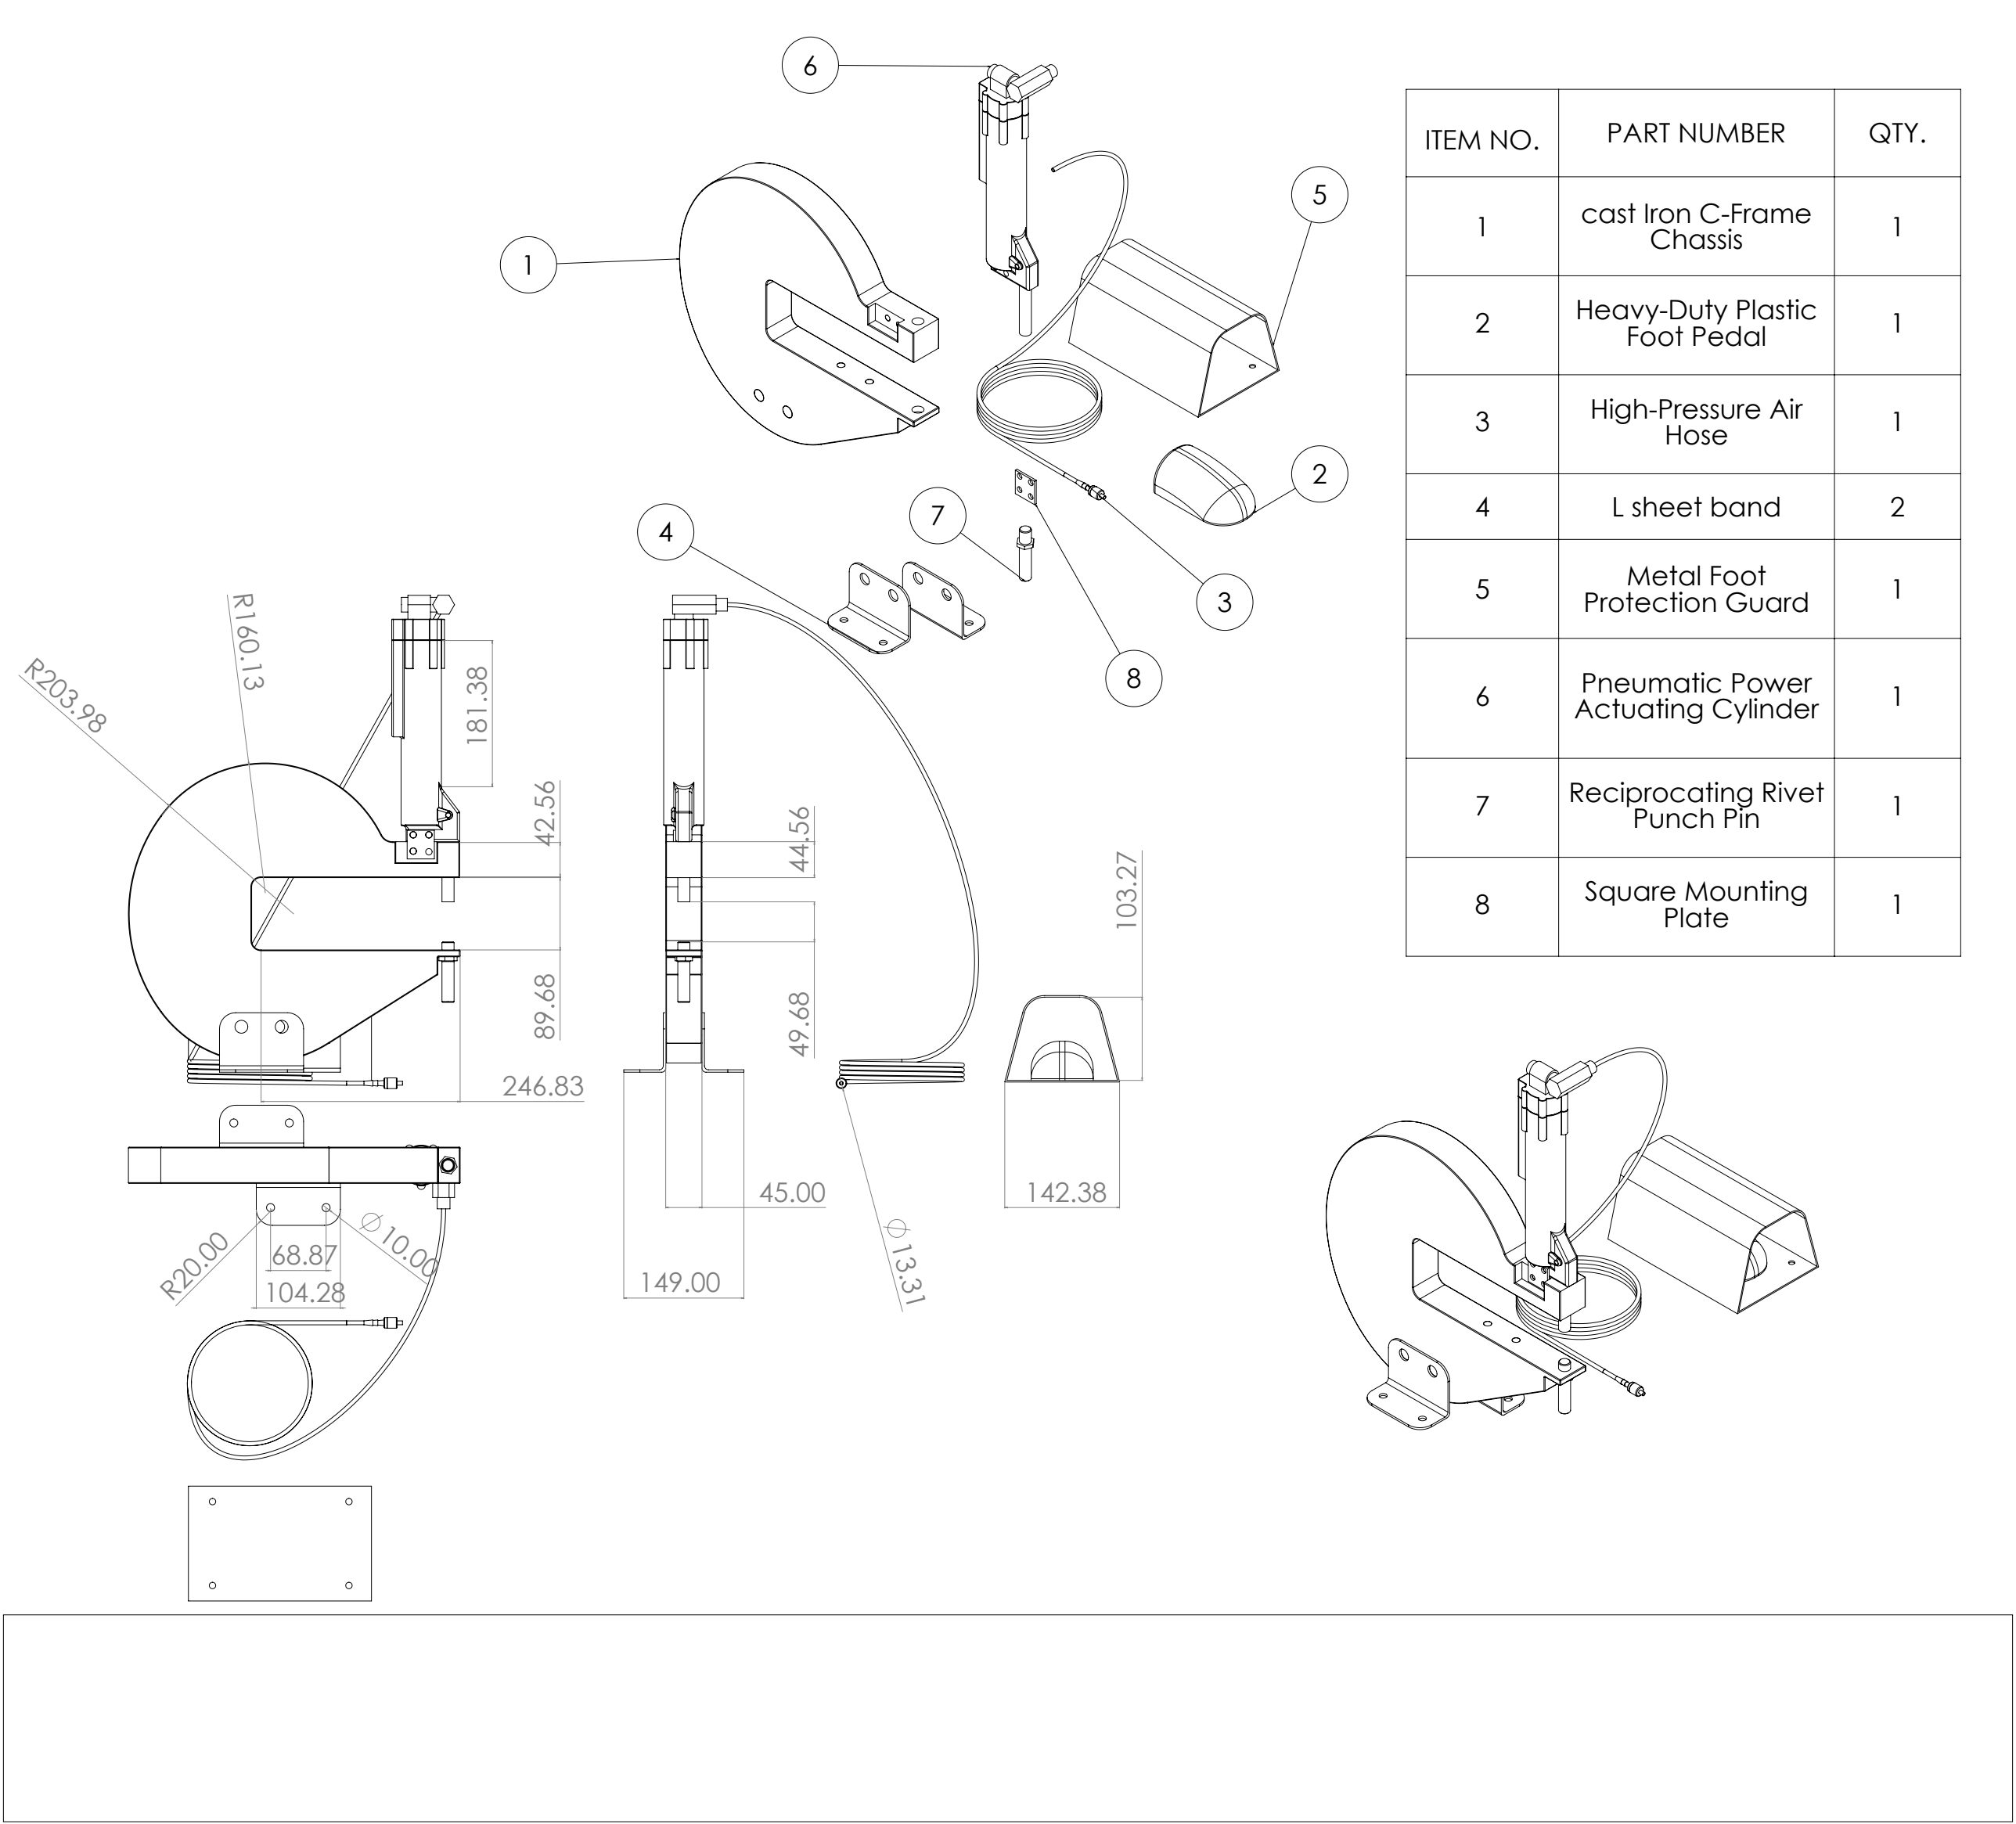
ISO-10303-21;
HEADER;
FILE_DESCRIPTION (('STEP AP214'),
    '1' );
FILE_NAME ('MAS-324',
    '2026-10-25T20:52:49',
    ( '' ),
    ( '' ),
    'SwSTEP 2.0',
    'SolidWorks 2025',
    '' );
FILE_SCHEMA (( 'AUTOMOTIVE_DESIGN' ));
ENDSEC;

DATA;
#1 = CARTESIAN_POINT ( 'NONE',  ( -113.6132551642233466, -295.8660902273127817, -261.0439986488574391 ) ) ;
#2 = CARTESIAN_POINT ( 'NONE',  ( -21.69829453939080111, -272.4952783879842286, -198.0198581616166962 ) ) ;
#3 = CARTESIAN_POINT ( 'NONE',  ( -77.14607672046975040, -275.6695791045739270, -333.3258523244866751 ) ) ;
#4 = CARTESIAN_POINT ( 'NONE',  ( -96.50722556860337420, -298.4744652489187047, -226.7430298893199279 ) ) ;
#5 = CARTESIAN_POINT ( 'NONE',  ( 35.29261755122405475, -294.8217676056252117, -258.4658906454228031 ) ) ;
#6 = DIRECTION ( 'NONE',  ( 0.000000000000000000, 1.000000000000000000, 0.000000000000000000 ) ) ;
#7 = CARTESIAN_POINT ( 'NONE',  ( 17.20777486049739124, -295.0510334597752831, -319.1340501124739717 ) ) ;
#8 = AXIS2_PLACEMENT_3D ( 'NONE', #62573, #33196, #12356 ) ;
#9 = CARTESIAN_POINT ( 'NONE',  ( -147.0026986695708047, -210.7421749798627673, -22.50000000000000000 ) ) ;
#11 = CARTESIAN_POINT ( 'NONE',  ( -84.47810206200919936, -295.7221423797171838, -326.1693894271719500 ) ) ;
#10 = CARTESIAN_POINT ( 'NONE',  ( 23.39288443123379579, -284.9668621146994951, -225.7548735365318748 ) ) ;
#12 = CARTESIAN_POINT ( 'NONE',  ( -83.27587881292458860, -285.4425543175578923, -208.4961557201596918 ) ) ;
#13 = CONICAL_SURFACE ( 'NONE', #77116, 24.00000000000001066, 0.7446590313522313265 ) ;
#14 = CARTESIAN_POINT ( 'NONE',  ( 24.12276456990134577, -287.8361799259163263, -316.7061702643556487 ) ) ;
#15 = CARTESIAN_POINT ( 'NONE',  ( -83.16459577638245548, -297.6555613683490265, -330.2488683299737886 ) ) ;
#16 = CARTESIAN_POINT ( 'NONE',  ( 12.16221636192367228, -290.7420802479286976, -214.1725176534357615 ) ) ;
#17 = CARTESIAN_POINT ( 'NONE',  ( -48.08606759839130973, -279.1160864900698471, -194.2237662435092886 ) ) ;
#18 = CARTESIAN_POINT ( 'NONE',  ( -110.4683760289727132, -293.8380690714490129, -287.0191576251351080 ) ) ;
#19 = LINE ( 'NONE', #14705, #54462 ) ;
#20 = CARTESIAN_POINT ( 'NONE',  ( 26.72141337091415991, -285.8585362577462661, -234.4374339655554991 ) ) ;
#21 = DIRECTION ( 'NONE',  ( -1.000000000000000000, -0.000000000000000000, -0.000000000000000000 ) ) ;
#22 = DIRECTION ( 'NONE',  ( -0.7957555401921980742, -0.6056179655966482667, 0.000000000000000000 ) ) ;
#23 = CARTESIAN_POINT ( 'NONE',  ( -111.0120785373717354, -298.2093386174307170, -265.9889607955867632 ) ) ;
#24 = CARTESIAN_POINT ( 'NONE',  ( -9.095926160855869469, -281.8396501160608523, -199.3626493647371376 ) ) ;
#26 = CARTESIAN_POINT ( 'NONE',  ( 24.14595339631129534, -281.7647060850542289, -309.8413200465337241 ) ) ;
#25 = CARTESIAN_POINT ( 'NONE',  ( -109.2360963732521952, -294.8641011722828580, -247.6139534407837743 ) ) ;
#27 = CARTESIAN_POINT ( 'NONE',  ( -106.5142501024570265, -297.1531912002984086, -236.5357083837597827 ) ) ;
#28 = EDGE_CURVE ( 'NONE', #72058, #65497, #786, .T. ) ;
#29 = CARTESIAN_POINT ( 'NONE',  ( -110.4578234273896271, -280.7667899122553763, -253.6568320815989921 ) ) ;
#30 = CARTESIAN_POINT ( 'NONE',  ( -93.78727130258138800, -296.2704692607680386, -223.6800016881232693 ) ) ;
#31 = VERTEX_POINT ( 'NONE', #14545 ) ;
#32 = DIRECTION ( 'NONE',  ( -0.8457827187922972723, -0.5335274993777825436, 0.000000000000000000 ) ) ;
#33 = CARTESIAN_POINT ( 'NONE',  ( -91.92744132223316456, -285.8159430608695288, -321.2751991526628785 ) ) ;
#34 = CARTESIAN_POINT ( 'NONE',  ( 143.2307367095235691, -26.41817448500847121, 22.50000000000000000 ) ) ;
#35 = CARTESIAN_POINT ( 'NONE',  ( -110.4542110544635705, -294.2666405000204577, -253.6410175316879361 ) ) ;
#36 = CARTESIAN_POINT ( 'NONE',  ( 16.83410871617971338, -275.5019898621288235, -324.9252248568274126 ) ) ;
#37 = CARTESIAN_POINT ( 'NONE',  ( -6.039705354571541562, -292.3087031825515965, -204.3989839164147782 ) ) ;
#38 = CARTESIAN_POINT ( 'NONE',  ( 33.63237012736230724, -283.3319559697839054, -290.1951570289018605 ) ) ;
#39 = CARTESIAN_POINT ( 'NONE',  ( 33.67317559943808192, -277.4154469211121636, -290.4904342910287482 ) ) ;
#40 = CARTESIAN_POINT ( 'NONE',  ( -68.83699650705307249, -285.0594432950156829, -339.7618826965099856 ) ) ;
#41 = CARTESIAN_POINT ( 'NONE',  ( 30.69690168102419747, -280.7137460309204471, -297.8907232790041348 ) ) ;
#42 = CARTESIAN_POINT ( 'NONE',  ( -110.7162897014109433, -280.3529109521358009, -285.8907753398488580 ) ) ;
#43 = CARTESIAN_POINT ( 'NONE',  ( -113.8629036840343218, -272.8260555190163927, -261.7875883216721036 ) ) ;
#44 = CARTESIAN_POINT ( 'NONE',  ( 36.88505382238304264, -275.6425748523263906, -290.8892655207978351 ) ) ;
#45 = CARTESIAN_POINT ( 'NONE',  ( 22.49833801616120255, -296.0810694518352193, -314.6384715069982576 ) ) ;
#46 = DIRECTION ( 'NONE',  ( -0.4999999999999952260, -0.8660254037844413721, 0.000000000000000000 ) ) ;
#47 = FACE_OUTER_BOUND ( 'NONE', #78112, .T. ) ;
#48 = EDGE_CURVE ( 'NONE', #2640, #65773, #51617, .T. ) ;
#49 = CARTESIAN_POINT ( 'NONE',  ( -61.22503046524085590, -293.4984592147682747, -342.3179306570231688 ) ) ;
#50 = CARTESIAN_POINT ( 'NONE',  ( -56.87203779738695175, -273.3011920805299724, -199.9055576269083190 ) ) ;
#51 = CARTESIAN_POINT ( 'NONE',  ( -39.21425765019228038, -293.5492008878248384, -194.0645109205592576 ) ) ;
#53 = CARTESIAN_POINT ( 'NONE',  ( -22.28692340252414539, -293.4457659912081908, -195.1980702719413614 ) ) ;
#52 = CARTESIAN_POINT ( 'NONE',  ( -72.08107566293803359, -300.1233781216987495, -198.2974183793908196 ) ) ;
#54 = CARTESIAN_POINT ( 'NONE',  ( 17.36828252781073800, -290.2692810089828868, -321.4942518745497182 ) ) ;
#55 = CARTESIAN_POINT ( 'NONE',  ( -112.2266234623324124, -276.5486602746883023, -270.6195867653905793 ) ) ;
#56 = CARTESIAN_POINT ( 'NONE',  ( -81.65742486183103210, -279.5809590698107172, -330.1727450829594659 ) ) ;
#57 = CARTESIAN_POINT ( 'NONE',  ( 35.17272386656721750, -291.8502700334059909, -287.2389789927554489 ) ) ;
#58 = CARTESIAN_POINT ( 'NONE',  ( 33.44209198229489743, -283.7601780698271341, -297.3788945958802969 ) ) ;
#59 = CARTESIAN_POINT ( 'NONE',  ( -109.8060437348913467, -283.3224215553644285, -281.7842631819470398 ) ) ;
#60 = ORIENTED_EDGE ( 'NONE', *, *, #32885, .T. ) ;
#61 = CARTESIAN_POINT ( 'NONE',  ( -71.42250952254038054, -283.1821142129608120, -334.9411916729687277 ) ) ;
#62 = CARTESIAN_POINT ( 'NONE',  ( -28.27524738754997813, -281.2441658516256098, -194.1546269278096304 ) ) ;
#63 = CARTESIAN_POINT ( 'NONE',  ( -113.4234760108877538, -283.4592184142248357, -261.4407986698293485 ) ) ;
#64 = CARTESIAN_POINT ( 'NONE',  ( -109.5114376524103363, -279.1602184646021101, -296.6766189074363638 ) ) ;
#65 = ADVANCED_FACE ( 'NONE', ( #14993 ), #6968, .F. ) ;
#66 = CARTESIAN_POINT ( 'NONE',  ( -97.37137399137552052, -279.4367685291730368, -317.4689306191668265 ) ) ;
#67 = CIRCLE ( 'NONE', #92305, 7.500000000000012434 ) ;
#68 = CARTESIAN_POINT ( 'NONE',  ( -6.941161984400275209, -297.1233781216987495, -333.4151289067050357 ) ) ;
#69 = ORIENTED_EDGE ( 'NONE', *, *, #59045, .F. ) ;
#70 = VERTEX_POINT ( 'NONE', #796 ) ;
#71 = CARTESIAN_POINT ( 'NONE',  ( -93.35509533216730915, -299.2464325822394926, -220.4862725388631191 ) ) ;
#72 = AXIS2_PLACEMENT_3D ( 'NONE', #82570, #38996, #88730 ) ;
#73 = CARTESIAN_POINT ( 'NONE',  ( -88.23497865206087454, -275.7892183208580263, -324.9662551183911319 ) ) ;
#74 = CARTESIAN_POINT ( 'NONE',  ( -102.3605472477040337, -292.8335325276641470, -230.9337581368000087 ) ) ;
#75 = CARTESIAN_POINT ( 'NONE',  ( 34.31805428248770795, -292.7103970009527529, -255.9121641687935949 ) ) ;
#76 = CARTESIAN_POINT ( 'NONE',  ( -96.34789938153127764, -289.3946153186523702, -319.7555901667715261 ) ) ;
#77 = DIRECTION ( 'NONE',  ( -0.000000000000000000, 1.000000000000000000, -0.000000000000000000 ) ) ;
#79 = CARTESIAN_POINT ( 'NONE',  ( -33.17331374697837987, -284.5052435883285966, -196.6285636872405860 ) ) ;
#78 = CARTESIAN_POINT ( 'NONE',  ( 36.88326735793300060, -292.3562425583122035, -288.5613484753777129 ) ) ;
#80 = CARTESIAN_POINT ( 'NONE',  ( -69.57500681174269630, -293.4837748164715094, -203.4749671060159528 ) ) ;
#81 = CARTESIAN_POINT ( 'NONE',  ( 22.22138339417639230, -283.4657779623778993, -313.4347628960813381 ) ) ;
#82 = CARTESIAN_POINT ( 'NONE',  ( -28.99082608718071796, -289.8901462222868872, -346.7236095928074064 ) ) ;
#83 = CARTESIAN_POINT ( 'NONE',  ( 34.39346676443356188, -281.8609718709653862, -256.4368729998031426 ) ) ;
#84 = CARTESIAN_POINT ( 'NONE',  ( 39.20951696572362977, -292.3824562929385706, -273.1753459359540557 ) ) ;
#85 = CARTESIAN_POINT ( 'NONE',  ( -4.393016225146153531, -289.4317384794202326, -339.7912944455955540 ) ) ;
#86 = CARTESIAN_POINT ( 'NONE',  ( 37.65823291392757000, -287.8290301222977519, -253.1405899415904912 ) ) ;
#87 = CARTESIAN_POINT ( 'NONE',  ( -52.09100773288315622, -286.0247242745892322, -198.8666571505329728 ) ) ;
#88 = EDGE_LOOP ( 'NONE', ( #36300, #74959 ) ) ;
#89 = DIRECTION ( 'NONE',  ( 0.000000000000000000, -0.000000000000000000, 1.000000000000000000 ) ) ;
#90 = CARTESIAN_POINT ( 'NONE',  ( 3.580403759654407825, -296.3688474698320192, -334.1856371305267430 ) ) ;
#91 = CARTESIAN_POINT ( 'NONE',  ( -113.1662103178394432, -295.1037629167083196, -280.9449385996212527 ) ) ;
#92 = EDGE_CURVE ( 'NONE', #64177, #39404, #21633, .T. ) ;
#93 = CARTESIAN_POINT ( 'NONE',  ( -83.57703501779413102, -278.4588845934780466, -213.5002235206053740 ) ) ;
#94 = CARTESIAN_POINT ( 'NONE',  ( -113.8008141857499993, -272.1671345119243028, -261.7861089057840900 ) ) ;
#95 = CARTESIAN_POINT ( 'NONE',  ( -103.3981541237931054, -294.5919941891141889, -303.1453271309203501 ) ) ;
#96 = CARTESIAN_POINT ( 'NONE',  ( 35.36480375133581333, -277.1321324331269693, -256.5141577024394337 ) ) ;
#97 = CARTESIAN_POINT ( 'NONE',  ( -54.47399014668751249, -271.9692736385993044, -198.1298912440302331 ) ) ;
#98 = CARTESIAN_POINT ( 'NONE',  ( 29.09142378860511258, -294.3365518058123484, -239.0359238687793777 ) ) ;
#99 = CARTESIAN_POINT ( 'NONE',  ( -75.80859898051943446, -296.6581450815154994, -332.8264140846681016 ) ) ;
#100 = CARTESIAN_POINT ( 'NONE',  ( -43.48489315514932230, -254.2578831974578009, -445.7297432066186502 ) ) ;
#101 = CARTESIAN_POINT ( 'NONE',  ( -85.24696079806301441, -293.7120025854050596, -328.2844675371921994 ) ) ;
#102 = CARTESIAN_POINT ( 'NONE',  ( -114.1802237732302245, -273.3548555386022372, -270.3713173946429720 ) ) ;
#103 = CARTESIAN_POINT ( 'NONE',  ( -94.45286519521168600, -275.2254758110098010, -221.7273418318577569 ) ) ;
#104 = CARTESIAN_POINT ( 'NONE',  ( -108.8900272069156472, -291.2871953198740016, -286.0477213144812936 ) ) ;
#105 = CARTESIAN_POINT ( 'NONE',  ( -4.323302397459051427, -294.9377782480969472, -335.5047827706411567 ) ) ;
#106 = CARTESIAN_POINT ( 'NONE',  ( -112.5882073356291926, -280.4803416563776182, -274.4070978670125669 ) ) ;
#107 = CARTESIAN_POINT ( 'NONE',  ( -108.0504587551557307, -277.6107128976585159, -241.1452023711554489 ) ) ;
#108 = CARTESIAN_POINT ( 'NONE',  ( -33.07270939256004993, -282.3483276930217585, -347.1537153405075173 ) ) ;
#109 = CARTESIAN_POINT ( 'NONE',  ( 15.96235870874075324, -274.1327303341880679, -214.9355814682232904 ) ) ;
#110 = CARTESIAN_POINT ( 'NONE',  ( -96.18649800141388084, -277.6093990147008412, -221.9287466249451199 ) ) ;
#111 = CARTESIAN_POINT ( 'NONE',  ( -61.43528157839729431, -277.7399057781236706, -199.1056149990290294 ) ) ;
#112 = CARTESIAN_POINT ( 'NONE',  ( -67.00311722930408109, -296.3398741006864157, -203.1056652694137199 ) ) ;
#113 = CARTESIAN_POINT ( 'NONE',  ( -33.55588428573118165, -276.0999399286864104, -195.4440965705611575 ) ) ;
#114 = PLANE ( 'NONE',  #30765 ) ;
#115 = CARTESIAN_POINT ( 'NONE',  ( 5.580496127948171292, -290.6504686268311843, -208.4249260671794843 ) ) ;
#116 = CARTESIAN_POINT ( 'NONE',  ( -112.2626902172997205, -290.3291827781827692, -288.1895695498705550 ) ) ;
#117 = CARTESIAN_POINT ( 'NONE',  ( -66.84020672111827821, -275.6666780896798059, -201.2245391158463406 ) ) ;
#118 = CARTESIAN_POINT ( 'NONE',  ( -41.95658063400141202, -295.9936855060223024, -195.6702128762018162 ) ) ;
#119 = CARTESIAN_POINT ( 'NONE',  ( -106.5292690430238025, -284.1790909977862043, -236.9359907930603981 ) ) ;
#120 = CARTESIAN_POINT ( 'NONE',  ( -37.35456021389456538, -284.0517986001094073, -195.3485413134038424 ) ) ;
#121 = DIRECTION ( 'NONE',  ( 0.000000000000000000, 0.7071067811865398012, 0.7071067811865552333 ) ) ;
#122 = CARTESIAN_POINT ( 'NONE',  ( 17.04267055929170738, -291.6439787220554649, -220.9968955086508515 ) ) ;
#123 = CARTESIAN_POINT ( 'NONE',  ( -62.96739064857778345, -283.8546313715036717, -200.6342915240590230 ) ) ;
#124 = CARTESIAN_POINT ( 'NONE',  ( 175.2296996224750103, 275.0000000000000568, 0.000000000000000000 ) ) ;
#125 = CARTESIAN_POINT ( 'NONE',  ( 208.4306832106271088, 20.44233620800389772, 0.000000000000000000 ) ) ;
#126 = CARTESIAN_POINT ( 'NONE',  ( 7.902484555432940816, -290.6701741179288092, -210.5450298619024636 ) ) ;
#127 = CARTESIAN_POINT ( 'NONE',  ( -89.97405692109779807, -282.2588973123018832, -325.6834086931719412 ) ) ;
#128 = CARTESIAN_POINT ( 'NONE',  ( -103.8431496891660544, -279.7226268398578668, -302.4792602913342421 ) ) ;
#129 = CARTESIAN_POINT ( 'NONE',  ( -65.74447246362868214, -286.8938844950662883, -199.2042825010933313 ) ) ;
#130 = CARTESIAN_POINT ( 'NONE',  ( -9.493390062269362772, -286.4264726012228266, -202.8681937675485756 ) ) ;
#131 = CARTESIAN_POINT ( 'NONE',  ( -94.04857214285830480, -279.3176295112319281, -317.2818740737955068 ) ) ;
#132 = CARTESIAN_POINT ( 'NONE',  ( -94.07220428401220147, -280.0074554778488505, -224.1631567100062625 ) ) ;
#133 = EDGE_CURVE ( 'NONE', #3915, #71428, #47386, .T. ) ;
#134 = CARTESIAN_POINT ( 'NONE',  ( -96.45200547131824464, -285.9190198393021092, -316.5235751886017397 ) ) ;
#135 = VERTEX_POINT ( 'NONE', #13608 ) ;
#136 = CARTESIAN_POINT ( 'NONE',  ( -46.12776598691637275, -297.7769461629130774, -193.8640261997899188 ) ) ;
#138 = CARTESIAN_POINT ( 'NONE',  ( -23.45499506039496396, -290.8538007153030662, -343.7556936576084468 ) ) ;
#137 = AXIS2_PLACEMENT_3D ( 'NONE', #66421, #57925, #65055 ) ;
#139 = DIRECTION ( 'NONE',  ( -0.000000000000000000, -0.000000000000000000, -1.000000000000000000 ) ) ;
#140 = ADVANCED_BREP_SHAPE_REPRESENTATION ( '', ( #90135, #18940 ), #43137 ) ;
#141 = CARTESIAN_POINT ( 'NONE',  ( -72.02372285203398405, -285.9805209788416391, -342.4524372437778652 ) ) ;
#142 = ORIENTED_EDGE ( 'NONE', *, *, #90775, .T. ) ;
#143 = CARTESIAN_POINT ( 'NONE',  ( 35.52797234631308498, -291.6693239864514453, -248.0799319934128278 ) ) ;
#144 = CARTESIAN_POINT ( 'NONE',  ( -9.246811333089969054, -287.9463490696106192, -202.2197728238365926 ) ) ;
#145 = CARTESIAN_POINT ( 'NONE',  ( 34.64086854919326441, -283.5370289157921775, -287.6338091762179943 ) ) ;
#146 = CARTESIAN_POINT ( 'NONE',  ( 23.68266680496880738, -289.5944490205463921, -316.3462561790806831 ) ) ;
#147 = CARTESIAN_POINT ( 'NONE',  ( -5.814316714654535367, -289.9613947498637572, -340.0699579485100230 ) ) ;
#148 = CARTESIAN_POINT ( 'NONE',  ( -108.8862810617042669, -286.2619989188776231, -292.8638642162096630 ) ) ;
#149 = CARTESIAN_POINT ( 'NONE',  ( -111.7315784639272209, -278.9682992199453224, -250.4319288396881689 ) ) ;
#150 = ORIENTED_EDGE ( 'NONE', *, *, #26082, .T. ) ;
#151 = CARTESIAN_POINT ( 'NONE',  ( 37.80224029141654540, -291.7390338754980235, -278.7595689655631759 ) ) ;
#152 = CARTESIAN_POINT ( 'NONE',  ( 36.17633980381252456, -281.0978762120507781, -247.4679353929731462 ) ) ;
#153 = CARTESIAN_POINT ( 'NONE',  ( -66.31674629447961422, -275.5291285280121656, -202.0141196464570328 ) ) ;
#154 = DIRECTION ( 'NONE',  ( 0.000000000000000000, 1.000000000000000000, 0.000000000000000000 ) ) ;
#155 = CARTESIAN_POINT ( 'NONE',  ( -20.25526795762937127, -294.7662352645559167, -195.3538533559490702 ) ) ;
#156 = CARTESIAN_POINT ( 'NONE',  ( -41.11966117830017708, -272.2452171050537686, -194.4168510268810053 ) ) ;
#157 = CYLINDRICAL_SURFACE ( 'NONE', #21355, 0.5000000000000004441 ) ;
#158 = CARTESIAN_POINT ( 'NONE',  ( -95.65708358510205755, -278.6778134938541598, -226.3255324265030310 ) ) ;
#159 = CARTESIAN_POINT ( 'NONE',  ( 38.33293935469181690, -276.6066984866882876, -258.3872807340205213 ) ) ;
#160 = CARTESIAN_POINT ( 'NONE',  ( -35.81830170358009724, -299.4968625532499118, -196.7715064960510745 ) ) ;
#161 = CARTESIAN_POINT ( 'NONE',  ( -70.37975053163600592, -282.5357189658061543, -339.6670035245268764 ) ) ;
#162 = CARTESIAN_POINT ( 'NONE',  ( -108.6968154583750703, -292.0538962897698525, -290.2073774136056272 ) ) ;
#163 = CARTESIAN_POINT ( 'NONE',  ( -35.86450529380874741, -299.5904438321611565, -194.0540724790644447 ) ) ;
#164 = CARTESIAN_POINT ( 'NONE',  ( -110.4388770307767373, -298.0485552961351345, -247.2764033145294036 ) ) ;
#165 = CARTESIAN_POINT ( 'NONE',  ( -15.02233590537950114, -296.7627049945999715, -341.8430372460552462 ) ) ;
#166 = CARTESIAN_POINT ( 'NONE',  ( -104.6730707308207968, -282.1193390125066003, -303.1377496322695038 ) ) ;
#167 = CARTESIAN_POINT ( 'NONE',  ( -113.9853605009663795, -290.3155259493814242, -262.6348601863189174 ) ) ;
#168 = CARTESIAN_POINT ( 'NONE',  ( -79.76971251359887560, -271.4959503811738273, -208.8840916564036263 ) ) ;
#169 = CARTESIAN_POINT ( 'NONE',  ( 2.307177052818977447, -288.1741521440539486, -205.2887970377841498 ) ) ;
#170 = CARTESIAN_POINT ( 'NONE',  ( -108.0463951965091098, -289.7272753538697998, -250.9943379319703922 ) ) ;
#171 = CARTESIAN_POINT ( 'NONE',  ( 201.3067182052938051, 288.2280244914530840, -97.39779909378675882 ) ) ;
#172 = ORIENTED_EDGE ( 'NONE', *, *, #18686, .T. ) ;
#173 = CARTESIAN_POINT ( 'NONE',  ( -109.8658504693686382, -289.4339475807516351, -246.1362763784779304 ) ) ;
#174 = CARTESIAN_POINT ( 'NONE',  ( -5.787136446112612020, -288.2921266566153236, -336.2124429329496706 ) ) ;
#175 = ORIENTED_EDGE ( 'NONE', *, *, #24191, .T. ) ;
#176 = CARTESIAN_POINT ( 'NONE',  ( -100.7487074920235273, -286.2040526672859073, -227.1274661871449609 ) ) ;
#177 = CARTESIAN_POINT ( 'NONE',  ( -69.25682644265404520, -277.8172129950345379, -336.0522927072145194 ) ) ;
#178 = CARTESIAN_POINT ( 'NONE',  ( 36.06976937112843729, -292.7541342344004534, -292.7275812612277264 ) ) ;
#179 = CARTESIAN_POINT ( 'NONE',  ( -38.72238868582785898, -283.7204533004693872, -347.2467895094548567 ) ) ;
#180 = CARTESIAN_POINT ( 'NONE',  ( -10.92373924738846114, -284.2341409807796140, -342.0049621938744622 ) ) ;
#181 = CARTESIAN_POINT ( 'NONE',  ( -94.38063292225054113, -284.1828072836642036, -322.0750035236984559 ) ) ;
#182 = CARTESIAN_POINT ( 'NONE',  ( 28.99011267871087938, -281.4722031727284275, -239.7083648369550417 ) ) ;
#183 = CARTESIAN_POINT ( 'NONE',  ( 180.6301689436333788, 254.0011452960685006, -166.8208226387889113 ) ) ;
#184 = CARTESIAN_POINT ( 'NONE',  ( 196.3077706885435134, 285.2721524738067274, -111.5570765633820969 ) ) ;
#185 = CARTESIAN_POINT ( 'NONE',  ( -90.09665665672530110, -228.8726286412962736, -344.7822526990161691 ) ) ;
#186 = CARTESIAN_POINT ( 'NONE',  ( -69.55286334857535735, -272.8140695680438057, -204.6721334301478521 ) ) ;
#187 = CARTESIAN_POINT ( 'NONE',  ( -11.36788948023329482, -273.3188565473291192, -201.7533031230518077 ) ) ;
#188 = CARTESIAN_POINT ( 'NONE',  ( -68.20725116294569546, -294.9544458090643957, -340.8369625160823375 ) ) ;
#189 = CARTESIAN_POINT ( 'NONE',  ( 6.867305562803349694, -59.82436178187390396, -351.3599612539230748 ) ) ;
#190 = CARTESIAN_POINT ( 'NONE',  ( -66.02668222974523360, -272.3693846100331939, -199.4212332350789154 ) ) ;
#191 = CARTESIAN_POINT ( 'NONE',  ( -37.17015063146384790, -299.9147455406174458, -196.1229585654807863 ) ) ;
#192 = CARTESIAN_POINT ( 'NONE',  ( 19.90811401000262038, -289.5144666564462455, -316.4447621617657092 ) ) ;
#193 = ORIENTED_EDGE ( 'NONE', *, *, #5103, .F. ) ;
#194 = CARTESIAN_POINT ( 'NONE',  ( -70.69477044455324233, -296.4224833217160153, -339.5159684217153426 ) ) ;
#195 = CARTESIAN_POINT ( 'NONE',  ( 17.81853407656373633, -287.3620640795646182, -222.4514425058484051 ) ) ;
#196 = CARTESIAN_POINT ( 'NONE',  ( -58.02497702157741344, -272.7114924129007250, -196.4567845684104839 ) ) ;
#197 = CARTESIAN_POINT ( 'NONE',  ( 36.21809064911852261, -294.6363344162023736, -292.7476569483883964 ) ) ;
#198 = CARTESIAN_POINT ( 'NONE',  ( -104.5460947458797278, -296.5572545471907802, -307.9279408047181050 ) ) ;
#199 = CARTESIAN_POINT ( 'NONE',  ( -110.3370228416248295, -290.7079322884769113, -271.1874753075676949 ) ) ;
#200 = VERTEX_POINT ( 'NONE', #71848 ) ;
#201 = CARTESIAN_POINT ( 'NONE',  ( -69.54077655466207375, -275.5518863169126007, -201.9910387382556678 ) ) ;
#202 = CARTESIAN_POINT ( 'NONE',  ( 38.34100351736458379, -274.5000774477773575, -282.5315648924769221 ) ) ;
#203 = EDGE_CURVE ( 'NONE', #23354, #33474, #15867, .T. ) ;
#204 = ORIENTED_EDGE ( 'NONE', *, *, #14407, .T. ) ;
#205 = CARTESIAN_POINT ( 'NONE',  ( -104.9245238535658160, -277.5835944543852634, -307.1318786540637120 ) ) ;
#206 = PRODUCT_DEFINITION_CONTEXT ( 'detailed design', #57764, 'design' ) ;
#207 = CARTESIAN_POINT ( 'NONE',  ( 31.87562710300615620, -273.6143523044818266, -244.7602971938240444 ) ) ;
#208 = CARTESIAN_POINT ( 'NONE',  ( -108.8394098029810380, -273.8445740299966928, -254.1653288387956025 ) ) ;
#209 = CARTESIAN_POINT ( 'NONE',  ( -1.618296635492913360, -275.4792631490921053, -206.4151797416647582 ) ) ;
#210 = CARTESIAN_POINT ( 'NONE',  ( -31.36245263867117217, -275.8867941206686396, -194.5969546141441526 ) ) ;
#211 = CIRCLE ( 'NONE', #62253, 4.999999999999997335 ) ;
#212 = CARTESIAN_POINT ( 'NONE',  ( 20.45256449681794564, -274.2372513224178761, -318.7163636411478933 ) ) ;
#213 = CARTESIAN_POINT ( 'NONE',  ( -26.18367686562210039, -295.5577560403836515, -342.6064720533350396 ) ) ;
#214 = CARTESIAN_POINT ( 'NONE',  ( 35.49350546835615461, -291.9893731014084892, -259.8536090943885597 ) ) ;
#215 = DIRECTION ( 'NONE',  ( 0.000000000000000000, 1.000000000000000000, 0.000000000000000000 ) ) ;
#216 = CARTESIAN_POINT ( 'NONE',  ( -102.0418390638001398, -278.4966892230997360, -312.0926700045682196 ) ) ;
#217 = CARTESIAN_POINT ( 'NONE',  ( 34.12090894609900005, -275.5214342262589753, -255.3972326369435280 ) ) ;
#218 = CARTESIAN_POINT ( 'NONE',  ( -26.67319746492361787, -284.8698424366841664, -194.5485961385973042 ) ) ;
#219 = CARTESIAN_POINT ( 'NONE',  ( -69.98802764187368552, -297.4812203234077970, -338.0823389745905843 ) ) ;
#220 = CARTESIAN_POINT ( 'NONE',  ( 211.4629471475955427, 32.98517505407394168, 10.00000000000000000 ) ) ;
#221 = CARTESIAN_POINT ( 'NONE',  ( -95.07820106282620998, -284.3812749118341685, -225.4064025234517032 ) ) ;
#222 = CARTESIAN_POINT ( 'NONE',  ( -62.15031415579434082, -275.6189368971078579, -340.1472874860159550 ) ) ;
#223 = CARTESIAN_POINT ( 'NONE',  ( -95.75169594866139278, -276.5021968402988364, -315.1232370903478568 ) ) ;
#224 = CARTESIAN_POINT ( 'NONE',  ( -110.1547686304307092, -286.7838384147241300, -252.3291687126599356 ) ) ;
#225 = CARTESIAN_POINT ( 'NONE',  ( 5.641680306182056626, -277.6606581397782065, -329.9180858645652279 ) ) ;
#226 = CARTESIAN_POINT ( 'NONE',  ( 219.8344101925596021, 35.72494958537217968, 7.000000000000000000 ) ) ;
#227 = CARTESIAN_POINT ( 'NONE',  ( 16.37664934189118426, -274.7048225403960942, -324.4790114041376796 ) ) ;
#228 = CARTESIAN_POINT ( 'NONE',  ( 34.80913351221764174, -276.3624349405349108, -282.4209052261880402 ) ) ;
#229 = CARTESIAN_POINT ( 'NONE',  ( 2.820361398021606458, -282.5894332162787350, -206.7619648397659091 ) ) ;
#230 = CARTESIAN_POINT ( 'NONE',  ( 201.2509219215139922, 65.09645894978946501, 0.000000000000000000 ) ) ;
#231 = CARTESIAN_POINT ( 'NONE',  ( 34.47262405957937403, -289.1691442991094618, -246.6989133634617701 ) ) ;
#232 = CARTESIAN_POINT ( 'NONE',  ( 21.86556464674976041, -292.1835024172012822, -316.4195789663704090 ) ) ;
#233 = DIRECTION ( 'NONE',  ( -0.000000000000000000, 0.000000000000000000, -1.000000000000000000 ) ) ;
#234 = CARTESIAN_POINT ( 'NONE',  ( -41.87763380309878869, -296.7886418773014725, -197.1043380165232293 ) ) ;
#235 = CARTESIAN_POINT ( 'NONE',  ( -106.8591441079072695, -289.0350993510990065, -244.1732922129692724 ) ) ;
#236 = CARTESIAN_POINT ( 'NONE',  ( -114.4693268140674434, -273.6886850827510216, -284.2063049943780015 ) ) ;
#237 = CARTESIAN_POINT ( 'NONE',  ( 196.8803347170859865, 73.40565171261609123, -12.49999999999998579 ) ) ;
#238 = CARTESIAN_POINT ( 'NONE',  ( -23.45726847500185741, -287.3577760870506950, -345.4476048667748955 ) ) ;
#239 = CARTESIAN_POINT ( 'NONE',  ( -33.75247087138109237, -284.3366009130915018, -194.4592639308252728 ) ) ;
#240 = CARTESIAN_POINT ( 'NONE',  ( -78.69286312455705001, -285.0466963355058851, -331.2335767372052260 ) ) ;
#241 = CARTESIAN_POINT ( 'NONE',  ( -107.9142151825760436, -285.1001298097412473, -289.6988518128527517 ) ) ;
#242 = CARTESIAN_POINT ( 'NONE',  ( -50.30864909105871163, -293.8672956765573758, -196.1299585228881313 ) ) ;
#243 = CARTESIAN_POINT ( 'NONE',  ( -66.22322631712503949, -274.0175736708989689, -198.9914908511120188 ) ) ;
#244 = CARTESIAN_POINT ( 'NONE',  ( -82.02121176197549346, -287.7358496163018913, -331.2959638059363101 ) ) ;
#245 = CARTESIAN_POINT ( 'NONE',  ( -99.64976321348814281, -277.9516674045289619, -315.6240650913662762 ) ) ;
#246 = CARTESIAN_POINT ( 'NONE',  ( 31.35993196141822281, -295.1472400932031519, -241.0411030402186157 ) ) ;
#247 = CARTESIAN_POINT ( 'NONE',  ( -48.18343439339132317, -269.7948820652942459, -438.7219023890238532 ) ) ;
#248 = CARTESIAN_POINT ( 'NONE',  ( 35.78497577281001440, -296.2662352645559167, -287.0191576251351080 ) ) ;
#249 = CARTESIAN_POINT ( 'NONE',  ( -18.62610965303630906, -281.4909754024122890, -341.4840500770574181 ) ) ;
#250 = EDGE_CURVE ( 'NONE', #25460, #78927, #7415, .T. ) ;
#251 = CARTESIAN_POINT ( 'NONE',  ( -39.50340962879238305, -278.0248805946041557, -195.3795613189264202 ) ) ;
#252 = ADVANCED_FACE ( 'NONE', ( #16740 ), #65214, .F. ) ;
#253 = CARTESIAN_POINT ( 'NONE',  ( -97.25653598327876637, -271.6698244868129564, -223.1073329477313791 ) ) ;
#254 = CARTESIAN_POINT ( 'NONE',  ( 34.47519203589411774, -274.7209678462776878, -256.7146287507716806 ) ) ;
#255 = CARTESIAN_POINT ( 'NONE',  ( -0.9307921106466295891, -294.0650048284701370, -206.2765958823960943 ) ) ;
#256 = CARTESIAN_POINT ( 'NONE',  ( 34.55765642826714412, -294.6765038290132566, -284.2855919575040389 ) ) ;
#257 = CARTESIAN_POINT ( 'NONE',  ( 37.74284114224520437, -294.7987799472403481, -256.1865648562181832 ) ) ;
#258 = CARTESIAN_POINT ( 'NONE',  ( 37.27658265588780040, -294.6540076195757933, -253.4083519683468353 ) ) ;
#259 = CARTESIAN_POINT ( 'NONE',  ( -108.8851482201205414, -296.1932415551128202, -284.9332040079801800 ) ) ;
#260 = CARTESIAN_POINT ( 'NONE',  ( -111.3897608342564070, -292.3983347659790866, -282.3532917929296673 ) ) ;
#261 = CARTESIAN_POINT ( 'NONE',  ( -41.56701483115121221, -283.2705272460136712, -347.2974267954927541 ) ) ;
#262 = CARTESIAN_POINT ( 'NONE',  ( -18.82848769330092153, -272.4274859315958111, -196.8388344709858018 ) ) ;
#263 = CARTESIAN_POINT ( 'NONE',  ( 22.99321104538541860, -286.7450741532542224, -222.4997577815586851 ) ) ;
#264 = CARTESIAN_POINT ( 'NONE',  ( -92.15899064099502880, -279.8196800380848686, -321.1009690803662124 ) ) ;
#265 = CARTESIAN_POINT ( 'NONE',  ( -8.150179586038067470, -285.5028795466129736, -203.1951773795938152 ) ) ;
#266 = EDGE_CURVE ( 'NONE', #10377, #27540, #29202, .T. ) ;
#267 = CARTESIAN_POINT ( 'NONE',  ( -77.09840566266530004, -287.5843468112212804, -334.0173477355417617 ) ) ;
#268 = CARTESIAN_POINT ( 'NONE',  ( -45.12257076738355721, -278.0943342815326105, -194.9447721771423971 ) ) ;
#270 = CIRCLE ( 'NONE', #69816, 1.000000000000001998 ) ;
#269 = CARTESIAN_POINT ( 'NONE',  ( -107.8893720497363518, -252.3744610414916565, -325.2219058921743908 ) ) ;
#271 = CARTESIAN_POINT ( 'NONE',  ( -103.0707657646160413, -283.6269096832978107, -302.3783997235955212 ) ) ;
#272 = AXIS2_PLACEMENT_3D ( 'NONE', #89516, #54022, #33648 ) ;
#273 = CARTESIAN_POINT ( 'NONE',  ( 37.16576817676342159, -282.9815768181842373, -288.2116639322431979 ) ) ;
#274 = CARTESIAN_POINT ( 'NONE',  ( -4.444799110440903256, -287.6879362380452108, -339.7341427214811347 ) ) ;
#275 = CARTESIAN_POINT ( 'NONE',  ( -111.3928543446432258, -279.9245025573324597, -288.3842106415503395 ) ) ;
#276 = CARTESIAN_POINT ( 'NONE',  ( -48.40600831671226700, -278.5052016875781078, -346.1172373858461242 ) ) ;
#277 = CARTESIAN_POINT ( 'NONE',  ( -92.20703582126834874, -279.0729676217148949, -222.1882355758204994 ) ) ;
#278 = CARTESIAN_POINT ( 'NONE',  ( -79.81114824688718556, -275.4550972370517457, -208.9127111854542704 ) ) ;
#279 = CARTESIAN_POINT ( 'NONE',  ( 33.32439624573670045, -293.1624354433766939, -239.7783969903679804 ) ) ;
#280 = CARTESIAN_POINT ( 'NONE',  ( -23.50445829584242219, -286.8946535863967711, -343.7650351519840797 ) ) ;
#281 = AXIS2_PLACEMENT_3D ( 'NONE', #4079, #26316, #18275 ) ;
#282 = CARTESIAN_POINT ( 'NONE',  ( -70.56748717621604783, -293.2214596486516598, -201.7864324643425675 ) ) ;
#283 = CARTESIAN_POINT ( 'NONE',  ( -108.4715376898812877, -295.7062291228027675, -252.5679424721457451 ) ) ;
#284 = CARTESIAN_POINT ( 'NONE',  ( -15.59057583108496203, -294.4296390795713592, -340.1206596468418297 ) ) ;
#285 = CARTESIAN_POINT ( 'NONE',  ( -77.02114960951715261, -292.6137018445027707, -204.6718712135360647 ) ) ;
#286 = CARTESIAN_POINT ( 'NONE',  ( 7.197872772093760751, -281.3285238675737787, -212.3305421225269640 ) ) ;
#287 = CARTESIAN_POINT ( 'NONE',  ( -31.92281438307887598, -297.0388370913102563, -193.6711941998320015 ) ) ;
#288 = CARTESIAN_POINT ( 'NONE',  ( -105.0622752010226577, -290.7319065036531924, -306.7923751401537515 ) ) ;
#289 = CARTESIAN_POINT ( 'NONE',  ( -87.52147800885803974, -281.8828391876222099, -327.1964541124606853 ) ) ;
#290 = CARTESIAN_POINT ( 'NONE',  ( -114.1670047289575791, -290.9462267493518084, -265.5013994278262999 ) ) ;
#291 = EDGE_CURVE ( 'NONE', #59112, #73985, #48974, .T. ) ;
#292 = CARTESIAN_POINT ( 'NONE',  ( -17.17010717937488096, -286.6529688014165345, -200.1285271177430332 ) ) ;
#293 = CARTESIAN_POINT ( 'NONE',  ( 169.2494399300530290, -11.64849832608277325, -3.999999999999998224 ) ) ;
#294 = CARTESIAN_POINT ( 'NONE',  ( -113.9112430796897115, -271.1015500560408213, -283.8576724739366455 ) ) ;
#295 = CARTESIAN_POINT ( 'NONE',  ( -39.22682415819677715, -139.9825792601168644, -360.8488084492784083 ) ) ;
#296 = CARTESIAN_POINT ( 'NONE',  ( -94.91159530925413890, -278.3846945089381961, -225.1933234040334071 ) ) ;
#297 = CARTESIAN_POINT ( 'NONE',  ( -67.42059858149401919, -278.5684387154228716, -203.4932414482983347 ) ) ;
#298 = CARTESIAN_POINT ( 'NONE',  ( 18.07732448069620190, -274.4864427186229250, -216.8572984162106252 ) ) ;
#299 = CARTESIAN_POINT ( 'NONE',  ( -92.64007872224544826, -240.2551808938772240, -339.7428190326851905 ) ) ;
#300 = CARTESIAN_POINT ( 'NONE',  ( -95.44584374818370520, -277.8015992959548726, -220.7172953016149393 ) ) ;
#301 = CARTESIAN_POINT ( 'NONE',  ( -68.49327023195247932, -281.4836232829917435, -338.1949331952813509 ) ) ;
#302 = CARTESIAN_POINT ( 'NONE',  ( 10.57689206411022553, -296.1611599144177376, -329.4016677618776612 ) ) ;
#303 = CARTESIAN_POINT ( 'NONE',  ( -37.55642042354166676, -292.5417769992668582, -197.2874406787996691 ) ) ;
#304 = CARTESIAN_POINT ( 'NONE',  ( 23.91132114415732346, -286.7970199167970122, -310.9958052702095870 ) ) ;
#305 = CARTESIAN_POINT ( 'NONE',  ( 25.23911174490946863, -275.6105727896177768, -225.6512951641706479 ) ) ;
#306 = CARTESIAN_POINT ( 'NONE',  ( -91.84630622800007416, -297.4132482821498797, -221.7993231391932341 ) ) ;
#307 = VERTEX_POINT ( 'NONE', #19143 ) ;
#308 = DIRECTION ( 'NONE',  ( 0.000000000000000000, 0.000000000000000000, -1.000000000000000000 ) ) ;
#309 = CARTESIAN_POINT ( 'NONE',  ( 196.7084708347797459, 24.79057925319257194, 12.79847700770043950 ) ) ;
#310 = CARTESIAN_POINT ( 'NONE',  ( -50.70934710825899572, -281.8028321744117193, -195.9929782340904580 ) ) ;
#311 = CARTESIAN_POINT ( 'NONE',  ( -27.53056093681999172, -281.2592550515166749, -197.6600890250774967 ) ) ;
#312 = CARTESIAN_POINT ( 'NONE',  ( -31.17860052041886831, -281.8889978174094040, -194.5728002490756694 ) ) ;
#313 = CARTESIAN_POINT ( 'NONE',  ( -5.942905713229805542, -281.6877908578424581, -336.5377726664386273 ) ) ;
#314 = CARTESIAN_POINT ( 'NONE',  ( 21.24440329897678836, -273.4090717797046182, -225.6371385638898062 ) ) ;
#315 = CARTESIAN_POINT ( 'NONE',  ( 209.2565306692229683, 27.88187848093107846, 12.07105558346639462 ) ) ;
#316 = CARTESIAN_POINT ( 'NONE',  ( 139.6925840978351516, -0.9999999999999859002, -21.50000000000000000 ) ) ;
#317 = CARTESIAN_POINT ( 'NONE',  ( 28.96178146475818593, -276.8614997905642667, -309.1941857057189509 ) ) ;
#318 = DIRECTION ( 'NONE',  ( -0.000000000000000000, -1.000000000000000000, -0.000000000000000000 ) ) ;
#319 = CARTESIAN_POINT ( 'NONE',  ( 4.769913331632007036, -278.4835506822664115, -332.4224800237890918 ) ) ;
#320 = CARTESIAN_POINT ( 'NONE',  ( -39.96107325075033145, -275.6591585686044255, -346.7399479336539230 ) ) ;
#321 = ORIENTED_EDGE ( 'NONE', *, *, #79781, .T. ) ;
#322 = LINE ( 'NONE', #6506, #611 ) ;
#323 = CARTESIAN_POINT ( 'NONE',  ( -52.56024909002068313, -285.2259183838634158, -344.2168985579138507 ) ) ;
#324 = CARTESIAN_POINT ( 'NONE',  ( 28.53551074124957410, -293.1804526957525354, -302.3023540898434476 ) ) ;
#325 = CARTESIAN_POINT ( 'NONE',  ( 26.27770430026630777, -286.3302106616349647, -227.1417106107467703 ) ) ;
#326 = CARTESIAN_POINT ( 'NONE',  ( -87.63360837066642262, -282.0053727907281882, -324.7331695838644805 ) ) ;
#327 = CARTESIAN_POINT ( 'NONE',  ( -34.84458204204858589, -281.5949315533735557, -343.9205063545541066 ) ) ;
#328 = CARTESIAN_POINT ( 'NONE',  ( 25.90896429186087957, -283.2670875563693471, -307.6971038925671564 ) ) ;
#329 = CARTESIAN_POINT ( 'NONE',  ( -24.47694389544438565, -272.2160532552937866, -196.4199350418342647 ) ) ;
#330 = AXIS2_PLACEMENT_3D ( 'NONE', #82535, #75438, #88694 ) ;
#331 = CARTESIAN_POINT ( 'NONE',  ( -110.7265842235424458, -282.6921952033420098, -290.8818197932454837 ) ) ;
#332 = CARTESIAN_POINT ( 'NONE',  ( -58.26820715863784272, -297.3226295211096044, -342.4366403366163922 ) ) ;
#333 = AXIS2_PLACEMENT_3D ( 'NONE', #2350, #57785, #47737 ) ;
#334 = CARTESIAN_POINT ( 'NONE',  ( -85.64834529566002175, -280.3052127297970628, -215.3168041969837248 ) ) ;
#335 = CARTESIAN_POINT ( 'NONE',  ( -5.572524851392624434, -288.4691924952029467, -202.2380827223223321 ) ) ;
#336 = CARTESIAN_POINT ( 'NONE',  ( 197.2699694956033341, 291.3106288012165805, -7.550674042187431212 ) ) ;
#337 = DIRECTION ( 'NONE',  ( -0.000000000000000000, -1.000000000000000000, -0.000000000000000000 ) ) ;
#338 = CARTESIAN_POINT ( 'NONE',  ( 23.63759464484336092, -294.8685903048981345, -225.7422900162428050 ) ) ;
#339 = AXIS2_PLACEMENT_3D ( 'NONE', #18506, #54487, #77693 ) ;
#340 = CARTESIAN_POINT ( 'NONE',  ( -39.23304639640969782, -275.0757377487332178, -345.3372706006049384 ) ) ;
#341 = CARTESIAN_POINT ( 'NONE',  ( -112.9761763116332247, -289.5785814991315874, -283.9848390634267048 ) ) ;
#342 = CARTESIAN_POINT ( 'NONE',  ( 21.95725545762149977, -292.5613560969318314, -314.2937286855417938 ) ) ;
#343 = CARTESIAN_POINT ( 'NONE',  ( -85.44055784739148862, -276.4180553261052182, -325.9960111145832116 ) ) ;
#344 = CARTESIAN_POINT ( 'NONE',  ( -95.72722165873599920, -271.2710829947001230, -224.1827130997946256 ) ) ;
#345 = CARTESIAN_POINT ( 'NONE',  ( -22.65836053330757238, -293.5592278193776679, -198.3497090604275854 ) ) ;
#346 = CARTESIAN_POINT ( 'NONE',  ( -69.85430415644619018, -285.9805209788416391, -337.9475929042657754 ) ) ;
#347 = CARTESIAN_POINT ( 'NONE',  ( -36.30347657727352129, -293.5192792618893236, -346.6737098085878870 ) ) ;
#348 = CARTESIAN_POINT ( 'NONE',  ( -72.72470772363107017, -291.1292060606908194, -335.1259478652599455 ) ) ;
#349 = CARTESIAN_POINT ( 'NONE',  ( -72.93889733817584897, -289.8270235111069155, -203.2136108133159951 ) ) ;
#350 = CARTESIAN_POINT ( 'NONE',  ( 21.65667839415024787, -289.5898385970144204, -314.3659227384940777 ) ) ;
#351 = CARTESIAN_POINT ( 'NONE',  ( 152.0879868122481184, 129.8824796955493355, -12.50000000000000178 ) ) ;
#352 = CARTESIAN_POINT ( 'NONE',  ( -84.78198129953274531, -290.5284216945488538, -326.1237722561434111 ) ) ;
#353 = CARTESIAN_POINT ( 'NONE',  ( 184.7149167944524493, -12.49482340714361506, 10.00000000000000000 ) ) ;
#354 = CARTESIAN_POINT ( 'NONE',  ( 16.41828331231947047, -289.5142829697366551, -325.0047850796670446 ) ) ;
#355 = CARTESIAN_POINT ( 'NONE',  ( -69.24261951150045036, -277.6547478299956424, -202.0774387024998475 ) ) ;
#356 = CARTESIAN_POINT ( 'NONE',  ( -93.06138155620693908, -279.6124719458072718, -217.1712879536569858 ) ) ;
#357 = CARTESIAN_POINT ( 'NONE',  ( -2.906107825339117934, -282.2763205639810167, -339.2229474479840405 ) ) ;
#358 = CARTESIAN_POINT ( 'NONE',  ( 32.85528928337881638, -285.2072911852064863, -243.8063626278319873 ) ) ;
#359 = CARTESIAN_POINT ( 'NONE',  ( 196.0143093133015384, 42.36571313990103960, 11.99999999999998934 ) ) ;
#360 = CARTESIAN_POINT ( 'NONE',  ( 16.70922893827216171, -280.4128521477969116, -321.3210328012327182 ) ) ;
#361 = ADVANCED_FACE ( 'NONE', ( #13917 ), #24780, .F. ) ;
#362 = CARTESIAN_POINT ( 'NONE',  ( -66.39029194718750659, -283.6716376159805009, -201.2150409871211707 ) ) ;
#363 = CARTESIAN_POINT ( 'NONE',  ( 122.1069165698472005, 147.2784710008442062, -260.4370889626021608 ) ) ;
#364 = CARTESIAN_POINT ( 'NONE',  ( -97.39534768318327451, -276.3970167199631760, -317.4383648314011452 ) ) ;
#365 = CARTESIAN_POINT ( 'NONE',  ( -89.66526190333848945, -284.2554813913510543, -214.2198617431564287 ) ) ;
#366 = CARTESIAN_POINT ( 'NONE',  ( -76.65960139014248398, -274.3138574429952996, -208.6626223191690030 ) ) ;
#367 = CARTESIAN_POINT ( 'NONE',  ( -110.4121956192968952, -292.0160383064796861, -280.8026003379728195 ) ) ;
#368 = CARTESIAN_POINT ( 'NONE',  ( -64.70614803693948147, -275.1270252510786349, -199.0042521874292731 ) ) ;
#369 = CARTESIAN_POINT ( 'NONE',  ( 31.13961632253437628, -274.8809954078292321, -245.0155703673037237 ) ) ;
#370 = CARTESIAN_POINT ( 'NONE',  ( -31.41970177568762068, -296.9776604953191281, -345.1784422849063390 ) ) ;
#371 = CARTESIAN_POINT ( 'NONE',  ( -65.44504524589291350, -289.5761160872477262, -342.1056879275396909 ) ) ;
#372 = CARTESIAN_POINT ( 'NONE',  ( 36.45377266294208596, -279.8396616290869474, -286.6547727834441162 ) ) ;
#373 = CARTESIAN_POINT ( 'NONE',  ( 20.38009769833850271, -292.6951850229471574, -219.3785238948976826 ) ) ;
#374 = CARTESIAN_POINT ( 'NONE',  ( -32.12861129292866735, -291.1782324718648169, -197.2989384837379987 ) ) ;
#375 = CARTESIAN_POINT ( 'NONE',  ( -41.85144338877410064, -293.1086862314667201, -345.2764462107752479 ) ) ;
#376 = ORIENTED_EDGE ( 'NONE', *, *, #4713, .F. ) ;
#377 = CARTESIAN_POINT ( 'NONE',  ( 0.000000000000000000, 131.0000000000000568, -11.50000000000000000 ) ) ;
#378 = CARTESIAN_POINT ( 'NONE',  ( -81.76149366879960212, -290.9364281575888072, -212.2895999433750660 ) ) ;
#379 = CARTESIAN_POINT ( 'NONE',  ( 207.5838500149071706, 29.29481134328564451, 13.58522159759120740 ) ) ;
#380 = CARTESIAN_POINT ( 'NONE',  ( -15.49194037015495340, -287.2693386610928314, -196.7164407258930510 ) ) ;
#381 = CARTESIAN_POINT ( 'NONE',  ( -53.35057174420112602, -300.3376638359844719, -200.3683826091709648 ) ) ;
#382 = CARTESIAN_POINT ( 'NONE',  ( -5.905052913589146080, -293.7076358184812648, -340.3936634569377588 ) ) ;
#383 = CARTESIAN_POINT ( 'NONE',  ( -100.9994486081661194, -285.3040589295532072, -312.8942100776160942 ) ) ;
#384 = CARTESIAN_POINT ( 'NONE',  ( -87.69296771485265651, -285.1580413244751639, -217.5051830566009698 ) ) ;
#385 = CARTESIAN_POINT ( 'NONE',  ( 27.23484507803531329, -276.5905825887086280, -234.7502008270885199 ) ) ;
#386 = CARTESIAN_POINT ( 'NONE',  ( 33.90947907481013601, -291.8606329916426034, -292.6123261580082158 ) ) ;
#387 = CARTESIAN_POINT ( 'NONE',  ( 23.78235592887573091, -295.8861003879378586, -312.1859408948212149 ) ) ;
#388 = CARTESIAN_POINT ( 'NONE',  ( 34.27735924785553578, -274.5585016382564731, -286.4756392014268158 ) ) ;
#389 = ORIENTED_EDGE ( 'NONE', *, *, #16197, .T. ) ;
#390 = CARTESIAN_POINT ( 'NONE',  ( 195.6182592083429768, 42.27466702580179714, 12.66657019004900953 ) ) ;
#391 = CARTESIAN_POINT ( 'NONE',  ( 1.755039088397472469, -294.2108378408647127, -336.6724237618244047 ) ) ;
#392 = CARTESIAN_POINT ( 'NONE',  ( 36.55663044536660067, -289.5882713313104659, -279.3249863250336489 ) ) ;
#393 = CARTESIAN_POINT ( 'NONE',  ( 27.34393682368281375, -296.8617045556625271, -195.3831644147898032 ) ) ;
#394 = CARTESIAN_POINT ( 'NONE',  ( -102.0629304562351791, -298.1732284488088567, -229.2192311247754617 ) ) ;
#395 = CARTESIAN_POINT ( 'NONE',  ( -25.13295117268265244, -286.8632252611534454, -198.2345166741048388 ) ) ;
#396 = CARTESIAN_POINT ( 'NONE',  ( -106.1398451837155505, -277.1705574142181945, -304.5341711825586231 ) ) ;
#397 = CARTESIAN_POINT ( 'NONE',  ( -65.55836371735222201, -296.0629673787829006, -341.9094569026487420 ) ) ;
#398 = CARTESIAN_POINT ( 'NONE',  ( -65.01824890676496693, -287.5493471980986442, -340.9453832113689487 ) ) ;
#399 = CARTESIAN_POINT ( 'NONE',  ( -112.8687659414040212, -297.0724226953441871, -255.4135726666953872 ) ) ;
#401 = CARTESIAN_POINT ( 'NONE',  ( -105.7319383130498238, -291.2284431431657481, -244.6273306386740671 ) ) ;
#400 = CIRCLE ( 'NONE', #83570, 2.500000000000007550 ) ;
#402 = CARTESIAN_POINT ( 'NONE',  ( 210.1640492649794396, 37.84931640281016030, 10.50000000000000000 ) ) ;
#403 = AXIS2_PLACEMENT_3D ( 'NONE', #74243, #31178, #30232 ) ;
#404 = DIRECTION ( 'NONE',  ( 0.000000000000000000, -1.000000000000000000, 0.000000000000000000 ) ) ;
#405 = CARTESIAN_POINT ( 'NONE',  ( -110.6395987777366372, -271.3322271728259238, -283.6871839692900039 ) ) ;
#406 = CARTESIAN_POINT ( 'NONE',  ( 36.69934693387597235, -288.8392658573746985, -251.9049237673648918 ) ) ;
#407 = CARTESIAN_POINT ( 'NONE',  ( -99.86837403722181250, -288.6952119285918457, -220.4570493818173702 ) ) ;
#408 = ORIENTED_EDGE ( 'NONE', *, *, #36940, .T. ) ;
#409 = AXIS2_PLACEMENT_3D ( 'NONE', #74640, #9280, #38163 ) ;
#410 = CARTESIAN_POINT ( 'NONE',  ( -110.4501830105272120, -278.2029926013627232, -246.3497191025504947 ) ) ;
#411 = CARTESIAN_POINT ( 'NONE',  ( -77.07960880002397630, -285.5857159168178896, -333.8331689869217485 ) ) ;
#412 = CARTESIAN_POINT ( 'NONE',  ( -111.3091925084824112, -282.8845413066624701, -289.5811479901594794 ) ) ;
#414 = CARTESIAN_POINT ( 'NONE',  ( 30.73219615365270485, -286.0310267411410905, -300.6096502203043315 ) ) ;
#413 = VECTOR ( 'NONE', #28280, 1000.000000000000000 ) ;
#415 = CARTESIAN_POINT ( 'NONE',  ( 9.776714872701816716, -278.2721951864857601, -329.7590680726313508 ) ) ;
#416 = CARTESIAN_POINT ( 'NONE',  ( -110.1599951406477516, -296.9581660565513062, -276.9113938487936366 ) ) ;
#417 = ORIENTED_EDGE ( 'NONE', *, *, #24378, .F. ) ;
#418 = CARTESIAN_POINT ( 'NONE',  ( -61.18891464443646555, -294.0530483757174238, -339.9316314393639686 ) ) ;
#419 = CARTESIAN_POINT ( 'NONE',  ( -71.19720023784525154, -280.2683243496197179, -201.3167996104560018 ) ) ;
#421 = CARTESIAN_POINT ( 'NONE',  ( -104.5325035349209770, -278.2870535611997980, -241.5637464807761603 ) ) ;
#420 = CARTESIAN_POINT ( 'NONE',  ( -95.61175034384609717, -279.1700810579507106, -226.3676360124166536 ) ) ;
#422 = CARTESIAN_POINT ( 'NONE',  ( -15.87710889929866376, -275.4030008116405384, -196.6801677939435820 ) ) ;
#423 = CARTESIAN_POINT ( 'NONE',  ( -82.37591756080814775, -276.5714600047618319, -332.4369729437565866 ) ) ;
#424 = CARTESIAN_POINT ( 'NONE',  ( -113.3918672577102740, -270.6791253856088133, -283.7747343605257129 ) ) ;
#425 = CARTESIAN_POINT ( 'NONE',  ( -67.97318274279425054, -296.8717553275860723, -340.3633934241867678 ) ) ;
#426 = CARTESIAN_POINT ( 'NONE',  ( -69.91165696735023971, -276.1233781216988064, -202.8022627189028810 ) ) ;
#427 = DIRECTION ( 'NONE',  ( -0.000000000000000000, 1.000000000000000000, -0.000000000000000000 ) ) ;
#428 = CARTESIAN_POINT ( 'NONE',  ( 7.103459944063120091, -287.7531359562102580, -211.9972993146364217 ) ) ;
#429 = CARTESIAN_POINT ( 'NONE',  ( -69.38620004629432003, -287.3964490037180326, -201.4475639410760834 ) ) ;
#430 = CARTESIAN_POINT ( 'NONE',  ( 35.06017669879758358, -287.0348881638780085, -280.5447993308172272 ) ) ;
#431 = CARTESIAN_POINT ( 'NONE',  ( 24.20210434625752782, -281.6748354658932953, -316.5334802164283019 ) ) ;
#432 = CARTESIAN_POINT ( 'NONE',  ( -110.7597969522451393, -277.0562332315128629, -262.3744125087495718 ) ) ;
#433 = CARTESIAN_POINT ( 'NONE',  ( -98.53737060242386292, -285.8362405327920328, -312.4739421121791452 ) ) ;
#434 = CARTESIAN_POINT ( 'NONE',  ( -98.55886781794781371, -277.5975963507496544, -229.2441326131148003 ) ) ;
#435 = CARTESIAN_POINT ( 'NONE',  ( -18.87697925039016056, -278.1245800897174263, -341.4968864787559824 ) ) ;
#436 = CARTESIAN_POINT ( 'NONE',  ( 7.363625341111400324, -275.1731506385693251, -212.5733829849779397 ) ) ;
#437 = CARTESIAN_POINT ( 'NONE',  ( -43.16748347093800930, -287.9191015667062175, -346.7421952665334857 ) ) ;
#438 =( BOUNDED_SURFACE ( )  B_SPLINE_SURFACE ( 3, 2, ( 
 ( #50320, #50797, #35669 ),
 ( #87224, #29020, #21923 ),
 ( #65495, #15274, #20984 ),
 ( #42745, #29497, #79681 ) ),
 .UNSPECIFIED., .F., .F., .F. ) 
 B_SPLINE_SURFACE_WITH_KNOTS ( ( 4, 4 ),
 ( 3, 3 ),
 ( 0.000000000000000000, 0.0009274969146595095750 ),
 ( 0.000000000000000000, 1.000000000000000000 ),
 .UNSPECIFIED. ) 
 GEOMETRIC_REPRESENTATION_ITEM ( )  RATIONAL_B_SPLINE_SURFACE ( (
 ( 1.000000000000000000, 0.7691239371209215303, 1.000000000000000000),
 ( 1.000000000000000000, 0.7869877059350417481, 1.000000000000000000),
 ( 1.000000000000000000, 0.8014280003973071054, 1.000000000000000000),
 ( 1.000000000000000000, 0.8108476219622873238, 1.000000000000000000) ) ) 
 REPRESENTATION_ITEM ( '' )  SURFACE ( )  );
#439 = CARTESIAN_POINT ( 'NONE',  ( -34.47473844410745158, -283.8198020982060257, -347.1461383420058269 ) ) ;
#440 = CIRCLE ( 'NONE', #73018, 5.024999999999987921 ) ;
#441 = CARTESIAN_POINT ( 'NONE',  ( 35.55280058431892343, -282.3566568378734019, -295.1421408184978645 ) ) ;
#442 = ORIENTED_EDGE ( 'NONE', *, *, #84617, .T. ) ;
#443 = VERTEX_POINT ( 'NONE', #78317 ) ;
#444 = CARTESIAN_POINT ( 'NONE',  ( 156.6537229343953754, 214.8829733828359849, 16.96953521546817001 ) ) ;
#445 = CARTESIAN_POINT ( 'NONE',  ( 11.63567796159732204, -290.2411052206740578, -328.1670165858570272 ) ) ;
#447 = ADVANCED_FACE ( 'NONE', ( #62233, #49878, #84920, #20557, #27656 ), #19601, .F. ) ;
#446 =( BOUNDED_SURFACE ( )  B_SPLINE_SURFACE ( 3, 2, ( 
 ( #46429, #52604, #66380 ),
 ( #81486, #45029, #45487 ),
 ( #9515, #38403, #9987 ),
 ( #68231, #32242, #60670 ) ),
 .UNSPECIFIED., .F., .F., .F. ) 
 B_SPLINE_SURFACE_WITH_KNOTS ( ( 4, 4 ),
 ( 3, 3 ),
 ( 0.000000000000000000, 0.0009274969146595095750 ),
 ( 0.000000000000000000, 1.000000000000000000 ),
 .UNSPECIFIED. ) 
 GEOMETRIC_REPRESENTATION_ITEM ( )  RATIONAL_B_SPLINE_SURFACE ( (
 ( 1.000000000000000000, 0.7691239371209221964, 1.000000000000000000),
 ( 1.000000000000000000, 0.7869877059350496307, 1.000000000000000000),
 ( 1.000000000000000000, 0.8014280003973005551, 1.000000000000000000),
 ( 1.000000000000000000, 0.8108476219622871017, 1.000000000000000000) ) ) 
 REPRESENTATION_ITEM ( '' )  SURFACE ( )  );
#448 = CARTESIAN_POINT ( 'NONE',  ( -101.2626605397846049, -289.7943000246049223, -228.2255153181214098 ) ) ;
#449 = CARTESIAN_POINT ( 'NONE',  ( 94.78702171985756308, -298.9449283184634965, -197.2183506070807653 ) ) ;
#450 = CARTESIAN_POINT ( 'NONE',  ( -11.09980241159285619, -294.0676480132073607, -342.6995274442535901 ) ) ;
#451 = CARTESIAN_POINT ( 'NONE',  ( 35.64438321566538548, -286.1663195541688651, -280.6380762210182525 ) ) ;
#452 = CARTESIAN_POINT ( 'NONE',  ( 36.05237603647821487, -288.7659386966579405, -271.0245089406109855 ) ) ;
#453 = CARTESIAN_POINT ( 'NONE',  ( 21.27581636871892101, -289.4090924074130839, -223.5744983911110353 ) ) ;
#454 = CARTESIAN_POINT ( 'NONE',  ( 37.35780284020656694, -289.6384337990135691, -277.0681965735167296 ) ) ;
#455 = CARTESIAN_POINT ( 'NONE',  ( -102.9959811661897078, -289.0380696731132275, -233.7613392213682744 ) ) ;
#456 = CARTESIAN_POINT ( 'NONE',  ( -41.38985635712994338, -294.0013616208397025, -195.4577283638537892 ) ) ;
#457 = CARTESIAN_POINT ( 'NONE',  ( -108.9475998404428339, -285.2906192478001230, -285.7830426642873931 ) ) ;
#458 = CARTESIAN_POINT ( 'NONE',  ( -44.74250737014229884, -293.9589824279485128, -195.5080083575545302 ) ) ;
#459 = CARTESIAN_POINT ( 'NONE',  ( 219.8344101925596021, 0.000000000000000000, 7.000000000000000000 ) ) ;
#460 = DIRECTION ( 'NONE',  ( -0.000000000000000000, -1.000000000000000000, -0.000000000000000000 ) ) ;
#461 = CARTESIAN_POINT ( 'NONE',  ( -69.45425524740572598, -275.6116147604159892, -202.1767048456104305 ) ) ;
#462 = CARTESIAN_POINT ( 'NONE',  ( 34.22529250880975127, -280.5486076104474478, -255.1103591393745091 ) ) ;
#463 = CARTESIAN_POINT ( 'NONE',  ( -5.198279291450013773, -280.6290538813578337, -338.1380734097782010 ) ) ;
#464 = CARTESIAN_POINT ( 'NONE',  ( -107.0242423197752260, -295.3340369974355895, -302.7417006471805507 ) ) ;
#465 = CARTESIAN_POINT ( 'NONE',  ( 26.15657362997979973, -273.2749777785776359, -232.2362400515366687 ) ) ;
#466 = CARTESIAN_POINT ( 'NONE',  ( -67.40623058219914299, -275.5294293008589648, -338.4598566561462576 ) ) ;
#467 = CARTESIAN_POINT ( 'NONE',  ( -70.70629809753577888, -298.9177607521856430, -204.8639294649306635 ) ) ;
#468 = AXIS2_PLACEMENT_3D ( 'NONE', #23626, #88479, #15587 ) ;
#469 = CARTESIAN_POINT ( 'NONE',  ( -12.79472286548296189, -296.1521451354898318, -339.7893085137351363 ) ) ;
#470 = EDGE_CURVE ( 'NONE', #443, #38673, #70143, .T. ) ;
#471 = CYLINDRICAL_SURFACE ( 'NONE', #38369, 1.000000000000000888 ) ;
#472 = CARTESIAN_POINT ( 'NONE',  ( -93.19907288353067543, -296.6847407908389300, -317.6304496190813325 ) ) ;
#473 = DIRECTION ( 'NONE',  ( -0.8510748438184358999, -0.5250018354872690862, -0.006684530980050039546 ) ) ;
#474 = AXIS2_PLACEMENT_3D ( 'NONE', #24792, #83000, #69744 ) ;
#476 = CARTESIAN_POINT ( 'NONE',  ( -108.7791315055169292, -296.7511089224530565, -255.2779189747055852 ) ) ;
#475 = CARTESIAN_POINT ( 'NONE',  ( -62.62531095629989153, -283.7448301468398881, -199.3741767513798777 ) ) ;
#477 = VECTOR ( 'NONE', #77768, 1000.000000000000000 ) ;
#478 = CARTESIAN_POINT ( 'NONE',  ( -104.0404571924912176, -285.0535134706426561, -231.7807334197285059 ) ) ;
#479 = CARTESIAN_POINT ( 'NONE',  ( 38.08672107127473794, -287.4111732831478889, -285.7330914080269508 ) ) ;
#480 = CARTESIAN_POINT ( 'NONE',  ( -27.84916182087626524, -290.1726618128096788, -196.0802578231074733 ) ) ;
#481 = AXIS2_PLACEMENT_3D ( 'NONE', #69178, #53570, #82445 ) ;
#482 = CARTESIAN_POINT ( 'NONE',  ( -96.68618260603486192, -278.4065655959097398, -221.5309156116981342 ) ) ;
#483 = CARTESIAN_POINT ( 'NONE',  ( -110.4683760289727132, -275.8380690714489560, -287.0191576251351080 ) ) ;
#484 = VECTOR ( 'NONE', #66979, 1000.000000000000000 ) ;
#485 = DIRECTION ( 'NONE',  ( 0.000000000000000000, 0.000000000000000000, -1.000000000000000000 ) ) ;
#486 = CARTESIAN_POINT ( 'NONE',  ( 15.32504751799938170, -285.6119886687430949, -219.2402396929666111 ) ) ;
#488 = DIRECTION ( 'NONE',  ( 0.000000000000000000, 1.000000000000000000, 0.000000000000000000 ) ) ;
#487 = CARTESIAN_POINT ( 'NONE',  ( -110.1331340237950371, -289.7794927530383688, -246.0517078306988310 ) ) ;
#489 = FACE_OUTER_BOUND ( 'NONE', #65073, .T. ) ;
#490 = CARTESIAN_POINT ( 'NONE',  ( -94.54989721759596932, -297.4992510617885841, -317.0035278207499232 ) ) ;
#491 = CARTESIAN_POINT ( 'NONE',  ( -2.673819891810099048, -281.9266918661726891, -202.2528603128815234 ) ) ;
#493 = CARTESIAN_POINT ( 'NONE',  ( 33.66971584016666696, -281.4439457894184216, -287.4280102006902666 ) ) ;
#492 = CARTESIAN_POINT ( 'NONE',  ( -112.0260394306532987, -294.4391519622371902, -280.7769840364173888 ) ) ;
#494 = CARTESIAN_POINT ( 'NONE',  ( 28.10704333086922801, -294.2504591929128992, -311.0255889924686130 ) ) ;
#495 = VECTOR ( 'NONE', #32367, 1000.000000000000000 ) ;
#496 = ADVANCED_FACE ( 'NONE', ( #85859 ), #33336, .T. ) ;
#497 = CARTESIAN_POINT ( 'NONE',  ( -67.88206223731559419, -281.6514772224624039, -201.8468337845070266 ) ) ;
#498 = CARTESIAN_POINT ( 'NONE',  ( -106.2125426076041634, -295.2784407768329515, -295.4144270085473636 ) ) ;
#499 = ORIENTED_EDGE ( 'NONE', *, *, #5733, .T. ) ;
#500 = CARTESIAN_POINT ( 'NONE',  ( 17.06571399127465583, -89.54582641780471874, -21.50000000000000000 ) ) ;
#501 = VECTOR ( 'NONE', #78144, 1000.000000000000000 ) ;
#502 = CARTESIAN_POINT ( 'NONE',  ( -95.55218877742616712, -285.8860174903883831, -317.1081560315652155 ) ) ;
#503 = CARTESIAN_POINT ( 'NONE',  ( -74.94434090351494149, -285.8906705383787994, 27.50000000000000000 ) ) ;
#504 = CARTESIAN_POINT ( 'NONE',  ( -110.4542110544635705, -282.2666405000204009, -253.6410175316879361 ) ) ;
#505 = CARTESIAN_POINT ( 'NONE',  ( -1.368022843707428438, -273.7141166933243994, -202.4637442224215818 ) ) ;
#506 = CARTESIAN_POINT ( 'NONE',  ( -109.9726748286922628, -290.4821773897211301, -263.0302572872621454 ) ) ;
#507 = CARTESIAN_POINT ( 'NONE',  ( 25.71966169681331849, -282.5511572894125152, -232.1312805657929346 ) ) ;
#508 = CARTESIAN_POINT ( 'NONE',  ( -96.93934988317018053, -274.7561529871699690, -226.7496344372156614 ) ) ;
#509 = AXIS2_PLACEMENT_3D ( 'NONE', #63054, #5739, #91883 ) ;
#510 = CARTESIAN_POINT ( 'NONE',  ( 33.84745103067382388, -283.4999324435455037, -297.5373055610141364 ) ) ;
#511 = CARTESIAN_POINT ( 'NONE',  ( 22.12468463488144010, -280.9459354239748450, -313.4044813569679491 ) ) ;
#512 = CARTESIAN_POINT ( 'NONE',  ( -111.1035872555647188, -280.7265676192138812, -256.7896531230614983 ) ) ;
#513 = CARTESIAN_POINT ( 'NONE',  ( -90.16440307809195076, -273.4969061714966756, -214.2636476280938780 ) ) ;
#514 = CARTESIAN_POINT ( 'NONE',  ( 2.419818390556676135, -274.4029431552878009, -204.4215877325289057 ) ) ;
#515 = CARTESIAN_POINT ( 'NONE',  ( 35.04236977698502642, -295.2468850698101619, -252.9326020219452857 ) ) ;
#516 = CARTESIAN_POINT ( 'NONE',  ( 159.4851178187871312, 15.00000000000000000, 9.000000000000000000 ) ) ;
#517 = CARTESIAN_POINT ( 'NONE',  ( 16.66419048074589782, -292.4339046538751177, -323.5739229754051394 ) ) ;
#518 = CARTESIAN_POINT ( 'NONE',  ( 5.217678648793666163, -274.1526882925118684, -210.9126626711573067 ) ) ;
#519 = CARTESIAN_POINT ( 'NONE',  ( -76.82721684469869672, -293.0540813855774900, -205.0039100937321734 ) ) ;
#521 = CARTESIAN_POINT ( 'NONE',  ( -33.57432131573970224, -293.3036558292391760, -193.8508861434929997 ) ) ;
#520 = CARTESIAN_POINT ( 'NONE',  ( -110.4683760289727132, -275.2662352645559167, -253.7030783399848985 ) ) ;
#522 = CARTESIAN_POINT ( 'NONE',  ( 32.19804620522597105, -289.9147606758254483, -298.1461082847454236 ) ) ;
#523 = CARTESIAN_POINT ( 'NONE',  ( -102.1838148814982645, -276.0511314017147129, -307.8220257815003720 ) ) ;
#524 = CARTESIAN_POINT ( 'NONE',  ( -73.52089337593383789, -279.4562368179799705, -335.4325269178318649 ) ) ;
#525 = CARTESIAN_POINT ( 'NONE',  ( -34.26569199195837712, -293.0930187872357351, -344.7375414908350422 ) ) ;
#526 = CARTESIAN_POINT ( 'NONE',  ( 18.23768133693696214, -282.6996858500997973, -218.8709457477553144 ) ) ;
#527 = EDGE_LOOP ( 'NONE', ( #23564, #43969, #29055, #47901 ) ) ;
#528 = CARTESIAN_POINT ( 'NONE',  ( -66.57193366333181928, -283.1125662302549699, -337.2901694264401158 ) ) ;
#529 = CARTESIAN_POINT ( 'NONE',  ( -79.75134091025527994, -280.5733721980102473, -206.3997167747376125 ) ) ;
#530 = CIRCLE ( 'NONE', #89712, 8.000000000000000000 ) ;
#531 = CARTESIAN_POINT ( 'NONE',  ( 35.22795202031545614, -280.6595075427375150, -295.0545065737637174 ) ) ;
#532 = CARTESIAN_POINT ( 'NONE',  ( -59.58534422498445338, -278.2746395945201812, -343.8324764135672922 ) ) ;
#533 =( NAMED_UNIT ( * ) SI_UNIT ( $, .STERADIAN. ) SOLID_ANGLE_UNIT ( ) );
#534 = CARTESIAN_POINT ( 'NONE',  ( -6.833954875992621858, -278.1790821057300604, -340.3179759246217486 ) ) ;
#535 = CARTESIAN_POINT ( 'NONE',  ( -102.0455923789670294, -281.4805209788416960, -239.2376011013261916 ) ) ;
#536 = EDGE_LOOP ( 'NONE', ( #40735, #1250, #34787, #36151 ) ) ;
#537 = ORIENTED_EDGE ( 'NONE', *, *, #58978, .T. ) ;
#538 = CARTESIAN_POINT ( 'NONE',  ( -94.27891396533529189, -299.2288517735989899, -221.5237939030694179 ) ) ;
#539 = VECTOR ( 'NONE', #13268, 1000.000000000000000 ) ;
#540 = CARTESIAN_POINT ( 'NONE',  ( -51.61964741925273614, -275.2557921787226292, -343.6276657439970563 ) ) ;
#541 = CARTESIAN_POINT ( 'NONE',  ( -39.20955032075062263, -293.7891813239779140, -194.3845451917290461 ) ) ;
#542 = CARTESIAN_POINT ( 'NONE',  ( 29.58004740640543417, -293.2959480609137017, -299.7783302023191254 ) ) ;
#543 = CARTESIAN_POINT ( 'NONE',  ( 32.65864715560118725, -286.6498733850967255, -238.3035732600245922 ) ) ;
#544 = CARTESIAN_POINT ( 'NONE',  ( 186.6539576904058890, 276.0000000000000568, 11.60392986742922616 ) ) ;
#546 = CARTESIAN_POINT ( 'NONE',  ( -108.5382654350417795, -282.6975571727014653, -289.8379683928316126 ) ) ;
#545 = CARTESIAN_POINT ( 'NONE',  ( -22.23194966639039194, -293.4369986843219635, -345.2630654359047639 ) ) ;
#547 = CARTESIAN_POINT ( 'NONE',  ( -64.24683902220084519, -291.2672496188426408, -339.6042094105640672 ) ) ;
#548 = CARTESIAN_POINT ( 'NONE',  ( -108.0627017584748870, -282.7599712521561628, -291.1245075829212965 ) ) ;
#549 = CARTESIAN_POINT ( 'NONE',  ( 25.99246253114274552, -283.3771681065013013, -307.7447886190831241 ) ) ;
#550 = CARTESIAN_POINT ( 'NONE',  ( -45.98732877144905018, -290.1003550732238523, -346.6903779564393062 ) ) ;
#551 = CIRCLE ( 'NONE', #48930, 4.025000000000000355 ) ;
#552 = CARTESIAN_POINT ( 'NONE',  ( -27.55633526468844252, -280.6720254424021164, -197.9066035369142469 ) ) ;
#553 = CARTESIAN_POINT ( 'NONE',  ( -33.47033252515218749, -293.7993959282042056, -346.8792103833187639 ) ) ;
#554 = CARTESIAN_POINT ( 'NONE',  ( -37.49099266878829440, -289.8567683557566852, -347.2125418609350049 ) ) ;
#555 = CARTESIAN_POINT ( 'NONE',  ( 12.38083513092553289, -288.8732566723153354, -329.0739478451774289 ) ) ;
#556 = CARTESIAN_POINT ( 'NONE',  ( -8.256898078943684993, -286.6106324874740494, -203.4053542703483117 ) ) ;
#557 = VERTEX_POINT ( 'NONE', #91558 ) ;
#558 = CARTESIAN_POINT ( 'NONE',  ( 195.4431342809958210, 25.62282010151562162, 12.94565045871722653 ) ) ;
#559 = CARTESIAN_POINT ( 'NONE',  ( 12.59971999844131396, -296.2254926977316813, -327.4057811323250462 ) ) ;
#560 = CIRCLE ( 'NONE', #36843, 1.897123461337413275 ) ;
#561 = CARTESIAN_POINT ( 'NONE',  ( -113.6276753064661165, -295.3183646335438652, -263.8953553310242910 ) ) ;
#562 = CARTESIAN_POINT ( 'NONE',  ( -109.7264424368263178, -277.4645562237244008, -281.4902477421676394 ) ) ;
#563 = CARTESIAN_POINT ( 'NONE',  ( 98.96984324953363910, -299.0653406705604880, -193.4775484312997662 ) ) ;
#564 = CARTESIAN_POINT ( 'NONE',  ( -12.79537854053787704, -293.2072255931282143, -339.9000241336492536 ) ) ;
#565 = CARTESIAN_POINT ( 'NONE',  ( 33.01822646521787874, -277.0097735718116496, -247.2300213676486464 ) ) ;
#566 = CARTESIAN_POINT ( 'NONE',  ( -35.08692667047458258, -296.3206129209522146, -196.3484649373850175 ) ) ;
#567 = CARTESIAN_POINT ( 'NONE',  ( 36.10541241948924807, -294.7622949125877767, -270.7467767446918856 ) ) ;
#568 = CARTESIAN_POINT ( 'NONE',  ( 26.06689073608121276, -295.1344300300592636, -307.1521043461206659 ) ) ;
#569 = DIRECTION ( 'NONE',  ( -0.7957555401921984073, -0.6056179655966479336, 0.000000000000000000 ) ) ;
#570 = CIRCLE ( 'NONE', #62551, 4.025000000000000355 ) ;
#571 = CARTESIAN_POINT ( 'NONE',  ( -97.60692826702394598, -295.1643581662601719, -225.4160354886601851 ) ) ;
#572 = CARTESIAN_POINT ( 'NONE',  ( -9.165054654810878887, -299.0476583445857841, -193.4600241329953008 ) ) ;
#573 = DIRECTION ( 'NONE',  ( -1.000000000000000000, 0.000000000000000000, 0.000000000000000000 ) ) ;
#574 = CARTESIAN_POINT ( 'NONE',  ( -68.84837883859820806, -290.4181530666822368, -336.4726725368212783 ) ) ;
#575 = CARTESIAN_POINT ( 'NONE',  ( -28.88931899185833885, -295.2754706862511966, -342.9424488748248905 ) ) ;
#576 = CARTESIAN_POINT ( 'NONE',  ( -93.95798993011017330, -279.8443368349776392, -320.0904104946291682 ) ) ;
#577 = CARTESIAN_POINT ( 'NONE',  ( -113.2789115823150041, -277.1143977978192652, -280.1000033892999568 ) ) ;
#578 = AXIS2_PLACEMENT_3D ( 'NONE', #28803, #50094, #12739 ) ;
#579 = CARTESIAN_POINT ( 'NONE',  ( 19.70231359237515179, -281.6026258314327038, -322.0073482961647642 ) ) ;
#580 = CARTESIAN_POINT ( 'NONE',  ( 36.49033549754070549, -274.6286845839015314, -248.6774485503754875 ) ) ;
#581 = CARTESIAN_POINT ( 'NONE',  ( -56.71680268613243925, -281.3837387631637625, -342.2354499514945587 ) ) ;
#582 = CARTESIAN_POINT ( 'NONE',  ( -45.17069689039524860, -278.3545798726502767, -194.5119291036368736 ) ) ;
#583 = CARTESIAN_POINT ( 'NONE',  ( -22.89302449604697998, -278.2363000005352660, -196.5432261782136436 ) ) ;
#584 = EDGE_CURVE ( 'NONE', #89341, #28861, #72351, .T. ) ;
#585 = CARTESIAN_POINT ( 'NONE',  ( -71.88205993780856318, -296.2703597272860065, -205.4761310522087570 ) ) ;
#586 = CARTESIAN_POINT ( 'NONE',  ( 37.31721839381581418, -277.6507211666369130, -278.0251792108447830 ) ) ;
#587 = LINE ( 'NONE', #21899, #2031 ) ;
#588 = CARTESIAN_POINT ( 'NONE',  ( -22.49268826115504893, -290.2613106025819434, -196.4302554823797493 ) ) ;
#589 = CARTESIAN_POINT ( 'NONE',  ( -107.7313703303886285, -290.1523481562727511, -301.7059457455363258 ) ) ;
#590 = VECTOR ( 'NONE', #42774, 1000.000000000000000 ) ;
#591 = CARTESIAN_POINT ( 'NONE',  ( -60.33512634693056498, -275.7550055312672157, -198.7433316086200819 ) ) ;
#592 = CARTESIAN_POINT ( 'NONE',  ( -94.41974712616571708, -271.2258015954081429, -221.6884789025067164 ) ) ;
#593 = CARTESIAN_POINT ( 'NONE',  ( -110.7686810774425936, -284.0362970395182174, -247.5406166420813747 ) ) ;
#594 = DIRECTION ( 'NONE',  ( -0.000000000000000000, 0.000000000000000000, -1.000000000000000000 ) ) ;
#595 = CARTESIAN_POINT ( 'NONE',  ( -42.85221553818946205, -283.9824678662702127, -195.5510574499011227 ) ) ;
#596 = DIRECTION ( 'NONE',  ( 0.000000000000000000, 0.000000000000000000, 1.000000000000000000 ) ) ;
#597 = CARTESIAN_POINT ( 'NONE',  ( -34.82839873673886899, -290.8793472931504311, -197.0070872693103183 ) ) ;
#598 = CARTESIAN_POINT ( 'NONE',  ( -109.2187920824703014, -282.9326966191597421, -251.7990832069660883 ) ) ;
#599 = CARTESIAN_POINT ( 'NONE',  ( 195.7618616733231249, 25.17790309710478880, 14.26375052247069597 ) ) ;
#600 = DIRECTION ( 'NONE',  ( 0.000000000000000000, 0.000000000000000000, -1.000000000000000000 ) ) ;
#601 = CARTESIAN_POINT ( 'NONE',  ( 37.19157926738635211, -291.6650951418104114, -279.1700606143812706 ) ) ;
#602 = CARTESIAN_POINT ( 'NONE',  ( -55.55561266974274304, -281.7623218828950939, -344.4621378191625354 ) ) ;
#603 = CARTESIAN_POINT ( 'NONE',  ( -108.5873101429798737, -279.9007832254608843, -289.6095846808224223 ) ) ;
#604 = CARTESIAN_POINT ( 'NONE',  ( -100.6768922541744047, -286.3294367639458073, -227.1783866267950032 ) ) ;
#605 = CARTESIAN_POINT ( 'NONE',  ( -69.98243004323033745, -285.6098162693991753, -205.0510579513368725 ) ) ;
#606 = CARTESIAN_POINT ( 'NONE',  ( -26.92027407178215270, -278.3423156410380557, -343.2086903171750123 ) ) ;
#607 = CARTESIAN_POINT ( 'NONE',  ( -110.3286395538065392, -279.2794286552243079, -276.1017110174043978 ) ) ;
#608 = EDGE_CURVE ( 'NONE', #87677, #6373, #68742, .T. ) ;
#609 = CARTESIAN_POINT ( 'NONE',  ( -72.69342520872417879, -287.5845644191949191, -204.1578700096011403 ) ) ;
#610 = VERTEX_POINT ( 'NONE', #13456 ) ;
#611 = VECTOR ( 'NONE', #22104, 1000.000000000000000 ) ;
#612 = CARTESIAN_POINT ( 'NONE',  ( -36.27657800195181892, -294.8725021804859239, -347.3668546410453359 ) ) ;
#613 = CARTESIAN_POINT ( 'NONE',  ( 35.62372540500069107, -289.7358906677945356, -286.1657956460347805 ) ) ;
#614 = DIRECTION ( 'NONE',  ( 0.000000000000000000, 0.000000000000000000, 1.000000000000000000 ) ) ;
#615 = CARTESIAN_POINT ( 'NONE',  ( 25.18497378105907814, -277.4090924074130839, -220.4570493818173702 ) ) ;
#616 = CARTESIAN_POINT ( 'NONE',  ( 36.65006893773713159, -291.7218174702185820, -252.1496235759580600 ) ) ;
#617 = AXIS2_PLACEMENT_3D ( 'NONE', #50183, #27969, #71997 ) ;
#618 = CARTESIAN_POINT ( 'NONE',  ( -16.99888552950729448, -287.8396185546561128, -199.4778519094652438 ) ) ;
#619 = CARTESIAN_POINT ( 'NONE',  ( -108.5999294765276062, -280.5736674880837995, -250.3081247049989599 ) ) ;
#620 = CARTESIAN_POINT ( 'NONE',  ( 5.244095234645274495, -289.9134760916920186, -333.8044495868525701 ) ) ;
#621 = CARTESIAN_POINT ( 'NONE',  ( -66.05854980302595436, -285.4280788811326488, -339.6595958286496852 ) ) ;
#622 = CARTESIAN_POINT ( 'NONE',  ( -102.0958390393031152, -278.1710745719942111, -312.1225588290878363 ) ) ;
#623 = ORIENTED_EDGE ( 'NONE', *, *, #12372, .T. ) ;
#624 = CARTESIAN_POINT ( 'NONE',  ( 38.16695403606040315, -291.6674930577466398, -273.1463184486848377 ) ) ;
#625 = CARTESIAN_POINT ( 'NONE',  ( 38.14512944601662525, -281.5754459229366375, -285.5511991337033351 ) ) ;
#626 = AXIS2_PLACEMENT_3D ( 'NONE', #69064, #4653, #32616 ) ;
#627 = CARTESIAN_POINT ( 'NONE',  ( -91.10728457839564953, -275.1385753027915371, -219.1553335681576300 ) ) ;
#628 = VECTOR ( 'NONE', #56195, 1000.000000000000000 ) ;
#629 = CARTESIAN_POINT ( 'NONE',  ( 196.6877655503061817, 294.2166337988281839, -7.999911143031724237 ) ) ;
#630 = CARTESIAN_POINT ( 'NONE',  ( -4.771743288812468897, -297.1233781216987495, -337.9199732462171255 ) ) ;
#631 = CARTESIAN_POINT ( 'NONE',  ( -1.755944882127600470, -272.7569627845279001, -203.2222466845226450 ) ) ;
#632 = DIRECTION ( 'NONE',  ( 0.000000000000000000, 0.000000000000000000, -1.000000000000000000 ) ) ;
#633 = CARTESIAN_POINT ( 'NONE',  ( -93.13313667296279164, -278.7298411586599514, -223.1687471948053485 ) ) ;
#634 = AXIS2_PLACEMENT_3D ( 'NONE', #54460, #69150, #62530 ) ;
#635 = CARTESIAN_POINT ( 'NONE',  ( 22.34134370700455108, -277.4043121424948595, -318.4021071408388366 ) ) ;
#636 = CARTESIAN_POINT ( 'NONE',  ( -47.37087138965788569, -299.3476306537725691, -197.4068819803149779 ) ) ;
#637 = CARTESIAN_POINT ( 'NONE',  ( -30.24860219207629086, -282.0232362878585946, -346.7974194006311563 ) ) ;
#638 = CARTESIAN_POINT ( 'NONE',  ( -82.36296692948907605, -293.1885541418192247, -211.5505299430354853 ) ) ;
#639 = CARTESIAN_POINT ( 'NONE',  ( 97.63982572653510772, -301.2333003928553694, -194.0202035235065523 ) ) ;
#640 = CARTESIAN_POINT ( 'NONE',  ( -29.12807470841969959, -299.3579053438171513, -193.7565484485259617 ) ) ;
#641 = CARTESIAN_POINT ( 'NONE',  ( 13.62160783359252392, -296.3369496282019782, -325.2296967268541721 ) ) ;
#642 = CARTESIAN_POINT ( 'NONE',  ( -77.12276404418378206, -281.5860396746064112, -333.8061287737435805 ) ) ;
#643 = CARTESIAN_POINT ( 'NONE',  ( -49.11044639364758524, -271.9217030055709188, -196.5975770573392083 ) ) ;
#644 = CARTESIAN_POINT ( 'NONE',  ( 4.720918495268251469, -288.2095907686901910, -206.7595012800831853 ) ) ;
#645 = TOROIDAL_SURFACE ( 'NONE', #5171, 1.000000000000000000, 0.5000000000000000000 ) ;
#646 = CARTESIAN_POINT ( 'NONE',  ( -0.8494590164562774159, -287.4760563537427061, -334.0005347574279995 ) ) ;
#647 = CARTESIAN_POINT ( 'NONE',  ( 204.7385211771276090, 294.9049021488058315, -68.64726399651360111 ) ) ;
#648 = ORIENTED_EDGE ( 'NONE', *, *, #78193, .T. ) ;
#649 = CARTESIAN_POINT ( 'NONE',  ( -82.51898930543246991, -288.2306517282796108, -331.9859411788225430 ) ) ;
#650 = CARTESIAN_POINT ( 'NONE',  ( -10.72034586036382287, -288.3620045295733689, -338.4108699226561043 ) ) ;
#651 = ORIENTED_EDGE ( 'NONE', *, *, #66834, .T. ) ;
#652 = CARTESIAN_POINT ( 'NONE',  ( -60.43001306444523379, -286.8393884576937580, -197.1728528206301689 ) ) ;
#653 = CARTESIAN_POINT ( 'NONE',  ( -36.46166220244045064, -277.3741405195800098, -343.3894296830907820 ) ) ;
#654 = CARTESIAN_POINT ( 'NONE',  ( 31.91276623249945388, -292.0471199576754771, -237.2935922219214149 ) ) ;
#655 = CARTESIAN_POINT ( 'NONE',  ( -114.1060177499678190, -285.1364680378219418, -275.7189543159105369 ) ) ;
#656 = CARTESIAN_POINT ( 'NONE',  ( 27.25401748960190673, -282.5344009542761228, -229.6406980113972054 ) ) ;
#657 = CARTESIAN_POINT ( 'NONE',  ( -30.21262458242523508, -283.2975638927446767, -347.0091484423581392 ) ) ;
#658 = CARTESIAN_POINT ( 'NONE',  ( 23.69787251492912006, -281.3288461764117869, -230.1917899458019576 ) ) ;
#659 = CARTESIAN_POINT ( 'NONE',  ( 45.39964763510799628, 12.39790288765882842, -332.1295406407559199 ) ) ;
#660 = CARTESIAN_POINT ( 'NONE',  ( -111.9891808443444461, -280.6201449729597357, -265.0902502256173534 ) ) ;
#661 = CARTESIAN_POINT ( 'NONE',  ( 184.0236931359747246, 263.5994396450613522, -152.8319179813719870 ) ) ;
#662 = CARTESIAN_POINT ( 'NONE',  ( 166.1890715538564791, 230.9239408293323095, -190.2239395719806510 ) ) ;
#663 = CARTESIAN_POINT ( 'NONE',  ( -78.93849876691669465, -272.6728204782807552, -210.1139715849992058 ) ) ;
#664 = CARTESIAN_POINT ( 'NONE',  ( 0.5047639842331865800, -294.0694645151006625, -337.3626420394939487 ) ) ;
#665 = CARTESIAN_POINT ( 'NONE',  ( -97.29061877149726456, -247.0397287528579113, -331.5487825117278362 ) ) ;
#666 = CARTESIAN_POINT ( 'NONE',  ( -13.20211036784315972, -273.0441534182189685, -197.7623681437754328 ) ) ;
#667 = CARTESIAN_POINT ( 'NONE',  ( -40.59542752110353803, -299.8712516084596587, -196.1844929354027443 ) ) ;
#668 = CARTESIAN_POINT ( 'NONE',  ( 35.01011000808389184, -289.0363855024123154, -283.2630189616197640 ) ) ;
#669 = ORIENTED_EDGE ( 'NONE', *, *, #93158, .F. ) ;
#670 = CARTESIAN_POINT ( 'NONE',  ( -47.58826728983434862, -296.1206370813446824, -346.4388944609972896 ) ) ;
#671 = CARTESIAN_POINT ( 'NONE',  ( 2.475306229651003775, -287.0942543838424399, -209.1026945105221841 ) ) ;
#672 = CARTESIAN_POINT ( 'NONE',  ( -91.93931476158491023, -272.2152748747753321, -216.5039644581051164 ) ) ;
#673 = CARTESIAN_POINT ( 'NONE',  ( 39.07760704016652653, -294.4615816861127655, -278.8668147344420731 ) ) ;
#674 = CARTESIAN_POINT ( 'NONE',  ( 30.85070177834801441, -294.5045078308516509, -305.9886807015176942 ) ) ;
#675 = CARTESIAN_POINT ( 'NONE',  ( -92.55788908050703867, -291.3992417568560427, -222.6099663514978602 ) ) ;
#676 = ORIENTED_EDGE ( 'NONE', *, *, #7722, .F. ) ;
#677 = CARTESIAN_POINT ( 'NONE',  ( -10.87534909323254162, -276.3145722300414491, -199.5322585787767764 ) ) ;
#678 = CARTESIAN_POINT ( 'NONE',  ( 30.18575029894034856, -274.8182300232326156, -306.6400819815780210 ) ) ;
#679 = EDGE_CURVE ( 'NONE', #83322, #83798, #47998, .T. ) ;
#680 = ORIENTED_EDGE ( 'NONE', *, *, #88813, .T. ) ;
#681 = CARTESIAN_POINT ( 'NONE',  ( -98.75809043947947430, -277.4419339083197542, -316.7244509340659420 ) ) ;
#682 = CARTESIAN_POINT ( 'NONE',  ( 34.01050524860151825, -274.1982273214497923, -289.2106061636620780 ) ) ;
#683 = CARTESIAN_POINT ( 'NONE',  ( -83.39540030172024387, -274.4831417728582323, -213.3235621710938972 ) ) ;
#684 = AXIS2_PLACEMENT_3D ( 'NONE', #53670, #32361, #85228 ) ;
#685 = CARTESIAN_POINT ( 'NONE',  ( 15.60864973082017393, -275.7652360154463622, -219.6945515725571170 ) ) ;
#686 = CARTESIAN_POINT ( 'NONE',  ( -69.72061775601729039, -275.3918994113864755, -201.6040406954463435 ) ) ;
#687 = CARTESIAN_POINT ( 'NONE',  ( 37.98731941993962380, -273.5468729298579547, -268.3747610727709798 ) ) ;
#688 = CARTESIAN_POINT ( 'NONE',  ( -73.34539347806307319, -296.1946930322869207, -333.9820794140245539 ) ) ;
#689 = CARTESIAN_POINT ( 'NONE',  ( 32.90389529345434738, -292.4151633868495423, -292.2912625614695230 ) ) ;
#690 = DIRECTION ( 'NONE',  ( 1.000000000000000000, 0.000000000000000000, -0.000000000000000000 ) ) ;
#691 = CARTESIAN_POINT ( 'NONE',  ( -73.74206659050952339, -280.0745212260765697, -202.5631407710726535 ) ) ;
#692 = CARTESIAN_POINT ( 'NONE',  ( 0.6106540497750301277, -274.7402250509520627, -208.0023269674989308 ) ) ;
#693 = CIRCLE ( 'NONE', #79306, 1.999999999999988454 ) ;
#694 = CARTESIAN_POINT ( 'NONE',  ( -113.6585905315610887, -283.3136399340182834, -264.2707121798462140 ) ) ;
#695 = CARTESIAN_POINT ( 'NONE',  ( -92.33048596441228995, -297.8364558181106077, -321.6271343944029013 ) ) ;
#696 = CARTESIAN_POINT ( 'NONE',  ( 193.9646936176702070, 20.00000000000000000, -15.00000000000000000 ) ) ;
#697 = CARTESIAN_POINT ( 'NONE',  ( -44.02897957833364018, -285.1626039587596892, -197.5059052623096534 ) ) ;
#698 = AXIS2_PLACEMENT_3D ( 'NONE', #32787, #46964, #39859 ) ;
#699 = CARTESIAN_POINT ( 'NONE',  ( -97.21239272151814248, -277.3926882713108171, -226.8470491839136400 ) ) ;
#700 = CARTESIAN_POINT ( 'NONE',  ( -29.66990048082298514, -275.5279792476659395, -343.6006735400557659 ) ) ;
#701 = CARTESIAN_POINT ( 'NONE',  ( -82.90715564395567583, -285.6751684639340283, -329.9973929718272529 ) ) ;
#702 = CARTESIAN_POINT ( 'NONE',  ( 31.48537372293037961, -276.4191044763052787, -244.8667184141149846 ) ) ;
#703 = CARTESIAN_POINT ( 'NONE',  ( 154.5739546116847407, 19.95362051968588801, 14.09237539257051530 ) ) ;
#704 = CARTESIAN_POINT ( 'NONE',  ( 34.44041461593528908, -274.2798963078302563, -296.0854221206491843 ) ) ;
#705 = CARTESIAN_POINT ( 'NONE',  ( -45.10985561628647389, -281.9542883495410024, -195.5451983406714476 ) ) ;
#706 = CARTESIAN_POINT ( 'NONE',  ( 151.2975037349263800, 130.0000000000000568, 12.50000000000000000 ) ) ;
#707 = CARTESIAN_POINT ( 'NONE',  ( 23.00713597926944942, -290.0892507473819819, -315.8290427371612736 ) ) ;
#708 = CARTESIAN_POINT ( 'NONE',  ( 36.16907749350749413, -291.7437606598707589, -285.2963673797056003 ) ) ;
#709 = CIRCLE ( 'NONE', #58172, 7.500000000000012434 ) ;
#710 = CARTESIAN_POINT ( 'NONE',  ( -93.27831109108397811, -271.9106773320791035, -222.6726400747448054 ) ) ;
#711 = CARTESIAN_POINT ( 'NONE',  ( -94.37384017523662294, -289.3549625681253588, -222.8207545989157836 ) ) ;
#712 = CARTESIAN_POINT ( 'NONE',  ( 202.1133578493929974, 280.9843981858382449, -111.1516734208197050 ) ) ;
#713 = CARTESIAN_POINT ( 'NONE',  ( -71.35234327475265559, -295.6029625508436425, -203.5016567919726356 ) ) ;
#714 = CARTESIAN_POINT ( 'NONE',  ( -93.09953196885054183, -288.3145404164422985, -322.5311680223112489 ) ) ;
#715 = CARTESIAN_POINT ( 'NONE',  ( -13.24915408362107350, -284.3342105798197395, -340.1719614645312504 ) ) ;
#716 = CARTESIAN_POINT ( 'NONE',  ( -112.1435345831089876, -282.6189540547150045, -284.0168456740346414 ) ) ;
#717 = CARTESIAN_POINT ( 'NONE',  ( -68.01354514851423971, -284.8882368152389404, -337.2536649652591336 ) ) ;
#718 = CARTESIAN_POINT ( 'NONE',  ( -108.1875804585888972, -285.5955144221215960, -252.1001495632447700 ) ) ;
#719 = CARTESIAN_POINT ( 'NONE',  ( -41.64096488500164384, -291.0859193018515612, -345.6065183928104716 ) ) ;
#720 = CARTESIAN_POINT ( 'NONE',  ( -29.84516578740547033, -274.4778797707422200, -193.7481539074419175 ) ) ;
#721 = CARTESIAN_POINT ( 'NONE',  ( -40.30719237505373087, -287.1689770165053233, -345.8757432178310296 ) ) ;
#722 = CARTESIAN_POINT ( 'NONE',  ( 20.82025024435684912, -276.2342150227256639, -320.8408352078911321 ) ) ;
#723 = CARTESIAN_POINT ( 'NONE',  ( 37.06597823717751083, -295.6087467872084176, -276.3062168818707391 ) ) ;
#724 = CARTESIAN_POINT ( 'NONE',  ( -48.18343439339130896, -254.0284636146130595, -457.8806065563920242 ) ) ;
#725 = CARTESIAN_POINT ( 'NONE',  ( -114.2704648735229114, -293.0519495502703080, -270.3937649182068981 ) ) ;
#726 = CARTESIAN_POINT ( 'NONE',  ( -42.98740052095085673, -281.8095809704739168, -343.6875247501199055 ) ) ;
#727 = CARTESIAN_POINT ( 'NONE',  ( -98.97715580903263799, -275.9694145354928878, -313.3855183923923278 ) ) ;
#728 = CARTESIAN_POINT ( 'NONE',  ( -100.6226321081433781, -271.6000071654493695, -227.6263586771150074 ) ) ;
#729 = CARTESIAN_POINT ( 'NONE',  ( -1.427376833368756426, -275.9114168707258159, -334.0898501826283677 ) ) ;
#730 = CARTESIAN_POINT ( 'NONE',  ( -4.541713650276184566, -294.0124598401033609, -204.3556340102542777 ) ) ;
#731 = CARTESIAN_POINT ( 'NONE',  ( 34.17699636152847376, -294.2853670901897658, -254.5397820205500068 ) ) ;
#733 = ADVANCED_FACE ( 'NONE', ( #49428 ), #55131, .T. ) ;
#732 = CARTESIAN_POINT ( 'NONE',  ( -98.96298881946114534, -286.8735947792195589, -229.3636693604602783 ) ) ;
#734 = CARTESIAN_POINT ( 'NONE',  ( 20.84983128615508363, -294.3043723182107101, -220.8199075194258683 ) ) ;
#735 = CARTESIAN_POINT ( 'NONE',  ( 36.93909827691977199, -294.6366481941321922, -252.0400573451966295 ) ) ;
#736 = CARTESIAN_POINT ( 'NONE',  ( -104.9627000912016257, -296.0170608139034698, -297.8638518189455340 ) ) ;
#737 = CARTESIAN_POINT ( 'NONE',  ( -85.96274351581530482, -291.7255569088807192, -327.5347675078998577 ) ) ;
#738 = CARTESIAN_POINT ( 'NONE',  ( -16.13979987481713607, -282.9521913927768537, -344.4399102074102643 ) ) ;
#739 = CARTESIAN_POINT ( 'NONE',  ( -95.07089606665093129, -271.3642186167389809, -221.2733869658146659 ) ) ;
#740 = CARTESIAN_POINT ( 'NONE',  ( 14.24845483363844245, -286.5864904423447683, -213.1279171234522209 ) ) ;
#741 = CARTESIAN_POINT ( 'NONE',  ( -90.23390132372703931, -279.7841386887515114, -323.1057526331036911 ) ) ;
#742 = EDGE_CURVE ( 'NONE', #34447, #93704, #90736, .T. ) ;
#743 = CARTESIAN_POINT ( 'NONE',  ( -110.0031653911141376, -283.4830689082544950, -259.9956961012273950 ) ) ;
#744 = CARTESIAN_POINT ( 'NONE',  ( 13.23568978385866401, -286.3453118881884052, -325.8113266033782907 ) ) ;
#745 = CARTESIAN_POINT ( 'NONE',  ( -40.92587324162294493, -278.1471230759572677, -194.6681552588967747 ) ) ;
#746 = CARTESIAN_POINT ( 'NONE',  ( -111.6667267435858832, -264.5695759149226092, -294.5014218916285245 ) ) ;
#747 = CARTESIAN_POINT ( 'NONE',  ( -72.39803528208439332, -285.0825930300327400, -206.2450818814191393 ) ) ;
#748 = CARTESIAN_POINT ( 'NONE',  ( 27.50698835981510015, -282.2194054974996789, -229.4860579828455514 ) ) ;
#749 = CARTESIAN_POINT ( 'NONE',  ( -34.68699798678275670, -288.0783086793965708, -347.0799081848566061 ) ) ;
#750 = CARTESIAN_POINT ( 'NONE',  ( -34.30239203478355847, -278.6146582274110983, -346.5004837745580062 ) ) ;
#751 = CARTESIAN_POINT ( 'NONE',  ( -1.682637469674603148, -277.9047561968292257, -338.0495920695061614 ) ) ;
#752 = CARTESIAN_POINT ( 'NONE',  ( -59.73161367698386925, -279.5873447164300387, -200.8262205653199999 ) ) ;
#753 = CARTESIAN_POINT ( 'NONE',  ( -29.84929053798609999, -276.1273659102687930, -196.0932877960297844 ) ) ;
#754 = CARTESIAN_POINT ( 'NONE',  ( 30.90234519700421600, -294.0122398859246005, -306.0227258777134125 ) ) ;
#755 = CARTESIAN_POINT ( 'NONE',  ( 6.797377311284128254, -286.4689073349238129, -330.6217694938074487 ) ) ;
#756 = CARTESIAN_POINT ( 'NONE',  ( -102.5419994578473109, -292.6735454659420270, -230.8212709184644780 ) ) ;
#757 = CARTESIAN_POINT ( 'NONE',  ( 23.18044467625053073, -293.0467460412842229, -311.8176801205185598 ) ) ;
#758 = CARTESIAN_POINT ( 'NONE',  ( -23.51899185931068814, -294.5374246873147968, -342.1136448299192807 ) ) ;
#759 = CARTESIAN_POINT ( 'NONE',  ( -88.45374369700220996, -292.4348123581069672, -213.1854980804716035 ) ) ;
#760 = AXIS2_PLACEMENT_3D ( 'NONE', #30344, #9477, #21860 ) ;
#761 = CARTESIAN_POINT ( 'NONE',  ( 25.21923189938433651, -281.6825884757689664, -232.4474024143111990 ) ) ;
#762 = CARTESIAN_POINT ( 'NONE',  ( -37.59279624607444958, -296.9694114674621801, -193.6706396809427133 ) ) ;
#763 = CARTESIAN_POINT ( 'NONE',  ( -31.82579664469638914, -289.6358137486776627, -347.1135885367444303 ) ) ;
#764 = CARTESIAN_POINT ( 'NONE',  ( -38.73399144683423145, -281.2090305365150584, -346.1131279147828081 ) ) ;
#765 = CARTESIAN_POINT ( 'NONE',  ( 21.47561144938456579, -288.5546550054625072, -320.0226539073504455 ) ) ;
#766 = CARTESIAN_POINT ( 'NONE',  ( -69.99569326733218588, -285.9430435095978851, -205.0340450781253878 ) ) ;
#767 = CARTESIAN_POINT ( 'NONE',  ( 153.3814170968207407, 207.2574094408751080, -217.2232996818673882 ) ) ;
#768 = CARTESIAN_POINT ( 'NONE',  ( -112.6840901989520205, -268.7463710152937892, -295.7251649536935361 ) ) ;
#769 = CARTESIAN_POINT ( 'NONE',  ( 192.8699606740408683, 275.8991237878555012, -123.9883993914645401 ) ) ;
#770 =( GEOMETRIC_REPRESENTATION_CONTEXT ( 3 ) GLOBAL_UNCERTAINTY_ASSIGNED_CONTEXT ( ( #62766 ) ) GLOBAL_UNIT_ASSIGNED_CONTEXT ( ( #61663, #3417, #24744 ) ) REPRESENTATION_CONTEXT ( 'NONE', 'WORKASPACE' ) );
#771 = CARTESIAN_POINT ( 'NONE',  ( -108.1262211969130362, -277.9935815721493100, -251.8145494874757162 ) ) ;
#772 = CARTESIAN_POINT ( 'NONE',  ( -95.02559501780957874, -278.1079005459940845, -225.0994072091617113 ) ) ;
#773 = CARTESIAN_POINT ( 'NONE',  ( -36.93558084685878384, -273.7238594976064405, -193.3702845615455601 ) ) ;
#774 = CARTESIAN_POINT ( 'NONE',  ( -96.94098799420999057, -247.8563818616659944, -332.2110617558730610 ) ) ;
#775 = CARTESIAN_POINT ( 'NONE',  ( -105.6406974281751303, -277.5723512479806914, -235.9817885254865928 ) ) ;
#776 = CARTESIAN_POINT ( 'NONE',  ( -85.95157403567156962, -281.7497591143824707, -327.0085094357900743 ) ) ;
#777 = CARTESIAN_POINT ( 'NONE',  ( -33.46383412104373889, -296.7641339003956205, -346.2617194651964496 ) ) ;
#778 = VECTOR ( 'NONE', #36386, 1000.000000000000000 ) ;
#779 = CARTESIAN_POINT ( 'NONE',  ( -20.06368573482255968, -292.7724513813253111, -199.3196609204650827 ) ) ;
#780 = CARTESIAN_POINT ( 'NONE',  ( -39.99255981794238579, -287.7708479432874356, -343.8563621197477573 ) ) ;
#781 = CARTESIAN_POINT ( 'NONE',  ( -113.7622917854316569, -273.3107105573316744, -261.8050699941366020 ) ) ;
#782 = CARTESIAN_POINT ( 'NONE',  ( -86.10186548931618233, -297.5199146281921685, -216.0339030858638694 ) ) ;
#783 = VERTEX_POINT ( 'NONE', #12506 ) ;
#784 = CARTESIAN_POINT ( 'NONE',  ( 165.2494399300530290, 8.542400036368780647, 9.000000000000001776 ) ) ;
#785 = CARTESIAN_POINT ( 'NONE',  ( -99.08665254665626776, -281.0595455446512005, -226.8079889331963841 ) ) ;
#786 = CIRCLE ( 'NONE', #77907, 4.999999999999990230 ) ;
#787 = CARTESIAN_POINT ( 'NONE',  ( -37.02071557574380023, -281.1359384565927826, -197.0527075262578762 ) ) ;
#788 = CARTESIAN_POINT ( 'NONE',  ( -110.4592604946704597, -280.0496039754244180, -291.0443571144713246 ) ) ;
#789 = CARTESIAN_POINT ( 'NONE',  ( -37.55320148959520310, -282.1136453882205615, -343.6085773246091435 ) ) ;
#790 = CARTESIAN_POINT ( 'NONE',  ( 15.96154643515947136, -273.3042590122290108, -219.4003769238387349 ) ) ;
#791 = EDGE_CURVE ( 'NONE', #63802, #44165, #5422, .T. ) ;
#792 = CARTESIAN_POINT ( 'NONE',  ( 208.4306832106271088, 0.000000000000000000, 0.000000000000000000 ) ) ;
#793 = EDGE_CURVE ( 'NONE', #79410, #22214, #70290, .T. ) ;
#794 = DIRECTION ( 'NONE',  ( 0.000000000000000000, 0.000000000000000000, 1.000000000000000000 ) ) ;
#795 = CARTESIAN_POINT ( 'NONE',  ( 29.80144657926215146, -275.8684020394861705, -232.8892292355113227 ) ) ;
#796 = CARTESIAN_POINT ( 'NONE',  ( 196.8702642586143270, 40.96915988761478644, 12.42857142857141994 ) ) ;
#797 = CARTESIAN_POINT ( 'NONE',  ( -4.837950822480131308, -278.6242992889652328, -337.9659741168057963 ) ) ;
#798 = CARTESIAN_POINT ( 'NONE',  ( -70.06527597014458308, -276.0494973529995946, -339.4245148474988696 ) ) ;
#799 = EDGE_LOOP ( 'NONE', ( #93336, #90500 ) ) ;
#800 = CARTESIAN_POINT ( 'NONE',  ( 197.0850307134193713, 40.94976125279444545, 10.55987713565813024 ) ) ;
#801 = CARTESIAN_POINT ( 'NONE',  ( 36.81162679258469694, -283.7042654170799665, -283.8378040925136929 ) ) ;
#802 = CARTESIAN_POINT ( 'NONE',  ( -95.23591547362887866, -290.3777209622477926, -225.6301269694029656 ) ) ;
#803 = CARTESIAN_POINT ( 'NONE',  ( 12.01850982276712010, -286.0659370170184843, -211.3265329020892409 ) ) ;
#804 = CARTESIAN_POINT ( 'NONE',  ( -26.61780063314323641, -281.1538624164415978, -343.6454429888399318 ) ) ;
#806 = CARTESIAN_POINT ( 'NONE',  ( 35.40842217358378718, -285.4279737154595864, -254.5898178880433704 ) ) ;
#805 = CARTESIAN_POINT ( 'NONE',  ( -61.74712069394157510, -281.9502078603786686, -339.8392114669903208 ) ) ;
#807 = CARTESIAN_POINT ( 'NONE',  ( 32.61443292740886335, -283.0520645491343998, -292.7364386427111071 ) ) ;
#808 = CARTESIAN_POINT ( 'NONE',  ( -72.97167380842988393, -271.5802567225570670, -204.3071389892957086 ) ) ;
#809 = CARTESIAN_POINT ( 'NONE',  ( -80.46847368171820847, -283.8785524581387563, -207.4760904748688120 ) ) ;
#810 = CARTESIAN_POINT ( 'NONE',  ( -78.36125111334239079, -297.6042968928582013, -333.1496287471148321 ) ) ;
#811 = CARTESIAN_POINT ( 'NONE',  ( -110.4021442392933778, -279.4178257768415961, -276.1092480629901047 ) ) ;
#812 = CARTESIAN_POINT ( 'NONE',  ( -15.95994241996441154, -288.3280766862233122, -198.2456266740734065 ) ) ;
#813 = LINE ( 'NONE', #31437, #58161 ) ;
#814 = CARTESIAN_POINT ( 'NONE',  ( 201.2104617360081704, 25.32700003806615996, 9.000000000000001776 ) ) ;
#815 = CARTESIAN_POINT ( 'NONE',  ( 21.08002887603609921, -294.8165126384732275, -222.4422721897455801 ) ) ;
#816 = CARTESIAN_POINT ( 'NONE',  ( -111.0125257249000441, -276.3706251386071244, -284.4864801008928339 ) ) ;
#817 = CARTESIAN_POINT ( 'NONE',  ( 14.48723273717265236, -287.5424470332873739, -327.1599286408305147 ) ) ;
#818 = CARTESIAN_POINT ( 'NONE',  ( 32.56533995485899169, -291.6392899356585531, -246.5492913139481175 ) ) ;
#819 = CARTESIAN_POINT ( 'NONE',  ( -91.34150605533277201, -276.5251455691686715, -320.2875890802395134 ) ) ;
#820 = CARTESIAN_POINT ( 'NONE',  ( -83.14016282443174077, -293.8260117241777039, -328.8506944977291369 ) ) ;
#821 = CARTESIAN_POINT ( 'NONE',  ( -1.027474884110952891, -293.8600899611792556, -206.4519417833921295 ) ) ;
#822 = DIRECTION ( 'NONE',  ( 0.000000000000000000, 0.000000000000000000, 1.000000000000000000 ) ) ;
#823 = DIRECTION ( 'NONE',  ( 1.000000000000000000, 0.000000000000000000, 0.000000000000000000 ) ) ;
#824 = CARTESIAN_POINT ( 'NONE',  ( -85.96850898010794140, -294.1919638546614806, -329.1670803653922235 ) ) ;
#825 = CARTESIAN_POINT ( 'NONE',  ( 35.55258103312795726, -289.3037453561979646, -281.9684635509040049 ) ) ;
#826 = CARTESIAN_POINT ( 'NONE',  ( -104.2741155191697828, -288.3207402773603576, -306.3336878296482837 ) ) ;
#827 = CARTESIAN_POINT ( 'NONE',  ( 19.98382587014834399, -289.6245471116602062, -316.5039287782337283 ) ) ;
#828 = DIRECTION ( 'NONE',  ( 1.000000000000000000, -0.000000000000000000, -0.000000000000000000 ) ) ;
#829 = CARTESIAN_POINT ( 'NONE',  ( -94.22339290928100297, -290.7056025044375929, -316.3727986070716724 ) ) ;
#830 = DIRECTION ( 'NONE',  ( -0.000000000000000000, -1.000000000000000000, -0.000000000000000000 ) ) ;
#831 = CARTESIAN_POINT ( 'NONE',  ( 22.98430296411414275, -289.3917007370027363, -317.5922224971516243 ) ) ;
#832 = CARTESIAN_POINT ( 'NONE',  ( -105.9117318151228204, -276.9818752618339204, -238.9856587709358280 ) ) ;
#833 = CARTESIAN_POINT ( 'NONE',  ( -33.92045958425376995, -280.4273695767720369, -193.4583260649926331 ) ) ;
#834 = CARTESIAN_POINT ( 'NONE',  ( 29.74138991309138191, -281.7101127769357731, -308.2269072033902830 ) ) ;
#835 = CARTESIAN_POINT ( 'NONE',  ( 35.96011129240598336, -285.7564829485111773, -286.2908819176259954 ) ) ;
#836 = CARTESIAN_POINT ( 'NONE',  ( -111.3408027809598622, -274.2966735324315550, -270.3833299183785357 ) ) ;
#837 = CARTESIAN_POINT ( 'NONE',  ( -84.19936477283708598, -277.5398685475452112, -212.7166139035312824 ) ) ;
#838 = CARTESIAN_POINT ( 'NONE',  ( -31.80989545341614289, -280.9821973052985413, -345.1697616508848228 ) ) ;
#839 = PLANE ( 'NONE',  #10916 ) ;
#840 = CARTESIAN_POINT ( 'NONE',  ( -86.66195202741687353, -276.2028282026039960, -328.6558689310012937 ) ) ;
#841 = AXIS2_PLACEMENT_3D ( 'NONE', #42069, #7056, #77614 ) ;
#842 = CARTESIAN_POINT ( 'NONE',  ( -97.80922045200648540, -282.8396864420637371, -317.5328414729910946 ) ) ;
#843 = CARTESIAN_POINT ( 'NONE',  ( -69.57128714561385152, -274.4194747542948676, -204.6811709041430447 ) ) ;
#844 = CARTESIAN_POINT ( 'NONE',  ( -100.4056891817341750, -292.6744678486936664, -232.0287074297657739 ) ) ;
#845 = CARTESIAN_POINT ( 'NONE',  ( 75.46536863027608888, -300.7518833175248005, -193.8295958960177359 ) ) ;
#846 = CARTESIAN_POINT ( 'NONE',  ( 3.142303339223668335, -276.1582845308063270, -331.1322702669907585 ) ) ;
#847 = CARTESIAN_POINT ( 'NONE',  ( -38.34415815245513670, -297.0648776346940849, -345.3544225554792888 ) ) ;
#848 = CARTESIAN_POINT ( 'NONE',  ( -91.59702342025792632, -289.9655573783689988, -325.0745681992650020 ) ) ;
#849 = CARTESIAN_POINT ( 'NONE',  ( 23.44806425252539128, -279.0242799450177813, -225.4844119210102917 ) ) ;
#850 = CARTESIAN_POINT ( 'NONE',  ( -50.56426823603852228, -291.7210690224612790, -194.5049139045978563 ) ) ;
#851 = CARTESIAN_POINT ( 'NONE',  ( -56.13750644488317931, -288.3588724156700209, -341.1960910039237547 ) ) ;
#852 = CARTESIAN_POINT ( 'NONE',  ( -78.40383310051349497, -293.6046204358681848, -333.1217894481948747 ) ) ;
#853 = ORIENTED_EDGE ( 'NONE', *, *, #21629, .T. ) ;
#854 = CARTESIAN_POINT ( 'NONE',  ( 199.7111327665421072, 66.88064514420912587, 10.01633191836423364 ) ) ;
#855 = CARTESIAN_POINT ( 'NONE',  ( -103.6095035000222992, -290.4747574026792449, -239.5947942224024985 ) ) ;
#856 = FACE_OUTER_BOUND ( 'NONE', #12534, .T. ) ;
#857 = CARTESIAN_POINT ( 'NONE',  ( 7.397043513501998291, -287.5866334202389680, -207.9156505405056237 ) ) ;
#858 = CARTESIAN_POINT ( 'NONE',  ( -6.941161984400275209, -291.1233781216987495, -333.4151289067050357 ) ) ;
#859 = CARTESIAN_POINT ( 'NONE',  ( -74.50299741682368904, -294.5923945951759606, -337.5910194094132066 ) ) ;
#860 = CARTESIAN_POINT ( 'NONE',  ( -44.35720491379382224, -284.4541675825812490, -346.5986523463424192 ) ) ;
#861 = CARTESIAN_POINT ( 'NONE',  ( -110.2280873567793691, -284.4500841960836510, -265.4630893970663692 ) ) ;
#862 = CARTESIAN_POINT ( 'NONE',  ( 27.20785419408808536, -277.3449904248215603, -305.6044022578221302 ) ) ;
#863 = CARTESIAN_POINT ( 'NONE',  ( 11.34570631553869369, -292.3934316537889231, -326.9418855063963747 ) ) ;
#864 = UNCERTAINTY_MEASURE_WITH_UNIT (LENGTH_MEASURE( 1.000000000000000082E-05 ), #46095, 'distance_accuracy_value', 'NONE');
#865 = ADVANCED_FACE ( 'NONE', ( #48951 ), #63665, .F. ) ;
#866 = CARTESIAN_POINT ( 'NONE',  ( 34.51321214708612217, -274.1499004116412834, -255.3330016623347944 ) ) ;
#867 = EDGE_LOOP ( 'NONE', ( #63453, #67407, #86830, #3763 ) ) ;
#868 = CARTESIAN_POINT ( 'NONE',  ( 138.4517698930976621, 181.0451598467585939, -241.7086681466011271 ) ) ;
#869 = CARTESIAN_POINT ( 'NONE',  ( 28.08571317074149576, -293.7505785399827118, -311.0198277226323853 ) ) ;
#870 = CARTESIAN_POINT ( 'NONE',  ( -6.440618138260185255, -288.3813296097144416, -202.6238822446383381 ) ) ;
#871 = CARTESIAN_POINT ( 'NONE',  ( -113.6343124262126594, -297.5338059234313164, -278.1668734224252262 ) ) ;
#872 = CARTESIAN_POINT ( 'NONE',  ( 19.58935568490491264, -287.5559108559137371, -224.4855621633024896 ) ) ;
#873 = CARTESIAN_POINT ( 'NONE',  ( -113.0025450158317284, -277.7736261043972377, -257.3897354765216505 ) ) ;
#874 = CARTESIAN_POINT ( 'NONE',  ( -30.59162539493526367, -295.6203245123036822, -346.9623534663205646 ) ) ;
#875 = CARTESIAN_POINT ( 'NONE',  ( -12.64904773237395652, -286.8742108251241234, -342.0441420440407114 ) ) ;
#876 = CARTESIAN_POINT ( 'NONE',  ( 37.76423380660313001, -294.0973076432025550, -287.2979206696631991 ) ) ;
#877 = CARTESIAN_POINT ( 'NONE',  ( -67.81388237054360957, -291.9741377566406300, -203.9882533135386211 ) ) ;
#878 = DIRECTION ( 'NONE',  ( 0.000000000000000000, 0.000000000000000000, -1.000000000000000000 ) ) ;
#879 = CARTESIAN_POINT ( 'NONE',  ( -29.93913374800817451, -125.2961201612322100, -360.6981843053002876 ) ) ;
#880 = CARTESIAN_POINT ( 'NONE',  ( 37.60552942728433123, -288.8913044591635639, -256.0216432299667417 ) ) ;
#881 = CARTESIAN_POINT ( 'NONE',  ( -2.659677404128736544, -286.1237833571631768, -342.4524372437778652 ) ) ;
#882 = ORIENTED_EDGE ( 'NONE', *, *, #83721, .T. ) ;
#883 = CARTESIAN_POINT ( 'NONE',  ( -86.73289319668791109, -278.7350365296442192, -211.3525748638704442 ) ) ;
#884 = CARTESIAN_POINT ( 'NONE',  ( 25.68802065633659382, -284.0977715745560204, -310.7960192280100387 ) ) ;
#885 = CARTESIAN_POINT ( 'NONE',  ( -113.3199147267640257, -283.0245608065034730, -278.4800587053243817 ) ) ;
#886 = CARTESIAN_POINT ( 'NONE',  ( -59.13358558329213821, -287.4160669487540645, -341.5938146063364229 ) ) ;
#887 = CARTESIAN_POINT ( 'NONE',  ( 28.85658233711649956, -276.9258151481580512, -233.4009841087603263 ) ) ;
#888 = CARTESIAN_POINT ( 'NONE',  ( -94.50338430842838022, -297.6865353482889986, -224.8580378279809793 ) ) ;
#889 = CARTESIAN_POINT ( 'NONE',  ( 27.58594934652676045, -292.7041980245496688, -304.9029987285169341 ) ) ;
#890 = CARTESIAN_POINT ( 'NONE',  ( -72.46765928994960859, -280.2510218501404324, -201.9397621900457693 ) ) ;
#892 = CARTESIAN_POINT ( 'NONE',  ( -94.01430263645522700, -278.5534451031831509, -224.1863543828957290 ) ) ;
#891 = CARTESIAN_POINT ( 'NONE',  ( 35.10608272257667295, -275.6756949264022296, -279.7263342099862484 ) ) ;
#893 = CARTESIAN_POINT ( 'NONE',  ( 4.682238158189504063, -275.6844985772212908, -206.1461012879581745 ) ) ;
#894 = CARTESIAN_POINT ( 'NONE',  ( 3.325883021990954092, -275.4399158623971289, -335.4439294335471686 ) ) ;
#895 = CARTESIAN_POINT ( 'NONE',  ( 193.6317248235237400, 279.2590636266914998, -125.8091547554434868 ) ) ;
#896 = CARTESIAN_POINT ( 'NONE',  ( -13.32075081187344345, -274.7401622057311670, -341.4644680875760514 ) ) ;
#897 = CARTESIAN_POINT ( 'NONE',  ( -113.5348082064481758, -298.0583695818863816, -263.9381939740887901 ) ) ;
#898 = CARTESIAN_POINT ( 'NONE',  ( -54.49178911615187815, -276.3376638359844151, -195.3683826091709363 ) ) ;
#899 = EDGE_CURVE ( 'NONE', #67369, #66900, #57022, .T. ) ;
#900 = CARTESIAN_POINT ( 'NONE',  ( 210.2448042458983366, 0.01303144969186963500, -7.291618491801075130 ) ) ;
#901 = CARTESIAN_POINT ( 'NONE',  ( -41.35353448545914290, -287.0801646925061732, -197.1493095816360892 ) ) ;
#902 = CARTESIAN_POINT ( 'NONE',  ( -73.15549711812488454, -287.3445839549407879, -203.2853287080060909 ) ) ;
#903 = CARTESIAN_POINT ( 'NONE',  ( -41.32019378768246298, -285.3493596849029927, -197.3550116065925408 ) ) ;
#904 = CARTESIAN_POINT ( 'NONE',  ( -77.23738224982504619, -277.9077660217334369, -208.2133749869777830 ) ) ;
#905 = CARTESIAN_POINT ( 'NONE',  ( -111.4630947916657249, -286.4768538268582461, -265.4059684462530981 ) ) ;
#906 = CARTESIAN_POINT ( 'NONE',  ( -100.0476087580543521, -277.5619938040289867, -231.5510620201579002 ) ) ;
#907 = EDGE_CURVE ( 'NONE', #12419, #67382, #86299, .T. ) ;
#908 = CARTESIAN_POINT ( 'NONE',  ( -41.86196548030189746, -278.1900880526117703, -343.5433876501726331 ) ) ;
#909 = EDGE_CURVE ( 'NONE', #57029, #39232, #24135, .T. ) ;
#910 = CARTESIAN_POINT ( 'NONE',  ( 5.207498729030233697, -275.1372241978257307, -210.9053760634883474 ) ) ;
#911 = CARTESIAN_POINT ( 'NONE',  ( 39.18188151753595605, -286.2904574326822740, -265.8571199716314482 ) ) ;
#912 = CARTESIAN_POINT ( 'NONE',  ( 38.09420738556068642, -282.1718228230033105, -255.7466498587353101 ) ) ;
#913 = CARTESIAN_POINT ( 'NONE',  ( -21.73234326751586210, -283.3495676913545935, -345.6995204175483991 ) ) ;
#914 = EDGE_LOOP ( 'NONE', ( #28478, #27992, #72584 ) ) ;
#915 = ORIENTED_EDGE ( 'NONE', *, *, #72851, .F. ) ;
#916 = CARTESIAN_POINT ( 'NONE',  ( 197.9834613664963001, 18.87240044341482914, -11.15593255764641967 ) ) ;
#917 = CARTESIAN_POINT ( 'NONE',  ( 27.85312228968123804, -289.9236316028311649, -308.9608667980314181 ) ) ;
#918 = CARTESIAN_POINT ( 'NONE',  ( -105.5567719990287827, -289.6871790054909184, -235.6033080927602441 ) ) ;
#919 = CARTESIAN_POINT ( 'NONE',  ( -60.55747184931169613, -296.9404801215839598, -200.9272070775346606 ) ) ;
#920 = CARTESIAN_POINT ( 'NONE',  ( 11.06107270794584707, -292.0504144434183900, -210.5390736144928781 ) ) ;
#921 = CARTESIAN_POINT ( 'NONE',  ( 35.44096400160235305, -286.1839987365116826, -281.9909303770633642 ) ) ;
#922 = CARTESIAN_POINT ( 'NONE',  ( 32.21200578076647503, -288.4475306472336911, -246.9215680932040584 ) ) ;
#923 = CARTESIAN_POINT ( 'NONE',  ( -20.19161114001083490, -297.3376638359846424, -345.3538533559490702 ) ) ;
#924 = CARTESIAN_POINT ( 'NONE',  ( -36.09388859611323852, -291.0366967872948294, -345.3635108684193256 ) ) ;
#925 = CARTESIAN_POINT ( 'NONE',  ( -56.84047808315676065, -287.3027138232282596, -343.0084844117062062 ) ) ;
#926 = CARTESIAN_POINT ( 'NONE',  ( -82.93186140916870386, -284.6345351891668543, -327.7406281803029060 ) ) ;
#927 = CARTESIAN_POINT ( 'NONE',  ( -108.1301928377422996, -292.2236681056449470, -295.7940793540527693 ) ) ;
#928 = CARTESIAN_POINT ( 'NONE',  ( 82.15603094527575934, -298.9910830478302159, -193.4355229634127795 ) ) ;
#929 = APPLICATION_CONTEXT ( 'automotive_design' ) ;
#930 = DIRECTION ( 'NONE',  ( 0.000000000000000000, 1.000000000000000000, 0.000000000000000000 ) ) ;
#931 = CARTESIAN_POINT ( 'NONE',  ( -32.06024178434928729, -300.0379246320565585, -194.7993979984996713 ) ) ;
#932 = CARTESIAN_POINT ( 'NONE',  ( 18.61126016977251751, -281.4176509715402403, -317.5172562330616870 ) ) ;
#933 = CARTESIAN_POINT ( 'NONE',  ( -79.52190423584431755, -281.6218152193807782, -332.3758825793864276 ) ) ;
#934 = CARTESIAN_POINT ( 'NONE',  ( -34.87009877148700809, -294.2190133407408439, -347.1598810435261839 ) ) ;
#935 = CARTESIAN_POINT ( 'NONE',  ( -102.9180141350952340, -271.2539721410189486, -235.9322371201628528 ) ) ;
#936 = CARTESIAN_POINT ( 'NONE',  ( 33.46041149705509810, -273.9310737872325490, -293.3475310819709989 ) ) ;
#937 = CARTESIAN_POINT ( 'NONE',  ( -82.25866614509931196, -298.7400811430143790, -212.1269462908238097 ) ) ;
#938 = CARTESIAN_POINT ( 'NONE',  ( 140.6539576904058606, 249.5000000000000568, 12.50000000000000000 ) ) ;
#939 = CARTESIAN_POINT ( 'NONE',  ( -94.82974042097328038, -294.1118501104623419, -320.0511495663456571 ) ) ;
#940 = EDGE_CURVE ( 'NONE', #59842, #18158, #80294, .T. ) ;
#941 = CARTESIAN_POINT ( 'NONE',  ( -26.09963061835976816, -296.3314905084831139, -343.0865659981205908 ) ) ;
#942 = DIRECTION ( 'NONE',  ( 0.000000000000000000, 0.000000000000000000, 1.000000000000000000 ) ) ;
#943 = CARTESIAN_POINT ( 'NONE',  ( -55.83427369241110938, -296.0991008964558091, -341.1993936045574287 ) ) ;
#944 = CARTESIAN_POINT ( 'NONE',  ( 195.7510731661265595, -142.7221692137691775, 21.50000000000000000 ) ) ;
#946 = CARTESIAN_POINT ( 'NONE',  ( -110.0992216245961401, -296.4658981593526050, -276.8996432020963425 ) ) ;
#945 = CARTESIAN_POINT ( 'NONE',  ( -112.5091102700940127, -282.6490287972261513, -264.3537110432848749 ) ) ;
#947 = CARTESIAN_POINT ( 'NONE',  ( -92.43373764308211094, -283.8142233278933872, -324.1557961807400829 ) ) ;
#948 = CARTESIAN_POINT ( 'NONE',  ( 25.53737957532825575, -284.0342829684607864, -312.2602293522240871 ) ) ;
#949 = CARTESIAN_POINT ( 'NONE',  ( 12.06725818327686461, -286.3840178553754185, -211.2619120057407827 ) ) ;
#950 = CARTESIAN_POINT ( 'NONE',  ( 16.20471157591834910, -290.8135480297377740, -218.0105845512304086 ) ) ;
#951 = CARTESIAN_POINT ( 'NONE',  ( -112.2420342695258313, -277.9642507728015630, -253.2118099222299179 ) ) ;
#952 = CARTESIAN_POINT ( 'NONE',  ( -95.99890600148557951, -281.4094976428775681, -317.0979686699210447 ) ) ;
#953 = CARTESIAN_POINT ( 'NONE',  ( -43.47555712338063927, -255.2612651217553434, -494.0498651529597964 ) ) ;
#954 = CARTESIAN_POINT ( 'NONE',  ( 35.14898454146587881, -286.4989941086593035, -281.9402881070710691 ) ) ;
#955 = CARTESIAN_POINT ( 'NONE',  ( -54.44610676298083263, -288.1871189736680208, -345.1747707523663280 ) ) ;
#956 = CARTESIAN_POINT ( 'NONE',  ( -100.5928439528197202, -298.6709374801468471, -232.2388944273133973 ) ) ;
#957 = CARTESIAN_POINT ( 'NONE',  ( -110.7760353280859675, -280.2442397757020558, -249.2422944540280412 ) ) ;
#959 = CARTESIAN_POINT ( 'NONE',  ( 35.72392568591476447, -281.2314915197200094, -271.3182695534003983 ) ) ;
#958 = CARTESIAN_POINT ( 'NONE',  ( -22.44783362419774519, -292.8824680474103275, -344.2297821128346982 ) ) ;
#960 = CARTESIAN_POINT ( 'NONE',  ( 33.41740802365017515, -294.1071294063391406, -300.8626818259278366 ) ) ;
#961 = CARTESIAN_POINT ( 'NONE',  ( -2.857853123212670710, -284.5841079123286477, -203.1143665305021102 ) ) ;
#962 = CARTESIAN_POINT ( 'NONE',  ( -94.40124125525481702, -281.2264783105441666, -221.6668586528346907 ) ) ;
#963 = CARTESIAN_POINT ( 'NONE',  ( -110.6093951094849928, -295.6325305761101845, -268.7156878205362318 ) ) ;
#964 = ORIENTED_EDGE ( 'NONE', *, *, #41918, .T. ) ;
#965 = PLANE ( 'NONE',  #3028 ) ;
#966 = CARTESIAN_POINT ( 'NONE',  ( 35.35669359156745628, -283.3135614387476267, -253.4262321628382040 ) ) ;
#967 = CARTESIAN_POINT ( 'NONE',  ( 175.2296996224750103, 214.5000000000000568, 0.000000000000000000 ) ) ;
#968 = CARTESIAN_POINT ( 'NONE',  ( -54.42813229853333468, -277.3380690714490697, -195.3538533559490702 ) ) ;
#969 = CARTESIAN_POINT ( 'NONE',  ( -35.51735102929995946, -273.2716381086009392, -193.5311515974589440 ) ) ;
#970 = CARTESIAN_POINT ( 'NONE',  ( -106.0332877464310286, -290.0564094396924588, -295.0687239970229712 ) ) ;
#971 = CARTESIAN_POINT ( 'NONE',  ( -11.51815736585606054, -281.9146998990236739, -201.2864930753476642 ) ) ;
#972 = CARTESIAN_POINT ( 'NONE',  ( -4.975394387236288907, -276.0856964431934557, -204.0232223557427460 ) ) ;
#973 = CARTESIAN_POINT ( 'NONE',  ( 36.42256047748497139, -283.3939899960176376, -289.4732679058714666 ) ) ;
#974 = CARTESIAN_POINT ( 'NONE',  ( 5.813239184487858147, -281.2472027869869748, -329.7309901121471398 ) ) ;
#975 = CARTESIAN_POINT ( 'NONE',  ( -37.79701941603578064, -279.0579763704753304, -345.3725346836218932 ) ) ;
#976 = EDGE_LOOP ( 'NONE', ( #39122, #15194, #45097, #86820 ) ) ;
#977 = CARTESIAN_POINT ( 'NONE',  ( 4.864935244613048049, -274.4383479087302931, -205.8959925199068550 ) ) ;
#978 = CARTESIAN_POINT ( 'NONE',  ( 24.52468685203869114, -294.9084711916231072, -228.9622730710885037 ) ) ;
#979 = CARTESIAN_POINT ( 'NONE',  ( 201.8074164582889125, 62.71404347880360319, -8.782170572880787063 ) ) ;
#980 = CARTESIAN_POINT ( 'NONE',  ( 160.5350683151633291, 250.5000000000000568, 20.22542485937379908 ) ) ;
#981 = CARTESIAN_POINT ( 'NONE',  ( 22.18623702242076945, -292.3289950001711759, -317.2512136965749505 ) ) ;
#982 = CARTESIAN_POINT ( 'NONE',  ( -0.5098349863465404530, -274.0635525867834872, -207.2481611531588044 ) ) ;
#983 = CARTESIAN_POINT ( 'NONE',  ( 193.9153122143737562, 214.9910457053126720, 17.21343741151142481 ) ) ;
#984 = CARTESIAN_POINT ( 'NONE',  ( 8.419526694714949855, -294.1856584809298738, -209.2327734719434886 ) ) ;
#986 = CARTESIAN_POINT ( 'NONE',  ( -16.74818689177746478, -293.5175093448845587, -196.5782207085586606 ) ) ;
#985 = CARTESIAN_POINT ( 'NONE',  ( -37.37352853689063892, -282.5519495502701943, -195.3611179825600175 ) ) ;
#987 = CARTESIAN_POINT ( 'NONE',  ( -2.490413321436029559, -290.5905754256617115, -336.6409961592946729 ) ) ;
#988 = CARTESIAN_POINT ( 'NONE',  ( 35.95524251878263300, -273.7461268672862502, -285.4470925500735348 ) ) ;
#989 = CARTESIAN_POINT ( 'NONE',  ( -32.29905878450974654, -278.9083651082324877, -344.6810802384226236 ) ) ;
#990 = CARTESIAN_POINT ( 'NONE',  ( 34.12595542525693304, -291.9026829951419018, -291.2320673009564871 ) ) ;
#991 = CARTESIAN_POINT ( 'NONE',  ( -4.219348060625711661, -282.3445218360288322, -202.2056929960885157 ) ) ;
#992 =( BOUNDED_CURVE ( )  B_SPLINE_CURVE ( 3, ( #17869, #39604, #3665, #9823 ),
 .UNSPECIFIED., .F., .T. ) 
 B_SPLINE_CURVE_WITH_KNOTS ( ( 4, 4 ),
 ( 0.000000000000000000, 1.570796326794896558 ),
 .UNSPECIFIED. ) 
 CURVE ( )  GEOMETRIC_REPRESENTATION_ITEM ( )  RATIONAL_B_SPLINE_CURVE ( ( 1.000000000000000000, 0.8047378541243649375, 0.8047378541243649375, 1.000000000000000000 ) ) 
 REPRESENTATION_ITEM ( '' )  );
#993 = ORIENTED_EDGE ( 'NONE', *, *, #1573, .T. ) ;
#994 = CARTESIAN_POINT ( 'NONE',  ( -24.06581367699070739, -282.5446068761607421, -342.1652844746584492 ) ) ;
#995 = CARTESIAN_POINT ( 'NONE',  ( -74.86872700455558061, -280.6441707290950376, -203.4790219939885105 ) ) ;
#996 =( BOUNDED_CURVE ( )  B_SPLINE_CURVE ( 3, ( #21405, #22335, #16165, #31310 ),
 .UNSPECIFIED., .F., .F. ) 
 B_SPLINE_CURVE_WITH_KNOTS ( ( 4, 4 ),
 ( 1.570796326794896558, 3.141592653589793116 ),
 .UNSPECIFIED. ) 
 CURVE ( )  GEOMETRIC_REPRESENTATION_ITEM ( )  RATIONAL_B_SPLINE_CURVE ( ( 1.000000000000000000, 0.8047378541243649375, 0.8047378541243649375, 1.000000000000000000 ) ) 
 REPRESENTATION_ITEM ( '' )  );
#997 = CARTESIAN_POINT ( 'NONE',  ( 0.6579846690457067382, -281.3521927483833451, -336.8896722809365656 ) ) ;
#998 = CARTESIAN_POINT ( 'NONE',  ( -14.64778039991939096, -277.7064287355931356, -343.7503030558007140 ) ) ;
#999 = EDGE_CURVE ( 'NONE', #46709, #71428, #37410, .T. ) ;
#1000 = DIRECTION ( 'NONE',  ( 1.000000000000000000, 0.000000000000000000, 0.000000000000000000 ) ) ;
#1001 = CARTESIAN_POINT ( 'NONE',  ( 27.89961750840676302, -276.5497980251693093, -230.6839122871389236 ) ) ;
#1002 = CARTESIAN_POINT ( 'NONE',  ( -105.5795714935544112, -286.8376638359844719, -285.9686137636504668 ) ) ;
#1003 = ORIENTED_EDGE ( 'NONE', *, *, #5970, .F. ) ;
#1004 = CARTESIAN_POINT ( 'NONE',  ( -67.65030268694809479, -299.6546725967230032, -201.7439321594510773 ) ) ;
#1005 = CARTESIAN_POINT ( 'NONE',  ( -79.58310737088281428, -275.6456418185090342, -331.9668237205792138 ) ) ;
#1006 = CARTESIAN_POINT ( 'NONE',  ( -111.5705844000524536, -292.1063541941880430, -286.6106335787735588 ) ) ;
#1007 = CARTESIAN_POINT ( 'NONE',  ( -17.39682783762583185, -291.6648620706661745, -199.9799727888749601 ) ) ;
#1008 = CARTESIAN_POINT ( 'NONE',  ( -3.093761974300191397, -288.1195746266095057, -339.2713484225133129 ) ) ;
#1009 = CARTESIAN_POINT ( 'NONE',  ( 165.0704140682094589, 2.965303559109564890, 10.00000000000000000 ) ) ;
#1011 = CARTESIAN_POINT ( 'NONE',  ( -110.8947407714575348, -282.8733013534049974, -276.3935823160416589 ) ) ;
#1010 = CARTESIAN_POINT ( 'NONE',  ( 33.91993294284144156, -291.7732104812580474, -242.6397112975752464 ) ) ;
#1012 = CARTESIAN_POINT ( 'NONE',  ( -110.1455382575282300, -292.2235340083572623, -284.9335032823274219 ) ) ;
#1013 = CARTESIAN_POINT ( 'NONE',  ( -100.1906034999029202, -283.5584432064873113, -231.7837677653867274 ) ) ;
#1014 = ADVANCED_FACE ( 'NONE', ( #2837 ), #75763, .T. ) ;
#1015 = CARTESIAN_POINT ( 'NONE',  ( -71.62417836667094662, -284.8303029174610401, -335.3684649896103451 ) ) ;
#1016 = CARTESIAN_POINT ( 'NONE',  ( -62.67465757400178461, -290.3150765332896412, -342.8815348908123042 ) ) ;
#1017 = B_SPLINE_CURVE_WITH_KNOTS ( 'NONE', 3,
 ( #237, #56627, #85477, #93503, #42373, #57546, #29117, #35287 ),
 .UNSPECIFIED., .F., .F.,
 ( 4, 2, 2, 4 ),
 ( -1.794524598959325299E-05, 0.004652435581272471032, 0.006987625994903502377, 0.009322816408534533722 ),
 .UNSPECIFIED. ) ;
#1018 = CARTESIAN_POINT ( 'NONE',  ( 35.49091247449603514, -282.1287150791714566, -276.7502876014257254 ) ) ;
#1019 = CARTESIAN_POINT ( 'NONE',  ( 26.17232062719289232, -291.7788378357195143, -227.4428137465853865 ) ) ;
#1020 = CARTESIAN_POINT ( 'NONE',  ( 2.648228718991627595, -287.3769849079112078, -204.7488903786906462 ) ) ;
#1021 = CARTESIAN_POINT ( 'NONE',  ( 14.56681859312259952, -288.8374182808695423, -327.2226890994894575 ) ) ;
#1022 = CARTESIAN_POINT ( 'NONE',  ( -30.53339763175301869, -286.3071789976789319, -197.6284991167072178 ) ) ;
#1023 = VERTEX_POINT ( 'NONE', #983 ) ;
#1024 = CARTESIAN_POINT ( 'NONE',  ( 195.7077576554793836, 26.39544325298913918, 13.66612345222623404 ) ) ;
#1025 = CARTESIAN_POINT ( 'NONE',  ( -50.23365427689127216, -297.0752956370846505, -345.0741110681527175 ) ) ;
#1026 = CARTESIAN_POINT ( 'NONE',  ( -68.04375013930707894, -294.1317519961890525, -340.4373792911929399 ) ) ;
#1027 = CARTESIAN_POINT ( 'NONE',  ( -87.68369393546051072, -278.3871389489561352, -217.1018354939701567 ) ) ;
#1028 = CARTESIAN_POINT ( 'NONE',  ( -68.12901672938096453, -297.0070944078794923, -199.8384217942894736 ) ) ;
#1029 = CARTESIAN_POINT ( 'NONE',  ( 20.74120918621679621, -291.3985485119546865, -224.9856012037972164 ) ) ;
#1030 = CARTESIAN_POINT ( 'NONE',  ( -2.455553030725395214, -276.2804968083602262, -205.0853126957729557 ) ) ;
#1031 = CARTESIAN_POINT ( 'NONE',  ( -111.3983774615681170, -294.7777569590534767, -271.4560451633701064 ) ) ;
#1032 = CARTESIAN_POINT ( 'NONE',  ( 19.64442711626699989, -294.1060809516100107, -224.0842267476853635 ) ) ;
#1033 = CARTESIAN_POINT ( 'NONE',  ( 32.64598668094742351, -294.9197028558654665, -292.1773910120720075 ) ) ;
#1034 = CARTESIAN_POINT ( 'NONE',  ( -43.21052124919093984, -280.7960701182722687, -430.6442049081570644 ) ) ;
#1035 = CARTESIAN_POINT ( 'NONE',  ( -34.93937233869628045, -293.0218790329423086, -345.4893899621767446 ) ) ;
#1036 = CARTESIAN_POINT ( 'NONE',  ( -77.72765701591760035, -299.5104587434639143, -207.1024028966750450 ) ) ;
#1037 = CARTESIAN_POINT ( 'NONE',  ( -31.84175907741981248, -289.9224447074661839, -343.4403859512186727 ) ) ;
#1038 = CARTESIAN_POINT ( 'NONE',  ( -77.95797922591019358, -295.9476078057366522, -331.1050152731499452 ) ) ;
#1039 = CARTESIAN_POINT ( 'NONE',  ( -93.74771131835602489, -281.2237479961370923, -220.3934413704049859 ) ) ;
#1040 = CARTESIAN_POINT ( 'NONE',  ( -102.9798362976808761, -277.7539956174660460, -230.9525056298894583 ) ) ;
#1041 = CARTESIAN_POINT ( 'NONE',  ( 4.814224570445547968, -273.9536928217604554, -205.9847119525065864 ) ) ;
#1042 = CARTESIAN_POINT ( 'NONE',  ( 26.38138932523645863, -279.1114354533789310, -231.7815413472453656 ) ) ;
#1043 = CARTESIAN_POINT ( 'NONE',  ( -40.94991361842823352, -278.4073685721277798, -194.2335325142391582 ) ) ;
#1044 = CARTESIAN_POINT ( 'NONE',  ( -78.87602176098383211, -277.4940363661532388, -207.6494441230378243 ) ) ;
#1045 = CARTESIAN_POINT ( 'NONE',  ( -96.74636351259668743, -271.7312411991802037, -226.8430752619213422 ) ) ;
#1046 = CARTESIAN_POINT ( 'NONE',  ( 36.52757507304578155, -277.3847850654564695, -257.3137226342531108 ) ) ;
#1047 = DIRECTION ( 'NONE',  ( -1.000000000000000000, 0.000000000000000000, 0.000000000000000000 ) ) ;
#1048 = CARTESIAN_POINT ( 'NONE',  ( -80.95740930335308860, -289.4832423238537444, -208.9113278011794819 ) ) ;
#1049 = CARTESIAN_POINT ( 'NONE',  ( -102.3012601845920813, -290.0091174574806132, -311.8023811898784174 ) ) ;
#1050 = CARTESIAN_POINT ( 'NONE',  ( -73.09581931445028147, -275.5799314238806232, -204.1846322639948710 ) ) ;
#1051 = CARTESIAN_POINT ( 'NONE',  ( -111.0917832501413613, -270.7306310493452770, -256.4483517006355555 ) ) ;
#1052 = CARTESIAN_POINT ( 'NONE',  ( -63.13758041765268558, -284.9216999928629548, -197.9820368860418398 ) ) ;
#1053 = CARTESIAN_POINT ( 'NONE',  ( 143.6449502718966755, 0.000000000000000000, 10.00000000000000178 ) ) ;
#1054 = CARTESIAN_POINT ( 'NONE',  ( 7.283460102669957692, -280.4442333741813513, -330.7041645467697322 ) ) ;
#1055 = CARTESIAN_POINT ( 'NONE',  ( 198.6746746775679355, 25.20017525016920246, 11.14960445189099225 ) ) ;
#1056 = CARTESIAN_POINT ( 'NONE',  ( 30.22726478279970408, -291.9627847652411106, -241.5680615429741920 ) ) ;
#1057 = CARTESIAN_POINT ( 'NONE',  ( -19.49636631882197335, -284.4237012843408934, -198.3027420730902861 ) ) ;
#1058 = CARTESIAN_POINT ( 'NONE',  ( 195.0811277904325323, 27.27788670632333989, 15.19607843137264602 ) ) ;
#1059 = CARTESIAN_POINT ( 'NONE',  ( 156.4851178187871312, 0.000000000000000000, -7.000000000000000888 ) ) ;
#1060 = CARTESIAN_POINT ( 'NONE',  ( -5.160997246936801730, -290.4755195668607257, -202.6018229802685084 ) ) ;
#1061 = CARTESIAN_POINT ( 'NONE',  ( -56.79160173907078502, -278.9071419925335817, -341.6050690812330686 ) ) ;
#1062 = CARTESIAN_POINT ( 'NONE',  ( -95.95652540879055437, -285.0894613208590158, -319.6998732974388417 ) ) ;
#1064 = CARTESIAN_POINT ( 'NONE',  ( -89.66285601298389452, -285.2889704125552157, -219.3818339802222681 ) ) ;
#1063 = CARTESIAN_POINT ( 'NONE',  ( 23.33833486314566485, -273.0219709064349445, -225.3361520858668996 ) ) ;
#1065 = CARTESIAN_POINT ( 'NONE',  ( 34.40420059604100800, -276.7625747367278564, -253.9371706092239265 ) ) ;
#1066 = CARTESIAN_POINT ( 'NONE',  ( -32.39946055657536306, -277.7912239715001306, -343.4055505056790594 ) ) ;
#1067 = CARTESIAN_POINT ( 'NONE',  ( -111.8361580510258761, -286.6639379119470732, -261.6676499405724599 ) ) ;
#1068 = EDGE_LOOP ( 'NONE', ( #54068, #62858, #68288, #37860 ) ) ;
#1069 = CARTESIAN_POINT ( 'NONE',  ( 175.2296996224749250, 276.0000000000000568, -24.99999999999999289 ) ) ;
#1070 = CARTESIAN_POINT ( 'NONE',  ( -105.9586663602423329, -295.9342305605439378, -305.4172663811372672 ) ) ;
#1071 = CARTESIAN_POINT ( 'NONE',  ( -28.96403834222452645, -290.9253240127049480, -344.5343044090064382 ) ) ;
#1072 = DIRECTION ( 'NONE',  ( 0.000000000000000000, 1.000000000000000000, 0.000000000000000000 ) ) ;
#1073 = CARTESIAN_POINT ( 'NONE',  ( -99.86837403722181250, -280.4090924074130839, -320.2651865833026363 ) ) ;
#1074 = CARTESIAN_POINT ( 'NONE',  ( -74.84472348819954846, -278.4851765789962883, -203.4655594688400697 ) ) ;
#1075 = CARTESIAN_POINT ( 'NONE',  ( 16.97682621455858509, -292.6941502471668173, -323.8771238473130438 ) ) ;
#1076 = CARTESIAN_POINT ( 'NONE',  ( 15.51342248968685134, -288.3367469005635257, -219.0089635461066848 ) ) ;
#1077 = CARTESIAN_POINT ( 'NONE',  ( -109.7515702377337732, -280.1129305147493938, -285.6838046556247832 ) ) ;
#1078 = CARTESIAN_POINT ( 'NONE',  ( 33.50290191486368485, -289.3452869432337025, -299.1316415469081562 ) ) ;
#1079 = CARTESIAN_POINT ( 'NONE',  ( -51.36761110440766487, -285.2315219378303368, -344.0909291930940412 ) ) ;
#1080 = CARTESIAN_POINT ( 'NONE',  ( -98.80214108853407140, -278.1008545729783350, -316.7682528913188094 ) ) ;
#1081 = CARTESIAN_POINT ( 'NONE',  ( -63.63577030268957913, -295.7279645418488485, -200.4460907883798768 ) ) ;
#1082 = CARTESIAN_POINT ( 'NONE',  ( -88.92987249621317858, -279.1839301068368400, -213.1976639563723666 ) ) ;
#1083 = CARTESIAN_POINT ( 'NONE',  ( -108.3854495593476059, -274.6950023225707014, -248.6522826635056731 ) ) ;
#1084 = CARTESIAN_POINT ( 'NONE',  ( 201.9208557708175249, 300.1658636863270431, -5.053462443409009630 ) ) ;
#1085 = CARTESIAN_POINT ( 'NONE',  ( -85.28047601435908120, -286.1948066931273615, -330.5268031993605859 ) ) ;
#1086 = CARTESIAN_POINT ( 'NONE',  ( -10.68186013637759224, -272.6348704612724987, -199.1487784743132465 ) ) ;
#1087 = CARTESIAN_POINT ( 'NONE',  ( 175.2296996224750103, 250.5000000000000568, 0.000000000000000000 ) ) ;
#1088 = CARTESIAN_POINT ( 'NONE',  ( -92.25054720890470605, -278.7473530858525805, -222.1445057983821698 ) ) ;
#1089 = CARTESIAN_POINT ( 'NONE',  ( 8.018354576881192131, -277.6528932049073433, -332.1558390401979182 ) ) ;
#1090 = CARTESIAN_POINT ( 'NONE',  ( -95.76787336223216585, -298.6020088580048082, -225.5995783673533026 ) ) ;
#1091 = CARTESIAN_POINT ( 'NONE',  ( -108.0152221341671321, -283.2267562136801757, -300.4650276262655666 ) ) ;
#1092 = CARTESIAN_POINT ( 'NONE',  ( 35.52319090334380292, -289.4812808199564529, -283.3488687464272289 ) ) ;
#1093 = CARTESIAN_POINT ( 'NONE',  ( -51.68940292160099403, -299.3920739648045810, -195.3616105337451643 ) ) ;
#1094 = CARTESIAN_POINT ( 'NONE',  ( -111.8914892694033369, -297.9786938558639804, -252.7447148475994254 ) ) ;
#1095 = CARTESIAN_POINT ( 'NONE',  ( -4.719850195966968975, -296.6216490810683695, -337.7239481761257593 ) ) ;
#1096 = CARTESIAN_POINT ( 'NONE',  ( 26.71855632994155982, -279.0314419247802107, -231.5784512824415913 ) ) ;
#1097 = CARTESIAN_POINT ( 'NONE',  ( -0.8980460531410958680, -272.5585906576740172, -205.2027395754095949 ) ) ;
#1098 = CARTESIAN_POINT ( 'NONE',  ( 28.00192510623821462, -288.6345080858802703, -231.0592566860217119 ) ) ;
#1099 = CARTESIAN_POINT ( 'NONE',  ( -100.5775226989478881, -288.9642007296278621, -307.5482832304992371 ) ) ;
#1100 = CARTESIAN_POINT ( 'NONE',  ( 198.9745609140036606, 284.0578480540463602, -111.6648769956217535 ) ) ;
#1101 = ORIENTED_EDGE ( 'NONE', *, *, #12784, .T. ) ;
#1102 = CARTESIAN_POINT ( 'NONE',  ( 23.66076176483710825, -286.7443653981940770, -316.3753107662619186 ) ) ;
#1103 = CARTESIAN_POINT ( 'NONE',  ( -74.73037293595314168, -289.2313689901456542, -333.0988087027815823 ) ) ;
#1104 = EDGE_LOOP ( 'NONE', ( #42911, #32160, #59830, #16502 ) ) ;
#1105 = CARTESIAN_POINT ( 'NONE',  ( -83.10249885895767363, -286.5220519591247808, -208.7526911711092907 ) ) ;
#1106 = CARTESIAN_POINT ( 'NONE',  ( -56.60166329816466657, -277.6404986654090976, -340.8489998805523555 ) ) ;
#1107 = CARTESIAN_POINT ( 'NONE',  ( -0.9384164133903355465, -291.4442618767709519, -202.8607961676685534 ) ) ;
#1108 = CARTESIAN_POINT ( 'NONE',  ( 36.07591863791223119, -281.9158374490495476, -247.4882947784958276 ) ) ;
#1109 = EDGE_CURVE ( 'NONE', #44168, #80534, #22737, .T. ) ;
#1110 = CARTESIAN_POINT ( 'NONE',  ( 34.95844376996689107, -283.3842659259722723, -294.9262075890190999 ) ) ;
#1111 = CARTESIAN_POINT ( 'NONE',  ( 4.537755288195992165, -282.8372464690514221, -335.0140232264483870 ) ) ;
#1112 = CARTESIAN_POINT ( 'NONE',  ( -1.959548566176730233, -280.8678831060333891, -206.4847464695805570 ) ) ;
#1113 = CARTESIAN_POINT ( 'NONE',  ( 174.3702828278471202, 243.3002394640316766, -179.7950274582404120 ) ) ;
#1114 = CARTESIAN_POINT ( 'NONE',  ( -100.7144291363231048, -280.0150311131046692, -310.2564250008069280 ) ) ;
#1115 = CARTESIAN_POINT ( 'NONE',  ( 4.499940650622777483, -57.89452529514181833, -353.9072000911820055 ) ) ;
#1116 = CARTESIAN_POINT ( 'NONE',  ( 191.9139817438699822, 276.9408567967533372, -124.2323592714584777 ) ) ;
#1117 = CARTESIAN_POINT ( 'NONE',  ( -108.6901069843859489, -271.9623749435439208, -254.1745010833050742 ) ) ;
#1118 = CARTESIAN_POINT ( 'NONE',  ( 38.79193668294810493, -292.9164059715525354, -258.9040720017960098 ) ) ;
#1119 = CARTESIAN_POINT ( 'NONE',  ( -107.0837456695891348, -264.9657348211522958, -305.5179930709127802 ) ) ;
#1121 = CARTESIAN_POINT ( 'NONE',  ( -10.45139258062658172, -287.0953617368729738, -339.1425665127841285 ) ) ;
#1120 = CARTESIAN_POINT ( 'NONE',  ( -91.80616674160452817, -271.9798102298358344, -216.6310505271245859 ) ) ;
#1122 = CARTESIAN_POINT ( 'NONE',  ( -8.733334960409219860, -296.5342515798746490, -338.8762476456487889 ) ) ;
#1123 = CARTESIAN_POINT ( 'NONE',  ( 33.50019461619996264, -288.6105727994026324, -250.7991797362542172 ) ) ;
#1124 = ORIENTED_EDGE ( 'NONE', *, *, #88943, .T. ) ;
#1125 = CARTESIAN_POINT ( 'NONE',  ( 4.110360476094063742, -295.4498316236593496, -335.0344413311789822 ) ) ;
#1126 = CARTESIAN_POINT ( 'NONE',  ( -46.73899239170622621, -286.4221153722847930, -197.8556285555808643 ) ) ;
#1127 = CARTESIAN_POINT ( 'NONE',  ( -52.47113154244657807, -272.7832085550333545, -195.1231704729238743 ) ) ;
#1128 = CARTESIAN_POINT ( 'NONE',  ( -69.56478962876855121, -292.4415673326432170, -200.5912948374864584 ) ) ;
#1129 = CARTESIAN_POINT ( 'NONE',  ( 25.66786172475784866, -294.6290315133653053, -314.5352401015075543 ) ) ;
#1130 = CARTESIAN_POINT ( 'NONE',  ( -108.1089997933592315, -290.9559001142337138, -252.3940989468879650 ) ) ;
#1131 = ORIENTED_EDGE ( 'NONE', *, *, #65065, .F. ) ;
#1132 = CARTESIAN_POINT ( 'NONE',  ( -80.44930343749901169, -275.3935366908764877, -208.2408831466813979 ) ) ;
#1133 = CARTESIAN_POINT ( 'NONE',  ( -1.473759650709204561, -273.3119385549804292, -202.6743425727264594 ) ) ;
#1134 = ADVANCED_FACE ( 'NONE', ( #58749 ), #55660, .T. ) ;
#1135 = VERTEX_POINT ( 'NONE', #59209 ) ;
#1136 = CARTESIAN_POINT ( 'NONE',  ( -25.78540478833620497, -276.4163586253898757, -346.4267405798486266 ) ) ;
#1137 = CARTESIAN_POINT ( 'NONE',  ( -66.10637053541185537, -272.0691433264092325, -202.3976413741297904 ) ) ;
#1138 = CARTESIAN_POINT ( 'NONE',  ( -32.36095606487933196, -275.1284053316981613, -344.4798563065289727 ) ) ;
#1139 = CARTESIAN_POINT ( 'NONE',  ( -93.15803736730549645, -274.3051355363830908, -222.8152951516119629 ) ) ;
#1140 = CARTESIAN_POINT ( 'NONE',  ( -105.6400026229400311, -273.8471441581478985, -243.7872833854606824 ) ) ;
#1141 = CARTESIAN_POINT ( 'NONE',  ( -87.38607253133439201, -275.1259472180560124, -213.1112975050200475 ) ) ;
#1142 = EDGE_CURVE ( 'NONE', #4350, #76692, #40467, .T. ) ;
#1143 = CARTESIAN_POINT ( 'NONE',  ( 31.07062864848332850, -273.1578201555006444, -238.6430976653437597 ) ) ;
#1144 = CARTESIAN_POINT ( 'NONE',  ( -108.3961317111346858, -296.9765516566779411, -287.5941142982170504 ) ) ;
#1145 = CARTESIAN_POINT ( 'NONE',  ( -6.534635463886656837, -293.2141614698999206, -337.1914979426683772 ) ) ;
#1146 = DIRECTION ( 'NONE',  ( 0.000000000000000000, 1.000000000000000000, 0.000000000000000000 ) ) ;
#1147 = CARTESIAN_POINT ( 'NONE',  ( 16.91627887158795929, -276.7969609196704823, -324.9845656149531692 ) ) ;
#1148 = CARTESIAN_POINT ( 'NONE',  ( -4.106581969183493719, -274.6697700212742461, -205.3514937019019158 ) ) ;
#1149 = CARTESIAN_POINT ( 'NONE',  ( -112.0472043524662951, -283.0292472786928215, -286.8652360616684405 ) ) ;
#1150 = CARTESIAN_POINT ( 'NONE',  ( -98.44641521233309334, -299.1465021712577936, -226.5862139532879382 ) ) ;
#1151 = CARTESIAN_POINT ( 'NONE',  ( 140.6539576904058606, 275.0000000000000568, -10.49999999999999822 ) ) ;
#1152 = CARTESIAN_POINT ( 'NONE',  ( 15.15246052924810805, -286.0141669556790589, -219.4006938889544358 ) ) ;
#1153 = CARTESIAN_POINT ( 'NONE',  ( -110.1245732095633940, -276.9668736212078670, -256.9213485965001382 ) ) ;
#1154 = CARTESIAN_POINT ( 'NONE',  ( -98.14583666262868178, -276.5548198592151721, -311.8126788427324527 ) ) ;
#1155 = CARTESIAN_POINT ( 'NONE',  ( -61.03100585867067451, -285.3596730798511771, -341.5756631663874714 ) ) ;
#1156 = CARTESIAN_POINT ( 'NONE',  ( -0.3593866511650910534, -275.7607016248830973, -206.9474036374556078 ) ) ;
#1157 = DIRECTION ( 'NONE',  ( -0.000000000000000000, -0.000000000000000000, -1.000000000000000000 ) ) ;
#1158 = CARTESIAN_POINT ( 'NONE',  ( 21.24893732608056851, -273.2899112099784134, -221.6417417495325424 ) ) ;
#1159 = CARTESIAN_POINT ( 'NONE',  ( -8.270145936652498975, -282.4320570641137920, -201.0299653366178916 ) ) ;
#1160 = CARTESIAN_POINT ( 'NONE',  ( 194.7173632872394649, 19.95192844427760193, 14.18452691302933033 ) ) ;
#1161 = CARTESIAN_POINT ( 'NONE',  ( -75.40291243911637764, -287.4693545276017517, -205.0271372972180757 ) ) ;
#1162 = LINE ( 'NONE', #80229, #54661 ) ;
#1163 = CARTESIAN_POINT ( 'NONE',  ( 33.09993806713283249, -291.2162720582772977, -244.4648538759696521 ) ) ;
#1164 = CARTESIAN_POINT ( 'NONE',  ( 82.17077897911026696, -297.8327751790970979, -196.3995604311907641 ) ) ;
#1165 = CARTESIAN_POINT ( 'NONE',  ( -69.41728368265411575, -296.4152365729725602, -204.3437911216519467 ) ) ;
#1166 = CARTESIAN_POINT ( 'NONE',  ( -49.87432899933946828, -290.0303049508679010, -197.1392690500716185 ) ) ;
#1167 = CARTESIAN_POINT ( 'NONE',  ( 193.8665746513534316, 275.1768195097669150, -123.9090917457166938 ) ) ;
#1168 = CARTESIAN_POINT ( 'NONE',  ( 180.2288731078812702, 214.9910457053126720, -24.90909090909092782 ) ) ;
#1169 = CARTESIAN_POINT ( 'NONE',  ( 37.87673106522297672, -285.8690075228681735, -257.4429778579698791 ) ) ;
#1170 = CARTESIAN_POINT ( 'NONE',  ( -29.33785757386130300, -284.5493500736085366, -343.7768735603187906 ) ) ;
#1171 = CARTESIAN_POINT ( 'NONE',  ( -110.5216977149730013, -282.5322082173488525, -290.8223488412324969 ) ) ;
#1172 = CARTESIAN_POINT ( 'NONE',  ( -10.74601416509237595, -284.1237968329435830, -339.0303281633322285 ) ) ;
#1173 = CARTESIAN_POINT ( 'NONE',  ( -93.53955684783119295, -284.6917313239906662, -317.2055693889384997 ) ) ;
#1174 = CARTESIAN_POINT ( 'NONE',  ( -103.6954691459158511, -292.0601716343610406, -306.0764387449386845 ) ) ;
#1175 = CARTESIAN_POINT ( 'NONE',  ( -52.54560006425432306, -274.1959337515751827, -194.8442124253568863 ) ) ;
#1176 = VERTEX_POINT ( 'NONE', #23212 ) ;
#1177 = CARTESIAN_POINT ( 'NONE',  ( 21.27231673997742334, -286.2841671170784821, -318.0649201518546647 ) ) ;
#1178 = CARTESIAN_POINT ( 'NONE',  ( 38.18236941731774436, -275.7397957691224519, -285.3649481369480441 ) ) ;
#1179 = CARTESIAN_POINT ( 'NONE',  ( 36.92927584952963116, -295.4293685446331779, -262.4020301294230535 ) ) ;
#1180 = CARTESIAN_POINT ( 'NONE',  ( 169.8384340989974532, 214.5000000000000568, -24.41176470588233727 ) ) ;
#1181 = CARTESIAN_POINT ( 'NONE',  ( 21.31550574532285580, -290.6948066931273615, -317.0979686699210447 ) ) ;
#1182 = CARTESIAN_POINT ( 'NONE',  ( -53.81639815550146722, -281.9527292216469618, -342.0363733493801988 ) ) ;
#1183 = CARTESIAN_POINT ( 'NONE',  ( -59.15783564601671429, -275.3337007900643130, -342.2922284652613030 ) ) ;
#1184 = CARTESIAN_POINT ( 'NONE',  ( -60.64083731168902602, -272.2352900528970281, -197.6433630077483201 ) ) ;
#1185 = CARTESIAN_POINT ( 'NONE',  ( 13.79671641445455244, -275.6608157164388899, -322.6690945520528544 ) ) ;
#1186 = CARTESIAN_POINT ( 'NONE',  ( -9.483153472013412966, -293.9429381436158906, -202.0821335701165538 ) ) ;
#1187 = CARTESIAN_POINT ( 'NONE',  ( 20.36089909560774558, -293.8595240299239322, -225.2429429730586889 ) ) ;
#1188 = CARTESIAN_POINT ( 'NONE',  ( -98.20179095344455789, -286.8913032155658129, -228.2195495346648499 ) ) ;
#1189 = CARTESIAN_POINT ( 'NONE',  ( 38.23643522871735456, -295.1191964814565267, -281.6106401458225719 ) ) ;
#1190 = CARTESIAN_POINT ( 'NONE',  ( 37.30647844064418450, -295.0790415012825179, -287.1818011770321846 ) ) ;
#1191 = CARTESIAN_POINT ( 'NONE',  ( -108.2995173750590823, -296.1585910187631612, -287.5599210686464744 ) ) ;
#1192 = CARTESIAN_POINT ( 'NONE',  ( -99.76145633253106837, -291.9902192124415592, -311.9630231620489553 ) ) ;
#1193 = CARTESIAN_POINT ( 'NONE',  ( -33.05662495295239012, -283.1662888241863811, -347.2549276083731797 ) ) ;
#1194 = CARTESIAN_POINT ( 'NONE',  ( -36.53468314664176830, -296.1420315690264715, -194.8013716169795941 ) ) ;
#1195 = CARTESIAN_POINT ( 'NONE',  ( -87.74833893996564882, -285.2041782759736748, -212.0825361959433906 ) ) ;
#1196 = CARTESIAN_POINT ( 'NONE',  ( -41.93312153859111646, -279.0901634900727117, -344.8774589337492671 ) ) ;
#1197 = ADVANCED_FACE ( 'NONE', ( #88535 ), #31719, .T. ) ;
#1198 = CARTESIAN_POINT ( 'NONE',  ( -101.3300127581286461, -283.8376077873674603, -234.3038855303090315 ) ) ;
#1199 = CARTESIAN_POINT ( 'NONE',  ( 35.55434084484616619, -285.7791524868341071, -288.0552444707524273 ) ) ;
#1200 = CARTESIAN_POINT ( 'NONE',  ( -95.84822795775885140, -277.3491536565922502, -222.2026946770242262 ) ) ;
#1201 = CARTESIAN_POINT ( 'NONE',  ( -90.99921415893403775, -226.8295888252787904, -341.9546587472784154 ) ) ;
#1202 = CARTESIAN_POINT ( 'NONE',  ( -97.40295851047305575, -284.6391784208976219, -228.7381206260400290 ) ) ;
#1203 = CARTESIAN_POINT ( 'NONE',  ( 32.80316486822700739, -282.3625786447462929, -239.5762737867115959 ) ) ;
#1204 = CARTESIAN_POINT ( 'NONE',  ( -71.81158898197851670, -288.5553575073413413, -338.9515471713892794 ) ) ;
#1205 = CARTESIAN_POINT ( 'NONE',  ( 16.40555481139226046, -277.9045635920165864, -324.4503068328998552 ) ) ;
#1206 = CARTESIAN_POINT ( 'NONE',  ( -37.11152475351090629, -278.3644594539755417, -346.8805982259588632 ) ) ;
#1207 = CARTESIAN_POINT ( 'NONE',  ( -46.45435341712889254, -279.7667479160460857, -197.8810193087713856 ) ) ;
#1208 = CARTESIAN_POINT ( 'NONE',  ( -10.93134026860996499, -276.3779266610945342, -200.4893906446764618 ) ) ;
#1209 = CARTESIAN_POINT ( 'NONE',  ( 6.496230378298051278, -292.6300419999305973, -207.0583862175101615 ) ) ;
#1210 = CARTESIAN_POINT ( 'NONE',  ( 13.25253470048357052, -286.3611021679851660, -325.3136617449595747 ) ) ;
#1211 = CARTESIAN_POINT ( 'NONE',  ( 12.73723067749040716, -294.3374027913102964, -212.9281909900552705 ) ) ;
#1212 = CARTESIAN_POINT ( 'NONE',  ( -6.647956837599817703, -293.5597064423145639, -336.9352886300005707 ) ) ;
#1213 = CARTESIAN_POINT ( 'NONE',  ( -41.04453566529495845, -294.7667164892986307, -343.3008888633975744 ) ) ;
#1214 = CARTESIAN_POINT ( 'NONE',  ( -111.9587277084514909, -291.4086792588819321, -288.1314329022340530 ) ) ;
#1215 = CARTESIAN_POINT ( 'NONE',  ( 0.4455469819851471946, -281.2211471695746923, -207.7244407954254370 ) ) ;
#1216 = CARTESIAN_POINT ( 'NONE',  ( -71.28793332262237925, -272.6736272856959999, -201.5100216516559613 ) ) ;
#1217 = CARTESIAN_POINT ( 'NONE',  ( 28.82027028128720403, -288.7148236305812361, -309.5517604615333767 ) ) ;
#1218 = CARTESIAN_POINT ( 'NONE',  ( 8.443234154030673011, -280.5722833566217105, -330.7270460431906827 ) ) ;
#1219 = EDGE_CURVE ( 'NONE', #20475, #31737, #23684, .T. ) ;
#1220 = CARTESIAN_POINT ( 'NONE',  ( -80.52524142950187525, -289.9531053261362104, -334.1509059850862400 ) ) ;
#1222 = CARTESIAN_POINT ( 'NONE',  ( -27.83800129034970894, -286.5094488523340601, -197.9610682924675871 ) ) ;
#1221 = VECTOR ( 'NONE', #34164, 1000.000000000000000 ) ;
#1223 = FACE_OUTER_BOUND ( 'NONE', #24496, .T. ) ;
#1224 = CARTESIAN_POINT ( 'NONE',  ( 137.1683788224899274, 180.3412242032398467, -239.8556167576348912 ) ) ;
#1225 = CARTESIAN_POINT ( 'NONE',  ( 102.7605738203126577, 114.6418858672116414, -279.4648970305247531 ) ) ;
#1226 = CARTESIAN_POINT ( 'NONE',  ( -109.2038207892207282, -277.5677594924471805, -284.1546075097517132 ) ) ;
#1227 = CARTESIAN_POINT ( 'NONE',  ( -85.31787691779859983, -276.6535200397928520, -325.8586223164987814 ) ) ;
#1228 = CARTESIAN_POINT ( 'NONE',  ( -66.21535069744108171, -273.3511189256474836, -198.9883044232203702 ) ) ;
#1229 = CARTESIAN_POINT ( 'NONE',  ( -92.67010577559203455, -240.0894200528963154, -339.5335687754159153 ) ) ;
#1230 = CARTESIAN_POINT ( 'NONE',  ( -77.16977791118213759, -278.1044712878600080, -205.0899764529922038 ) ) ;
#1231 = CARTESIAN_POINT ( 'NONE',  ( -44.67521729214921322, -296.9037517187510957, -346.0457820422524264 ) ) ;
#1232 = CARTESIAN_POINT ( 'NONE',  ( -41.60269001370426878, -292.4895289931519642, -197.3740484606091172 ) ) ;
#1233 = CARTESIAN_POINT ( 'NONE',  ( -99.38399009088003311, -274.0962103606051414, -225.0670462314396048 ) ) ;
#1234 = CARTESIAN_POINT ( 'NONE',  ( 12.47787929332878498, -287.0257133110566201, -324.4603671640349489 ) ) ;
#1235 = CARTESIAN_POINT ( 'NONE',  ( -66.19667825136785666, -274.3356543446176943, -199.0679154175945484 ) ) ;
#1236 = CARTESIAN_POINT ( 'NONE',  ( -69.25945243168244758, -297.7867702038719244, -204.7085697271741083 ) ) ;
#1237 = ORIENTED_EDGE ( 'NONE', *, *, #74557, .F. ) ;
#1238 = PLANE ( 'NONE',  #55318 ) ;
#1239 = CARTESIAN_POINT ( 'NONE',  ( -95.72076983864123179, -281.1291109105193868, -222.3701828786022077 ) ) ;
#1240 = EDGE_CURVE ( 'NONE', #8882, #83322, #52548, .T. ) ;
#1241 = CARTESIAN_POINT ( 'NONE',  ( -94.18890406394115189, -280.2842494856001849, -224.0726585210119310 ) ) ;
#1242 = CARTESIAN_POINT ( 'NONE',  ( -110.8414872854830833, -280.0671331399246924, -289.6931427410897868 ) ) ;
#1243 = CARTESIAN_POINT ( 'NONE',  ( -21.76881556398774720, -272.7352590174109537, -198.3320056955437281 ) ) ;
#1244 = CARTESIAN_POINT ( 'NONE',  ( 209.0514133012270861, 29.56734752687822620, 14.78224109794551033 ) ) ;
#1245 = CARTESIAN_POINT ( 'NONE',  ( -147.0026986695710320, 31.65052214425349675, 21.50000000000000000 ) ) ;
#1246 = CARTESIAN_POINT ( 'NONE',  ( -79.05660610622193474, -279.6384712174848346, -210.4539679608586482 ) ) ;
#1247 = CARTESIAN_POINT ( 'NONE',  ( 22.62589851958319898, -275.7098621028263778, -222.2981301742025266 ) ) ;
#1248 = CARTESIAN_POINT ( 'NONE',  ( 36.76375887619934701, -277.7047962690376721, -282.2368622495716863 ) ) ;
#1249 = CARTESIAN_POINT ( 'NONE',  ( -86.72829848125643082, -276.2976626089749175, -328.7361955000521334 ) ) ;
#1250 = ORIENTED_EDGE ( 'NONE', *, *, #18442, .F. ) ;
#1251 = CARTESIAN_POINT ( 'NONE',  ( 152.4536156746142410, 250.0000000000000568, -11.99999999999999112 ) ) ;
#1252 = CARTESIAN_POINT ( 'NONE',  ( -24.78235124978375481, -284.8727238771388102, -344.7152890780492953 ) ) ;
#1253 = CARTESIAN_POINT ( 'NONE',  ( -88.03512400441982777, -290.5182726999854594, -217.5390677845554990 ) ) ;
#1254 = EDGE_CURVE ( 'NONE', #75524, #47701, #79849, .T. ) ;
#1255 = CARTESIAN_POINT ( 'NONE',  ( 14.18474048092872941, -286.1018353062679580, -213.2078114396948081 ) ) ;
#1256 = CARTESIAN_POINT ( 'NONE',  ( -51.22971925187731301, -281.4718253673992194, -343.1120849470090661 ) ) ;
#1257 = CARTESIAN_POINT ( 'NONE',  ( -53.83927818999645609, -281.8426486551438757, -342.1297666177063093 ) ) ;
#1258 = CARTESIAN_POINT ( 'NONE',  ( 24.00602563254055610, -282.2005001400641504, -229.9757303430876050 ) ) ;
#1259 = CARTESIAN_POINT ( 'NONE',  ( 193.6317247519612863, 279.2590634987193994, -125.8091550203929216 ) ) ;
#1260 = CARTESIAN_POINT ( 'NONE',  ( -47.17353373968273900, -281.5749530826011551, -345.9241741808497181 ) ) ;
#1261 = CARTESIAN_POINT ( 'NONE',  ( 31.47881924792857333, -295.1622739691200650, -240.5494296925795652 ) ) ;
#1262 = CARTESIAN_POINT ( 'NONE',  ( -97.72836163025088752, -278.6311702047453878, -311.5599502583124831 ) ) ;
#1263 = CARTESIAN_POINT ( 'NONE',  ( -72.77193442836117754, -287.5845644209379657, -204.0107249021278619 ) ) ;
#1264 = CARTESIAN_POINT ( 'NONE',  ( 196.7806748523260012, 250.5000000000000568, -12.67104836398113399 ) ) ;
#1265 = CARTESIAN_POINT ( 'NONE',  ( -83.40815675873707846, -293.3468823295299899, -210.4019555419367862 ) ) ;
#1266 = CARTESIAN_POINT ( 'NONE',  ( 28.51095958071148573, -274.0301895446212370, -306.3642975492415985 ) ) ;
#1267 = CARTESIAN_POINT ( 'NONE',  ( -20.54168934993978013, -288.0390185172796009, -345.3951224932175137 ) ) ;
#1268 = CARTESIAN_POINT ( 'NONE',  ( -27.98494059256432465, -290.5726294592739123, -197.1053629635317179 ) ) ;
#1269 = CARTESIAN_POINT ( 'NONE',  ( -101.0184308945940046, -276.7360075648400652, -307.1582907912126643 ) ) ;
#1270 = CARTESIAN_POINT ( 'NONE',  ( -103.6247257536396802, -295.1392584653447670, -236.8188105767752916 ) ) ;
#1271 = CARTESIAN_POINT ( 'NONE',  ( -96.15295369221790622, -291.2525545779229219, -314.4556879514004777 ) ) ;
#1272 = CARTESIAN_POINT ( 'NONE',  ( 193.9646936176702070, 21.00000000000000000, -15.00000000000000000 ) ) ;
#1273 = CARTESIAN_POINT ( 'NONE',  ( 175.2296996224749250, 250.5000000000000568, -24.99999999999999289 ) ) ;
#1274 = CARTESIAN_POINT ( 'NONE',  ( 12.92442427130810856, -292.8454988994985797, -327.8421735475841956 ) ) ;
#1275 = CARTESIAN_POINT ( 'NONE',  ( -5.471426269818340238, -288.0786184467141311, -203.7834850905255166 ) ) ;
#1276 = CARTESIAN_POINT ( 'NONE',  ( -112.9956661257817387, -288.8888957890508209, -262.7163230750809930 ) ) ;
#1277 = CARTESIAN_POINT ( 'NONE',  ( 35.10493895194819913, -289.1464659952534930, -283.2785250020855869 ) ) ;
#1278 = CARTESIAN_POINT ( 'NONE',  ( -113.5000000000000568, -218.8335761803644743, -447.4016117689005796 ) ) ;
#1279 = CARTESIAN_POINT ( 'NONE',  ( -23.74516055091860878, -289.6769305378810486, -342.2998982507519941 ) ) ;
#1280 = LINE ( 'NONE', #2221, #36777 ) ;
#1281 = AXIS2_PLACEMENT_3D ( 'NONE', #34817, #63730, #27726 ) ;
#1282 = CARTESIAN_POINT ( 'NONE',  ( -20.56832576917869915, -290.0466037300154198, -345.1594865736184943 ) ) ;
#1283 = CARTESIAN_POINT ( 'NONE',  ( -58.80892421910212420, -277.7959193459898302, -198.1284031630851814 ) ) ;
#1284 = CARTESIAN_POINT ( 'NONE',  ( -109.5878191296876594, -279.2231289540560510, -243.6319765235116961 ) ) ;
#1285 = CARTESIAN_POINT ( 'NONE',  ( -36.74845336231327764, -279.7261383661606828, -193.3715058316192312 ) ) ;
#1286 = CARTESIAN_POINT ( 'NONE',  ( -60.57463744152092033, -283.7506191264303652, -199.0503104512943935 ) ) ;
#1287 = CARTESIAN_POINT ( 'NONE',  ( 196.5738014817347050, 41.11195847892590649, 11.18394375856346556 ) ) ;
#1288 = CARTESIAN_POINT ( 'NONE',  ( -36.97890755337682833, -278.1963271922607532, -196.1268006791808034 ) ) ;
#1289 = CARTESIAN_POINT ( 'NONE',  ( -2.584223713412890255, -280.5922660126767596, -336.8210193129521031 ) ) ;
#1290 = FACE_OUTER_BOUND ( 'NONE', #52683, .T. ) ;
#1291 = CARTESIAN_POINT ( 'NONE',  ( -103.0189976239582990, -276.5201896994689719, -309.3132081572083507 ) ) ;
#1292 = CARTESIAN_POINT ( 'NONE',  ( -70.79946912355336508, -299.1226755514359752, -204.6866931959504257 ) ) ;
#1293 = CARTESIAN_POINT ( 'NONE',  ( -109.0189814984703673, -283.1241916530127583, -297.7829623172737570 ) ) ;
#1294 = CARTESIAN_POINT ( 'NONE',  ( -46.20846488888262371, -274.7396264861915824, -197.7389298480991329 ) ) ;
#1295 = CARTESIAN_POINT ( 'NONE',  ( -92.75743588560285957, -274.7020742062829868, -217.7330602485023121 ) ) ;
#1296 = CARTESIAN_POINT ( 'NONE',  ( 7.590064494120423610, -276.0865560307798887, -327.9861570643587356 ) ) ;
#1297 = CARTESIAN_POINT ( 'NONE',  ( -34.19239939503944470, -297.0126997558913899, -345.2949725208078462 ) ) ;
#1298 = CARTESIAN_POINT ( 'NONE',  ( -75.66183911080170787, -289.7155964329720632, -337.1485940005564999 ) ) ;
#1299 = CARTESIAN_POINT ( 'NONE',  ( -70.57872091346399657, -277.6971733661320627, -202.5038070151277054 ) ) ;
#1300 = CARTESIAN_POINT ( 'NONE',  ( -102.3024015441570782, -289.8424642856674609, -311.8005918935049294 ) ) ;
#1301 = CARTESIAN_POINT ( 'NONE',  ( -61.34340426095521082, -288.4304225641278094, -339.5516277842015143 ) ) ;
#1302 = CARTESIAN_POINT ( 'NONE',  ( -1.730437127795238172, -290.5239215406219273, -204.3547652704849895 ) ) ;
#1303 = ORIENTED_EDGE ( 'NONE', *, *, #24438, .F. ) ;
#1304 = FACE_BOUND ( 'NONE', #58441, .T. ) ;
#1305 = CARTESIAN_POINT ( 'NONE',  ( -94.15609292284101173, -289.4106324383022297, -316.2970866045370713 ) ) ;
#1306 = DIRECTION ( 'NONE',  ( 0.000000000000000000, 0.000000000000000000, 1.000000000000000000 ) ) ;
#1307 = CARTESIAN_POINT ( 'NONE',  ( -32.33377699988042053, -287.0550684935378172, -193.7468109722198619 ) ) ;
#1308 = CARTESIAN_POINT ( 'NONE',  ( -92.08974858914540107, -287.6948066931273047, -226.7417163044926838 ) ) ;
#1309 = CARTESIAN_POINT ( 'NONE',  ( 33.19561060100984662, -292.9993756964033764, -300.7824051068001268 ) ) ;
#1310 = CARTESIAN_POINT ( 'NONE',  ( 24.71714679701682016, -283.4646391430484869, -315.1270526228138351 ) ) ;
#1311 = CARTESIAN_POINT ( 'NONE',  ( -93.25373315542717023, -285.0519866982648409, -223.4266469907795454 ) ) ;
#1312 = CARTESIAN_POINT ( 'NONE',  ( 15.79182080314342862, -276.1390977356639951, -219.5127464327528060 ) ) ;
#1313 = CARTESIAN_POINT ( 'NONE',  ( 35.93431208748905448, -291.7558319500407720, -284.5904130878255955 ) ) ;
#1314 = CARTESIAN_POINT ( 'NONE',  ( 33.89827047411661454, -274.1152497349642090, -252.6976784929620976 ) ) ;
#1315 = VERTEX_POINT ( 'NONE', #89447 ) ;
#1316 = LINE ( 'NONE', #58628, #74329 ) ;
#1317 = CARTESIAN_POINT ( 'NONE',  ( -8.399926009726220499, -294.3503289677409498, -341.7486276080564380 ) ) ;
#1318 = CARTESIAN_POINT ( 'NONE',  ( 16.04554392009131902, -288.7367144869345452, -218.4851469519760201 ) ) ;
#1319 = CARTESIAN_POINT ( 'NONE',  ( -89.40857248324721240, -298.4192051437676696, -213.9816785797699197 ) ) ;
#1320 = CARTESIAN_POINT ( 'NONE',  ( 18.73462360188017328, -287.5386252663560072, -223.4445128708985919 ) ) ;
#1321 = CARTESIAN_POINT ( 'NONE',  ( -108.2906088729402256, -277.9845747191277496, -241.0511783668453063 ) ) ;
#1322 = CARTESIAN_POINT ( 'NONE',  ( -32.01128333207816468, -295.6380054311364347, -347.0874532399008103 ) ) ;
#1323 = CARTESIAN_POINT ( 'NONE',  ( 21.43170968467204318, -286.3438955711848166, -318.1935738807069924 ) ) ;
#1324 = CARTESIAN_POINT ( 'NONE',  ( 34.43330939936353019, -294.2380094333950069, -298.1836322253800518 ) ) ;
#1325 = CARTESIAN_POINT ( 'NONE',  ( -69.03061536482888982, -291.9568873796781645, -204.5605326833156710 ) ) ;
#1326 = CARTESIAN_POINT ( 'NONE',  ( 152.4536156746142410, 275.0000000000000568, -11.50000000000000355 ) ) ;
#1327 = DIRECTION ( 'NONE',  ( 0.000000000000000000, 0.000000000000000000, -1.000000000000000000 ) ) ;
#1328 = CARTESIAN_POINT ( 'NONE',  ( -54.76359932917087292, -169.9329552034514279, -360.8268486737608214 ) ) ;
#1329 = CARTESIAN_POINT ( 'NONE',  ( -36.59186565410484349, -287.5815181310400135, -194.0452119181639148 ) ) ;
#1330 = CARTESIAN_POINT ( 'NONE',  ( -88.52914483777347243, -281.1952119285918457, -334.4957818155094174 ) ) ;
#1331 = EDGE_LOOP ( 'NONE', ( #25766, #6601, #5992, #88463 ) ) ;
#1332 = CARTESIAN_POINT ( 'NONE',  ( -100.1609200747649027, -278.4883935519898728, -226.0095859684839468 ) ) ;
#1333 = CARTESIAN_POINT ( 'NONE',  ( 20.23064365918139274, -282.8906745597048484, -222.5348204226079361 ) ) ;
#1334 = CARTESIAN_POINT ( 'NONE',  ( 155.5532833854414605, 205.0543101207102552, -216.1346246433878662 ) ) ;
#1335 = CARTESIAN_POINT ( 'NONE',  ( -98.85897664030493104, -283.7346967105872295, -224.9504601315421155 ) ) ;
#1336 = CARTESIAN_POINT ( 'NONE',  ( 24.69633640067911173, -286.1921374569451473, -311.5255637593836013 ) ) ;
#1337 = CARTESIAN_POINT ( 'NONE',  ( 23.47400430328696430, -276.8019297325512298, -225.1753284315388441 ) ) ;
#1338 = CARTESIAN_POINT ( 'NONE',  ( -88.17305750314029922, -297.8096883478827408, -217.8103719788934995 ) ) ;
#1339 = CARTESIAN_POINT ( 'NONE',  ( 29.93481593136025509, -292.6322940907930956, -299.9434414810605176 ) ) ;
#1340 = CARTESIAN_POINT ( 'NONE',  ( -111.9889758563177651, -279.4355265076290493, -251.8382576489704547 ) ) ;
#1341 = CARTESIAN_POINT ( 'NONE',  ( -21.65302150415941185, -276.8455267778230109, -341.7073272721959256 ) ) ;
#1342 = CARTESIAN_POINT ( 'NONE',  ( -36.55569576436343482, -299.0030139488621899, -193.5962881258471100 ) ) ;
#1343 = CARTESIAN_POINT ( 'NONE',  ( 0.8809921019165840583, -275.4753837376584897, -336.9083267520210825 ) ) ;
#1344 = LINE ( 'NONE', #84136, #2329 ) ;
#1345 = CARTESIAN_POINT ( 'NONE',  ( 20.43381909603769131, -274.2126301869488998, -318.2629804891827803 ) ) ;
#1346 = CARTESIAN_POINT ( 'NONE',  ( -111.0190159084740742, -297.7217385083195040, -290.6159799495050038 ) ) ;
#1347 = DIRECTION ( 'NONE',  ( 0.000000000000000000, 1.000000000000000000, 0.000000000000000000 ) ) ;
#1348 = VECTOR ( 'NONE', #50781, 1000.000000000000000 ) ;
#1349 = DIRECTION ( 'NONE',  ( 0.000000000000000000, 0.000000000000000000, -1.000000000000000000 ) ) ;
#1350 = CARTESIAN_POINT ( 'NONE',  ( -81.67639484432494612, -286.5118216850802355, -211.9773795181534410 ) ) ;
#1351 = CARTESIAN_POINT ( 'NONE',  ( -73.77021608239635952, -285.2887063867223105, -337.1051792772611293 ) ) ;
#1352 = CARTESIAN_POINT ( 'NONE',  ( -17.13575233439146572, -285.6684329036442591, -200.0542813169454632 ) ) ;
#1353 = CARTESIAN_POINT ( 'NONE',  ( -105.0130160142174276, -276.5588928881783204, -299.9346840640773166 ) ) ;
#1354 = CARTESIAN_POINT ( 'NONE',  ( -111.5446812273848707, -286.4409455841696968, -268.1740940822559196 ) ) ;
#1355 = CARTESIAN_POINT ( 'NONE',  ( -19.34668950920417529, -278.7676106982231090, -198.8458383650429653 ) ) ;
#1356 = CARTESIAN_POINT ( 'NONE',  ( 32.39645809962343037, -276.9304153606940986, -292.9623427422388886 ) ) ;
#1357 = CARTESIAN_POINT ( 'NONE',  ( -26.41588298435790350, -486.4924983417995463, -430.6442049081568939 ) ) ;
#1358 = CARTESIAN_POINT ( 'NONE',  ( 94.63317399270954411, -300.3986776538885124, -197.2442351111135963 ) ) ;
#1359 = CARTESIAN_POINT ( 'NONE',  ( 29.62619520685872487, -282.8460436223892884, -308.1453017321348398 ) ) ;
#1360 = CARTESIAN_POINT ( 'NONE',  ( -0.3994739115543821106, -283.0669260933392479, -337.8652953817621665 ) ) ;
#1361 = ORIENTED_EDGE ( 'NONE', *, *, #30936, .F. ) ;
#1362 = EDGE_LOOP ( 'NONE', ( #389, #48035 ) ) ;
#1363 = DIRECTION ( 'NONE',  ( -0.000000000000000000, -1.000000000000000000, -0.000000000000000000 ) ) ;
#1364 = CARTESIAN_POINT ( 'NONE',  ( 36.51020841098728908, -289.1968773317620958, -253.3861411473637304 ) ) ;
#1365 = CARTESIAN_POINT ( 'NONE',  ( -113.6222243893442254, -289.1547419823139649, -276.8947000431542165 ) ) ;
#1366 = CARTESIAN_POINT ( 'NONE',  ( -107.0262058871500415, -295.4524755518525581, -292.8113214809180818 ) ) ;
#1367 = EDGE_CURVE ( 'NONE', #81908, #50747, #52092, .T. ) ;
#1368 = CARTESIAN_POINT ( 'NONE',  ( -22.20572272908044553, -291.5895758068863870, -194.9131297881342277 ) ) ;
#1369 = CARTESIAN_POINT ( 'NONE',  ( 10.55130591562493869, -286.8567396987317011, -326.4372153599002218 ) ) ;
#1370 = CARTESIAN_POINT ( 'NONE',  ( -37.28564521386969233, -287.6261629888885523, -343.9503276333391000 ) ) ;
#1371 = CARTESIAN_POINT ( 'NONE',  ( -41.35992835435267523, -287.2055487697227250, -197.0615519117667418 ) ) ;
#1372 = CARTESIAN_POINT ( 'NONE',  ( -110.2374995252888681, -276.3247971859484551, -288.0559321959354975 ) ) ;
#1373 = CARTESIAN_POINT ( 'NONE',  ( -29.16912478323997959, -290.9488840426138836, -344.9666562665581750 ) ) ;
#1374 = CARTESIAN_POINT ( 'NONE',  ( -37.52335318451943635, -287.0542291568665405, -345.5403296610969051 ) ) ;
#1375 = CARTESIAN_POINT ( 'NONE',  ( -110.4639598478855333, -285.5578378642339317, -265.4613663405748412 ) ) ;
#1376 = CARTESIAN_POINT ( 'NONE',  ( -110.1399438166561708, -292.3117252194971911, -289.1326928361215778 ) ) ;
#1377 = CARTESIAN_POINT ( 'NONE',  ( 82.13662659784047548, -300.5150969315919838, -193.6047415040562498 ) ) ;
#1378 = CARTESIAN_POINT ( 'NONE',  ( 156.4947056272798136, 19.99999999999999645, -15.00000000000000711 ) ) ;
#1379 = CARTESIAN_POINT ( 'NONE',  ( -112.1790098971907668, -298.6063709220446754, -259.8417975139061014 ) ) ;
#1380 = CARTESIAN_POINT ( 'NONE',  ( -9.175753616059115103, -279.6272733076894497, -202.8386684985784143 ) ) ;
#1381 = CARTESIAN_POINT ( 'NONE',  ( 36.02688869273971051, -279.3514737429551928, -254.7418426853482742 ) ) ;
#1382 = CARTESIAN_POINT ( 'NONE',  ( 39.06670442241018293, -292.6414538926898672, -261.7541836717572323 ) ) ;
#1383 = CARTESIAN_POINT ( 'NONE',  ( -94.54750324048427501, -271.4483917101229054, -223.3788747945172588 ) ) ;
#1384 = CARTESIAN_POINT ( 'NONE',  ( 10.57262087529013073, -274.4640251165277505, -327.3306891391998192 ) ) ;
#1385 = CARTESIAN_POINT ( 'NONE',  ( -108.7744014947930111, -297.6402048737558061, -287.6945511815222289 ) ) ;
#1386 = CARTESIAN_POINT ( 'NONE',  ( 204.7786681169002350, 32.98517505407394168, 10.00000000000000000 ) ) ;
#1387 = CARTESIAN_POINT ( 'NONE',  ( -91.98409470737627203, -294.0590528655447997, -323.1643634114109318 ) ) ;
#1388 = CARTESIAN_POINT ( 'NONE',  ( 16.60333062456019704, -295.6910400073747383, -320.4141755769032329 ) ) ;
#1389 = DIRECTION ( 'NONE',  ( 0.000000000000000000, 0.000000000000000000, 1.000000000000000000 ) ) ;
#1390 = CARTESIAN_POINT ( 'NONE',  ( -69.78650493502040320, -296.2935837162376629, -335.9350180386305169 ) ) ;
#1391 = CARTESIAN_POINT ( 'NONE',  ( 125.9462722777150958, 8.500086813760361792, 22.50000000000000000 ) ) ;
#1393 = CARTESIAN_POINT ( 'NONE',  ( -108.8847233520359197, -296.3598946323040764, -284.9352898441010211 ) ) ;
#1392 = CARTESIAN_POINT ( 'NONE',  ( -66.52821591130842194, -283.6919026314164967, -200.8877122727009237 ) ) ;
#1394 = CARTESIAN_POINT ( 'NONE',  ( -114.3407659224605766, -284.5568958099508450, -269.9818202197658934 ) ) ;
#1395 = CARTESIAN_POINT ( 'NONE',  ( 37.84780553902246680, -283.5740164944031676, -278.3416710924523159 ) ) ;
#1396 = CARTESIAN_POINT ( 'NONE',  ( -65.86558042004320157, -285.3557758935428978, -198.8477890740071246 ) ) ;
#1397 = CARTESIAN_POINT ( 'NONE',  ( 35.74574881223696110, -291.3444308111306214, -254.2315161905954142 ) ) ;
#1398 = CARTESIAN_POINT ( 'NONE',  ( -112.0780845840028945, -277.6733258455329292, -288.5211455284123758 ) ) ;
#1399 = CARTESIAN_POINT ( 'NONE',  ( -37.37352853689063181, -280.5523547857346784, -345.3611179825600175 ) ) ;
#1400 = CARTESIAN_POINT ( 'NONE',  ( -48.18343439339133027, -283.1093320178188151, -502.6442049081569508 ) ) ;
#1401 = CARTESIAN_POINT ( 'NONE',  ( 32.65688275607818269, -286.0555277732573813, -248.2434858962869839 ) ) ;
#1402 = CARTESIAN_POINT ( 'NONE',  ( -46.00456630510468869, -288.0797573760335695, -346.6140794719176483 ) ) ;
#1403 = CARTESIAN_POINT ( 'NONE',  ( 197.8477145984406889, 64.61450673763175701, -7.741079165001063522 ) ) ;
#1404 = CARTESIAN_POINT ( 'NONE',  ( -104.4493723474346751, -279.5009052287889517, -306.9010498480661226 ) ) ;
#1406 = CARTESIAN_POINT ( 'NONE',  ( 29.33203249001316593, -281.6212203201883426, -300.2627754168768206 ) ) ;
#1405 = CARTESIAN_POINT ( 'NONE',  ( 18.29781725470346032, -292.2790196284022386, -321.2568800984311679 ) ) ;
#1407 = CARTESIAN_POINT ( 'NONE',  ( 37.78439455871049546, -293.9307334786635124, -287.3046512182173160 ) ) ;
#1408 = CARTESIAN_POINT ( 'NONE',  ( 25.17985865037724125, -285.0616745523148552, -227.9072402999705389 ) ) ;
#1409 = CARTESIAN_POINT ( 'NONE',  ( -47.86405180145010974, -281.9186281289387352, -196.0504666327389600 ) ) ;
#1411 = CARTESIAN_POINT ( 'NONE',  ( -80.30245814932901283, -294.7091538289109849, -329.6720083629043643 ) ) ;
#1410 = VECTOR ( 'NONE', #49510, 1000.000000000000000 ) ;
#1412 = CARTESIAN_POINT ( 'NONE',  ( -108.3611493555414995, -270.8699978521538583, -245.7386433506795527 ) ) ;
#1413 = ORIENTED_EDGE ( 'NONE', *, *, #64946, .T. ) ;
#1414 = DIRECTION ( 'NONE',  ( 0.000000000000000000, 0.000000000000000000, 1.000000000000000000 ) ) ;
#1415 = CARTESIAN_POINT ( 'NONE',  ( 33.80659575920257254, -283.8267560256765023, -293.1076588587019387 ) ) ;
#1416 = CARTESIAN_POINT ( 'NONE',  ( -61.03904947665057534, -294.8757426141323776, -339.5264176675144085 ) ) ;
#1417 = DIRECTION ( 'NONE',  ( 0.000000000000000000, 1.000000000000000000, 0.000000000000000000 ) ) ;
#1418 = CARTESIAN_POINT ( 'NONE',  ( -106.6662871844225293, -281.6237833571634610, -303.7098442033569086 ) ) ;
#1419 = CARTESIAN_POINT ( 'NONE',  ( -71.32217281691825406, -272.8120242918620875, -201.4446011151220830 ) ) ;
#1420 = EDGE_CURVE ( 'NONE', #67590, #20083, #42046, .T. ) ;
#1421 = ADVANCED_FACE ( 'NONE', ( #16119 ), #24606, .F. ) ;
#1422 = CARTESIAN_POINT ( 'NONE',  ( -98.11185000843182991, -289.8237282426162551, -310.8312352110697248 ) ) ;
#1423 = CARTESIAN_POINT ( 'NONE',  ( -89.98227290016242819, -280.8123861596716893, -218.7167137960210539 ) ) ;
#1424 = CARTESIAN_POINT ( 'NONE',  ( -16.43331552015228425, -275.9268990689354837, -199.5315708164286832 ) ) ;
#1425 = CARTESIAN_POINT ( 'NONE',  ( -19.09005687647491101, -284.4213199808800141, -344.3973838385429644 ) ) ;
#1426 = CARTESIAN_POINT ( 'NONE',  ( -64.95132935486626025, -278.4781689442403376, -202.3549500325787278 ) ) ;
#1427 = CARTESIAN_POINT ( 'NONE',  ( -51.63783561217644547, -279.2352042517546806, -343.9859857652226651 ) ) ;
#1428 = ORIENTED_EDGE ( 'NONE', *, *, #14429, .F. ) ;
#1429 = CARTESIAN_POINT ( 'NONE',  ( -90.16131540396499133, -273.1635997788909549, -214.2607405942027867 ) ) ;
#1430 = CARTESIAN_POINT ( 'NONE',  ( -102.3937442989139015, -292.9587663097002519, -234.0675382806387574 ) ) ;
#1431 = DIRECTION ( 'NONE',  ( 0.000000000000000000, 0.000000000000000000, 1.000000000000000000 ) ) ;
#1432 = CYLINDRICAL_SURFACE ( 'NONE', #55768, 26.04691768583017364 ) ;
#1433 = CARTESIAN_POINT ( 'NONE',  ( -33.52120502682937797, -293.1441615915895795, -346.0424438696508105 ) ) ;
#1434 = CARTESIAN_POINT ( 'NONE',  ( 19.90763343179916589, -274.4194142080881988, -224.9483417611401421 ) ) ;
#1435 = CARTESIAN_POINT ( 'NONE',  ( -58.76276249475572655, -293.3000997861807377, -197.1228367477258132 ) ) ;
#1437 = CARTESIAN_POINT ( 'NONE',  ( -37.80809119427475196, -293.2515017321359778, -193.7596088598672850 ) ) ;
#1436 = CARTESIAN_POINT ( 'NONE',  ( 35.77081079830085031, -277.8376638359845288, -253.6410175316879361 ) ) ;
#1438 = CARTESIAN_POINT ( 'NONE',  ( 36.57399071147558089, -289.7037128773318386, -282.1262348526219057 ) ) ;
#1439 = CARTESIAN_POINT ( 'NONE',  ( 34.26340533266121469, -273.8333595633521327, -292.1480107064741674 ) ) ;
#1440 = CARTESIAN_POINT ( 'NONE',  ( 28.04306295079809885, -277.9498730916036493, -306.0518975365675374 ) ) ;
#1441 = CARTESIAN_POINT ( 'NONE',  ( -3.707476465593006143, -292.6847075651662067, -336.7836217841268081 ) ) ;
#1442 = CARTESIAN_POINT ( 'NONE',  ( -103.7229564553331613, -280.8932924034027110, -233.8394218753010989 ) ) ;
#1443 = VERTEX_POINT ( 'NONE', #82370 ) ;
#1444 = CARTESIAN_POINT ( 'NONE',  ( -26.74390006549232979, -282.5804926980131881, -342.6604363933534501 ) ) ;
#1445 = CARTESIAN_POINT ( 'NONE',  ( -53.70797439407711948, -280.9266823302423290, -195.3825539801070192 ) ) ;
#1446 = CARTESIAN_POINT ( 'NONE',  ( -24.61474080773121997, -281.6882686554803286, -345.9532429516009984 ) ) ;
#1447 = CARTESIAN_POINT ( 'NONE',  ( -95.02603804343112870, -278.8058644561330652, -321.0102776263897795 ) ) ;
#1448 = CARTESIAN_POINT ( 'NONE',  ( 23.91164583182238701, -276.4616907791411791, -224.8557846361411521 ) ) ;
#1449 = CARTESIAN_POINT ( 'NONE',  ( 30.89617123739170168, -289.8376638359844719, -254.7536222014695397 ) ) ;
#1450 = ORIENTED_EDGE ( 'NONE', *, *, #68389, .T. ) ;
#1451 = VERTEX_POINT ( 'NONE', #73871 ) ;
#1452 = CARTESIAN_POINT ( 'NONE',  ( -109.3874940036984640, -298.8206270639723243, -249.5187516343233654 ) ) ;
#1453 = CARTESIAN_POINT ( 'NONE',  ( -25.37210858833041982, -293.2878451266919342, -197.9840818391974722 ) ) ;
#1454 = CARTESIAN_POINT ( 'NONE',  ( -108.6962292960956091, -276.2863250136849729, -292.4519222031888148 ) ) ;
#1455 = CARTESIAN_POINT ( 'NONE',  ( -15.22547718514172388, -290.5299158293701680, -343.1130917346178535 ) ) ;
#1456 = CARTESIAN_POINT ( 'NONE',  ( -66.59726230471117958, -291.0070993842258531, -203.3685456317933244 ) ) ;
#1457 = CARTESIAN_POINT ( 'NONE',  ( 3.142418115635885911, -288.0318454059959095, -335.8496251866239390 ) ) ;
#1458 = DIRECTION ( 'NONE',  ( 0.000000000000000000, 1.000000000000000000, 0.000000000000000000 ) ) ;
#1459 = CARTESIAN_POINT ( 'NONE',  ( -111.1911077235709087, -282.9450498158478808, -270.8949704174044086 ) ) ;
#1460 = CARTESIAN_POINT ( 'NONE',  ( -110.6349106926464145, -292.2586127777328784, -282.2295021675640783 ) ) ;
#1461 = CARTESIAN_POINT ( 'NONE',  ( -108.4350998182151926, -282.7775506637423177, -289.8107735325176009 ) ) ;
#1462 = CARTESIAN_POINT ( 'NONE',  ( -9.073033251643639829, -281.7449377755394835, -202.5221472374239511 ) ) ;
#1463 = ORIENTED_EDGE ( 'NONE', *, *, #63505, .T. ) ;
#1464 = CARTESIAN_POINT ( 'NONE',  ( -97.96638673433362499, -290.8625750643865899, -317.4511125449042765 ) ) ;
#1465 = CARTESIAN_POINT ( 'NONE',  ( -89.52191759520569292, -279.7847770721391498, -219.1502558904300599 ) ) ;
#1466 = CARTESIAN_POINT ( 'NONE',  ( -44.84281161810447713, -290.7542629961829448, -194.0736863607303917 ) ) ;
#1467 = CARTESIAN_POINT ( 'NONE',  ( 21.95902065947467818, -287.6970775699344358, -221.4982145150968620 ) ) ;
#1468 = CARTESIAN_POINT ( 'NONE',  ( 7.903391843717010090, -288.9450214563344730, -332.6554997890902996 ) ) ;
#1469 = CARTESIAN_POINT ( 'NONE',  ( -72.37587749378877788, -285.7415138044681271, -206.3031160916555677 ) ) ;
#1470 = VERTEX_POINT ( 'NONE', #17520 ) ;
#1471 = DIRECTION ( 'NONE',  ( 0.000000000000000000, 0.000000000000000000, 1.000000000000000000 ) ) ;
#1472 = CARTESIAN_POINT ( 'NONE',  ( 19.43705777708717264, -294.7219535435830835, -220.1770140457471427 ) ) ;
#1473 = CARTESIAN_POINT ( 'NONE',  ( -22.21155743937168126, -293.5470792457638822, -345.3569648920415602 ) ) ;
#1474 = CARTESIAN_POINT ( 'NONE',  ( -61.87991936387788883, -276.4376941382475366, -339.4170950671252740 ) ) ;
#1475 = CARTESIAN_POINT ( 'NONE',  ( -54.56426064149214028, -297.1850267285084897, -195.4164971240218449 ) ) ;
#1476 = AXIS2_PLACEMENT_3D ( 'NONE', #8968, #1414, #22268 ) ;
#1477 = CARTESIAN_POINT ( 'NONE',  ( 19.35423114739423056, -292.6934918920479731, -317.4384918592071472 ) ) ;
#1478 = CARTESIAN_POINT ( 'NONE',  ( -111.2224919485975789, -294.8496100106004292, -265.9336343442270731 ) ) ;
#1479 = CARTESIAN_POINT ( 'NONE',  ( -79.77269421180812969, -292.6695535082092761, -210.4094046147227175 ) ) ;
#1480 = CARTESIAN_POINT ( 'NONE',  ( 12.57537448609780029, -295.4166087703552535, -324.1197342669860291 ) ) ;
#1481 = CARTESIAN_POINT ( 'NONE',  ( -43.53110651506508333, -249.2076723177077042, -456.5898888690692843 ) ) ;
#1482 = B_SPLINE_CURVE_WITH_KNOTS ( 'NONE', 3,
 ( #10660, #39516, #23489, #52356, #74608, #10190, #31066, #9737, #82632, #82167 ),
 .UNSPECIFIED., .F., .F.,
 ( 4, 2, 2, 2, 4 ),
 ( -1.872485596898890801E-05, 0.002374103250644057396, 0.004766931357257103534, 0.007159759463870149672, 0.009552587570483194943 ),
 .UNSPECIFIED. ) ;
#1483 = CARTESIAN_POINT ( 'NONE',  ( 24.97718621167626196, -292.1192734698619802, -312.3894992523332803 ) ) ;
#1484 = AXIS2_PLACEMENT_3D ( 'NONE', #68828, #19100, #3957 ) ;
#1485 = CARTESIAN_POINT ( 'NONE',  ( -100.9186871615504373, -299.0880780845530467, -230.4781179084328642 ) ) ;
#1486 = CARTESIAN_POINT ( 'NONE',  ( -107.6244744988845810, -291.7653974983800254, -249.7316160731506045 ) ) ;
#1487 = CARTESIAN_POINT ( 'NONE',  ( 8.244676534088640096, -294.7421266707629570, -327.4696829607519248 ) ) ;
#1488 = CARTESIAN_POINT ( 'NONE',  ( -96.42336048847371899, -281.1715587650895145, -223.5875761371995054 ) ) ;
#1489 = CARTESIAN_POINT ( 'NONE',  ( -95.51983067280377782, -277.9116797784892583, -220.6559596598636404 ) ) ;
#1490 = CARTESIAN_POINT ( 'NONE',  ( -111.7175489734729439, -272.1479081000331917, -250.6242070340624650 ) ) ;
#1491 = CARTESIAN_POINT ( 'NONE',  ( 35.04479773637792306, -279.8573300613501260, -287.7792932032427302 ) ) ;
#1492 = CARTESIAN_POINT ( 'NONE',  ( -94.34960562910202952, -277.6443057176829257, -219.7988877434916333 ) ) ;
#1493 = CARTESIAN_POINT ( 'NONE',  ( -107.8767749087758290, -276.8900631826272161, -244.2334650969371808 ) ) ;
#1494 = CARTESIAN_POINT ( 'NONE',  ( -33.76528826327452038, -296.7826661299722559, -196.8687839923029230 ) ) ;
#1495 = CARTESIAN_POINT ( 'NONE',  ( -102.6196903255425923, -275.0456344671761144, -233.3280175503710439 ) ) ;
#1496 = CARTESIAN_POINT ( 'NONE',  ( 194.3475392320528385, 26.68743749201679805, 14.50895590765962240 ) ) ;
#1497 = CARTESIAN_POINT ( 'NONE',  ( -110.3352241451626128, -288.3323161655783906, -289.1305061886560566 ) ) ;
#1498 = CARTESIAN_POINT ( 'NONE',  ( -109.8655511909556992, -290.2238299034394231, -296.3898506772237624 ) ) ;
#1499 = CARTESIAN_POINT ( 'NONE',  ( 10.59640682969090797, -276.7123369522162761, -212.3973327032843486 ) ) ;
#1500 = CARTESIAN_POINT ( 'NONE',  ( -102.4414457841392334, -271.0499318755020113, -233.0139747473175476 ) ) ;
#1501 = CARTESIAN_POINT ( 'NONE',  ( -61.19128421136908003, -282.5511546251398158, -343.4602108481794858 ) ) ;
#1502 = DIRECTION ( 'NONE',  ( -0.000000000000000000, 0.000000000000000000, -1.000000000000000000 ) ) ;
#1503 = CARTESIAN_POINT ( 'NONE',  ( -55.75508799387365855, -281.2888926331569905, -343.1185365373967215 ) ) ;
#1504 = DIRECTION ( 'NONE',  ( 0.000000000000000000, 0.000000000000000000, 1.000000000000000000 ) ) ;
#1505 = CARTESIAN_POINT ( 'NONE',  ( 34.87661588333293139, -292.1742611994909566, -257.1898032103383684 ) ) ;
#1506 = CARTESIAN_POINT ( 'NONE',  ( -80.00003502251276188, -283.6081244029235791, -209.5433377442685696 ) ) ;
#1507 = CARTESIAN_POINT ( 'NONE',  ( 228.6245981097501101, -142.7221692137691775, 21.50000000000000000 ) ) ;
#1508 = LINE ( 'NONE', #59764, #45796 ) ;
#1509 = CARTESIAN_POINT ( 'NONE',  ( -0.2458855626439184761, -290.5452906424620210, -205.1626475860752237 ) ) ;
#1510 = CARTESIAN_POINT ( 'NONE',  ( -68.35526443095929494, -279.0666212601479970, -337.3421645641082023 ) ) ;
#1511 = CARTESIAN_POINT ( 'NONE',  ( 0.6846499462318222928, -283.7619552028866110, -336.8744341544945087 ) ) ;
#1513 = CARTESIAN_POINT ( 'NONE',  ( -99.60931826203945150, -285.0783202633334668, -232.1630526575822842 ) ) ;
#1512 = CARTESIAN_POINT ( 'NONE',  ( -80.40917117863796193, -271.5538468486288934, -208.2130509116692281 ) ) ;
#1514 = CARTESIAN_POINT ( 'NONE',  ( 29.69846770327152896, -277.3831657951517400, -300.7089484258265202 ) ) ;
#1515 = CARTESIAN_POINT ( 'NONE',  ( -11.18678636406967186, -277.5051935538521661, -338.6877029478237091 ) ) ;
#1516 = CARTESIAN_POINT ( 'NONE',  ( -102.6622816111977556, -286.0600908051282545, -307.3203115391984852 ) ) ;
#1517 = EDGE_LOOP ( 'NONE', ( #90741, #8726, #54853, #21935 ) ) ;
#1518 = CARTESIAN_POINT ( 'NONE',  ( 200.4551663813218170, 64.49084098419280053, 0.000000000000000000 ) ) ;
#1519 = CARTESIAN_POINT ( 'NONE',  ( -56.07233749544652568, -295.1202883827519372, -345.0482201374624083 ) ) ;
#1520 = CARTESIAN_POINT ( 'NONE',  ( 34.24027624111162282, -289.2576488976930023, -249.1532017050213881 ) ) ;
#1521 = PLANE ( 'NONE',  #44283 ) ;
#1522 = CARTESIAN_POINT ( 'NONE',  ( 36.60358173371529489, -290.6237833571632905, -234.7871824221999191 ) ) ;
#1523 = CARTESIAN_POINT ( 'NONE',  ( -113.9014659788277157, -277.5287711341777594, -265.8783998487165263 ) ) ;
#1524 = EDGE_CURVE ( 'NONE', #92711, #90042, #92671, .T. ) ;
#1525 = CARTESIAN_POINT ( 'NONE',  ( -37.76987282709563232, -290.4467517415907309, -194.1623182098586824 ) ) ;
#1526 = CARTESIAN_POINT ( 'NONE',  ( -111.0840718524911921, -286.0647981291634210, -270.9338253024325809 ) ) ;
#1527 = CARTESIAN_POINT ( 'NONE',  ( -111.1710211117971312, -280.3801643721818664, -265.1452408090502786 ) ) ;
#1528 = CARTESIAN_POINT ( 'NONE',  ( 12.04888671161283931, -289.8060316138229382, -328.6635726732819194 ) ) ;
#1529 = CARTESIAN_POINT ( 'NONE',  ( 17.29998704130776233, -284.2728057879130006, -321.8100623489077066 ) ) ;
#1530 = CARTESIAN_POINT ( 'NONE',  ( -9.209842786283447325, -276.8610115028255905, -342.0381617762970450 ) ) ;
#1531 = CARTESIAN_POINT ( 'NONE',  ( -39.18421180120234482, -296.0490574145894129, -195.7263683417058360 ) ) ;
#1532 = CARTESIAN_POINT ( 'NONE',  ( -41.00627162774281231, -279.8405853337705480, -193.4351737076655979 ) ) ;
#1533 =( BOUNDED_CURVE ( )  B_SPLINE_CURVE ( 3, ( #22098, #93125, #56710, #43398 ),
 .UNSPECIFIED., .F., .F. ) 
 B_SPLINE_CURVE_WITH_KNOTS ( ( 4, 4 ),
 ( 1.570796326794895004, 2.004620063563923082 ),
 .UNSPECIFIED. ) 
 CURVE ( )  GEOMETRIC_REPRESENTATION_ITEM ( )  RATIONAL_B_SPLINE_CURVE ( ( 1.000000000000000000, 0.9843778111405747655, 0.9843778111405747655, 1.000000000000000000 ) ) 
 REPRESENTATION_ITEM ( '' )  );
#1534 = CARTESIAN_POINT ( 'NONE',  ( -108.8493213664828261, -298.7406335615847865, -249.6735781582797529 ) ) ;
#1535 = CARTESIAN_POINT ( 'NONE',  ( 155.8055003384388897, 17.52828139914081618, 8.087387968559804463 ) ) ;
#1536 = DIRECTION ( 'NONE',  ( -1.000000000000000000, 0.000000000000000000, 0.000000000000000000 ) ) ;
#1537 = AXIS2_PLACEMENT_3D ( 'NONE', #11772, #17497, #68618 ) ;
#1538 = CARTESIAN_POINT ( 'NONE',  ( -73.44339699170770075, -271.8202371963305950, -203.4397772358568091 ) ) ;
#1539 = DIRECTION ( 'NONE',  ( -1.000000000000000000, -0.000000000000000000, -0.000000000000000000 ) ) ;
#1540 = CARTESIAN_POINT ( 'NONE',  ( -110.0266555542237370, -278.1638359122140969, -262.4681452224736518 ) ) ;
#1541 = CARTESIAN_POINT ( 'NONE',  ( 5.661122632621188977, -277.6885939791913529, -333.7548554677638322 ) ) ;
#1542 = AXIS2_PLACEMENT_3D ( 'NONE', #35545, #85251, #20398 ) ;
#1543 = CARTESIAN_POINT ( 'NONE',  ( -55.65768918071592708, -282.3410986941567558, -344.9087185965823892 ) ) ;
#1544 = CARTESIAN_POINT ( 'NONE',  ( 23.59678886155491995, -289.8895293847145922, -312.3891160001019784 ) ) ;
#1545 = CARTESIAN_POINT ( 'NONE',  ( -37.27381386635783400, -299.5731044153225184, -194.0536722989971850 ) ) ;
#1546 = CARTESIAN_POINT ( 'NONE',  ( -43.27439573798378092, -299.1840176812871164, -193.9353343587565348 ) ) ;
#1547 = CARTESIAN_POINT ( 'NONE',  ( 27.81869143408052381, -295.0596889637145637, -233.4565744346762131 ) ) ;
#1548 = CARTESIAN_POINT ( 'NONE',  ( 37.52205576741398119, -279.5288648170840133, -268.5643515860454613 ) ) ;
#1549 = CARTESIAN_POINT ( 'NONE',  ( 14.95337341170095691, -284.2284178440503410, -323.4105009922290037 ) ) ;
#1550 = CARTESIAN_POINT ( 'NONE',  ( -24.28447781559408725, -272.2396343130468495, -196.8144476749051250 ) ) ;
#1551 = CARTESIAN_POINT ( 'NONE',  ( -95.64491491427668279, -285.4844500834294081, -319.4442754478668576 ) ) ;
#1552 = CARTESIAN_POINT ( 'NONE',  ( -31.86191381937559441, -287.9018474164876693, -343.5159773154330196 ) ) ;
#1553 = CARTESIAN_POINT ( 'NONE',  ( 140.5102961050414763, 179.4691865189072359, -241.1533972869285947 ) ) ;
#1554 = ORIENTED_EDGE ( 'NONE', *, *, #13930, .F. ) ;
#1555 = CARTESIAN_POINT ( 'NONE',  ( 37.24578009612667273, -286.3367520131498623, -287.0133803577105596 ) ) ;
#1556 = CARTESIAN_POINT ( 'NONE',  ( 30.50325596076029555, -287.5816946940914818, -297.5002385342463640 ) ) ;
#1557 = EDGE_LOOP ( 'NONE', ( #41598, #34259, #35254, #4428 ) ) ;
#1558 = CARTESIAN_POINT ( 'NONE',  ( -114.0181679633995628, -285.6722543968268724, -267.1411551968898834 ) ) ;
#1559 = CARTESIAN_POINT ( 'NONE',  ( 35.04090862371136694, -275.7583618527364706, -260.7254842694100034 ) ) ;
#1560 = CARTESIAN_POINT ( 'NONE',  ( 24.62835469155562507, -293.0748126654536350, -315.5629284065417437 ) ) ;
#1561 = CARTESIAN_POINT ( 'NONE',  ( 11.43435798209858056, -283.0478621234250340, -329.8792427238093410 ) ) ;
#1562 = CARTESIAN_POINT ( 'NONE',  ( 25.69681137297977358, -282.4989251112415900, -227.2706535599281494 ) ) ;
#1563 = CARTESIAN_POINT ( 'NONE',  ( -65.24056689306723911, -283.7402202951333834, -342.1206833954711328 ) ) ;
#1564 = CARTESIAN_POINT ( 'NONE',  ( 35.70842359217802198, -281.8619309966367723, -268.5788269733583320 ) ) ;
#1565 = CARTESIAN_POINT ( 'NONE',  ( -109.1418805571601069, -294.0523547857346784, -270.3284710469131937 ) ) ;
#1566 = CARTESIAN_POINT ( 'NONE',  ( 202.7079149121087198, 293.4844853417044988, -83.24464055084622771 ) ) ;
#1567 = VERTEX_POINT ( 'NONE', #67252 ) ;
#1568 = CARTESIAN_POINT ( 'NONE',  ( -23.97779326579380310, -278.8813625873251567, -344.0442539909758466 ) ) ;
#1569 = CARTESIAN_POINT ( 'NONE',  ( -23.12974717564393501, -107.7894168028556834, -362.0842449849661762 ) ) ;
#1570 = CARTESIAN_POINT ( 'NONE',  ( -110.3438963854144816, -295.8504482178817057, -274.1784481349151292 ) ) ;
#1571 = CARTESIAN_POINT ( 'NONE',  ( 24.83284670563353558, -293.6620419679333622, -315.7027587331984364 ) ) ;
#1572 = CARTESIAN_POINT ( 'NONE',  ( 65.57626950325040127, 46.04035155613875929, -315.5245225720349254 ) ) ;
#1573 = EDGE_CURVE ( 'NONE', #90412, #43035, #24613, .T. ) ;
#1575 = CARTESIAN_POINT ( 'NONE',  ( -83.05761992626356971, -288.0899159806922967, -328.2963843580874936 ) ) ;
#1574 = CARTESIAN_POINT ( 'NONE',  ( -100.2551300561488716, -295.7040920794071894, -226.9733230316642505 ) ) ;
#1576 = CARTESIAN_POINT ( 'NONE',  ( -35.59824836245590518, -296.8904974318918448, -344.5885532932438764 ) ) ;
#1577 = CARTESIAN_POINT ( 'NONE',  ( 15.37162616743650645, -288.1318320000314088, -219.1502918934397997 ) ) ;
#1578 = ORIENTED_EDGE ( 'NONE', *, *, #52624, .F. ) ;
#1579 = CARTESIAN_POINT ( 'NONE',  ( 6.489514836131241360, -295.4140806042470899, -333.4468814723030050 ) ) ;
#1580 = CARTESIAN_POINT ( 'NONE',  ( -57.41730933459302832, -286.2784353751287085, -200.0592000619339785 ) ) ;
#1581 = CARTESIAN_POINT ( 'NONE',  ( -54.49127349994017067, -296.6314533129871052, -195.7025561786944081 ) ) ;
#1582 = CARTESIAN_POINT ( 'NONE',  ( 19.28972365225641994, -293.6469338819406403, -218.4280778137662367 ) ) ;
#1583 = CARTESIAN_POINT ( 'NONE',  ( 27.99678076511742475, -293.5114966892802499, -229.6352269325376483 ) ) ;
#1584 = CARTESIAN_POINT ( 'NONE',  ( -104.7038899018843807, -291.0977518044177259, -242.0988807419200555 ) ) ;
#1585 = VERTEX_POINT ( 'NONE', #11336 ) ;
#1586 = CARTESIAN_POINT ( 'NONE',  ( 158.3977298502311157, 18.03393767897202693, 9.815540976419818264 ) ) ;
#1587 = CARTESIAN_POINT ( 'NONE',  ( -41.14521788562242222, -275.9249179403554990, -194.8456234185303231 ) ) ;
#1588 = CARTESIAN_POINT ( 'NONE',  ( 17.81441157817552678, -273.6147887391460927, -217.1265888411712126 ) ) ;
#1589 = ORIENTED_EDGE ( 'NONE', *, *, #28, .T. ) ;
#1590 = CARTESIAN_POINT ( 'NONE',  ( -93.29355369734641101, -277.3374731295478455, -323.2477723545381991 ) ) ;
#1591 = CARTESIAN_POINT ( 'NONE',  ( -69.82492212025711353, -272.0169028397427837, -204.0943789151146177 ) ) ;
#1592 = CARTESIAN_POINT ( 'NONE',  ( -94.91322446383126987, -281.0648676543580677, -223.4955115175889091 ) ) ;
#1593 = CARTESIAN_POINT ( 'NONE',  ( -72.25572342815260640, -275.6587097611486001, -335.8878727235614292 ) ) ;
#1594 = CARTESIAN_POINT ( 'NONE',  ( -103.4898831614755039, -274.0573957815899462, -238.7597896242689899 ) ) ;
#1595 = CARTESIAN_POINT ( 'NONE',  ( -38.09677444851720196, -274.9837151869672311, -197.1297154856137865 ) ) ;
#1596 = CARTESIAN_POINT ( 'NONE',  ( -110.8439382731208980, -274.5590712724159062, -250.8879076638938557 ) ) ;
#1597 = CARTESIAN_POINT ( 'NONE',  ( -13.55721941409112574, -272.3795423424051592, -198.8579342890237740 ) ) ;
#1598 = CARTESIAN_POINT ( 'NONE',  ( -69.76182583659532099, -296.1421888589821947, -335.8807953138737616 ) ) ;
#1599 = CARTESIAN_POINT ( 'NONE',  ( 14.72041401247748915, -292.8762895228433649, -322.4415078165400246 ) ) ;
#1600 = CARTESIAN_POINT ( 'NONE',  ( 11.63197158325052172, -331.8906705383788562, 57.50000000000000000 ) ) ;
#1601 = CARTESIAN_POINT ( 'NONE',  ( -4.015826881889136502, -277.1167301806580099, -339.7219329248168833 ) ) ;
#1602 = CARTESIAN_POINT ( 'NONE',  ( 21.47992204937843752, -275.1131098739491563, -227.1289913990223113 ) ) ;
#1603 = CARTESIAN_POINT ( 'NONE',  ( -111.7435278037817454, -283.0119462341349958, -288.2398208758913825 ) ) ;
#1604 = CARTESIAN_POINT ( 'NONE',  ( -104.3124203261300238, -298.1007224023215372, -304.6070781542059080 ) ) ;
#1605 = CARTESIAN_POINT ( 'NONE',  ( -25.10477003004976737, -285.4092135434137845, -198.1788573615894222 ) ) ;
#1606 = CARTESIAN_POINT ( 'NONE',  ( -109.3589609794314441, -282.2747094004473638, -291.9359041034900883 ) ) ;
#1607 = CARTESIAN_POINT ( 'NONE',  ( -81.44086963633981213, -275.9012561383001980, -329.8021581798747093 ) ) ;
#1608 = CARTESIAN_POINT ( 'NONE',  ( -43.27252726397514948, -275.7032369514942047, -343.7109660178809918 ) ) ;
#1610 = CARTESIAN_POINT ( 'NONE',  ( -51.28233074770404443, -281.8742238388606438, -196.6158302983829742 ) ) ;
#1609 = CIRCLE ( 'NONE', #49999, 0.5000000000000004441 ) ;
#1611 = CARTESIAN_POINT ( 'NONE',  ( 35.50211883959628523, -276.8805763525704720, -279.7620530667037997 ) ) ;
#1612 = CYLINDRICAL_SURFACE ( 'NONE', #21692, 24.00000000000000355 ) ;
#1613 = CARTESIAN_POINT ( 'NONE',  ( 24.68765769267331578, -273.3593948587888462, -226.0804652099130010 ) ) ;
#1614 = AXIS2_PLACEMENT_3D ( 'NONE', #18179, #47029, #23426 ) ;
#1615 = CARTESIAN_POINT ( 'NONE',  ( -72.92088819288660773, -281.5820908632840656, -204.1336082957760425 ) ) ;
#1616 = CARTESIAN_POINT ( 'NONE',  ( 195.3965999132940397, 19.72393862741004611, 13.34571198792791868 ) ) ;
#1617 = CARTESIAN_POINT ( 'NONE',  ( 21.84831040855851469, -288.8315702692190143, -223.3739541679873355 ) ) ;
#1618 = DIRECTION ( 'NONE',  ( -0.000000000000000000, -1.000000000000000000, 0.000000000000000000 ) ) ;
#1619 = CARTESIAN_POINT ( 'NONE',  ( -83.46247577153260977, -289.4201316962644910, -211.1532311690369852 ) ) ;
#1620 = DIRECTION ( 'NONE',  ( -1.000000000000000000, 0.000000000000000000, -0.000000000000000000 ) ) ;
#1621 = CARTESIAN_POINT ( 'NONE',  ( -60.62740868408015871, -296.5383017693818033, -200.7020011217740603 ) ) ;
#1622 = CARTESIAN_POINT ( 'NONE',  ( -65.77857512665582362, -289.8157886128017253, -201.7747179894851115 ) ) ;
#1623 = CARTESIAN_POINT ( 'NONE',  ( 202.9738562182569694, 291.4636489450776367, -54.00000000000002132 ) ) ;
#1624 = CARTESIAN_POINT ( 'NONE',  ( 188.2019740231993410, 44.81720372851549428, 10.50000000000000000 ) ) ;
#1625 = CARTESIAN_POINT ( 'NONE',  ( 14.12169607694052154, -286.8252731300303822, -326.7729787424775054 ) ) ;
#1626 = CARTESIAN_POINT ( 'NONE',  ( -61.78063094932833366, -284.9751209561533756, -340.0509784335445715 ) ) ;
#1627 = CARTESIAN_POINT ( 'NONE',  ( -113.1983268329517500, -282.7253018832102498, -275.6249542651085562 ) ) ;
#1628 = CARTESIAN_POINT ( 'NONE',  ( -106.5712913338532104, -290.8597095495214830, -247.2037497926789058 ) ) ;
#1629 = CARTESIAN_POINT ( 'NONE',  ( 5.249533110438283856, -282.0664097247295103, -210.3497709975815440 ) ) ;
#1630 = CARTESIAN_POINT ( 'NONE',  ( 21.94878897923050687, -282.9535193080128579, -313.2456052752808091 ) ) ;
#1631 = ADVANCED_FACE ( 'NONE', ( #76207 ), #91321, .T. ) ;
#1632 = CARTESIAN_POINT ( 'NONE',  ( -45.81522711214778099, -291.1388278857802447, -345.2903830732265646 ) ) ;
#1633 = CARTESIAN_POINT ( 'NONE',  ( -35.83027923402509884, -298.2372649447141839, -193.3610765279775308 ) ) ;
#1634 = ORIENTED_EDGE ( 'NONE', *, *, #50049, .T. ) ;
#1635 = CARTESIAN_POINT ( 'NONE',  ( 33.70987938463910893, -285.9646333182316198, -296.2228784914229323 ) ) ;
#1636 = CARTESIAN_POINT ( 'NONE',  ( 37.23874443599788719, -275.7918163529477056, -289.5120262801918329 ) ) ;
#1637 = CARTESIAN_POINT ( 'NONE',  ( -33.44728051850636774, -294.0812828094680640, -195.8052002624553722 ) ) ;
#1638 = DIRECTION ( 'NONE',  ( -1.000000000000000000, 0.000000000000000000, 0.000000000000000000 ) ) ;
#1639 = CARTESIAN_POINT ( 'NONE',  ( -20.25526795762937127, -288.7662352645560304, -195.3538533559490702 ) ) ;
#1640 = CARTESIAN_POINT ( 'NONE',  ( -104.7137483946727485, -276.1118192998647487, -303.8105025117007472 ) ) ;
#1641 = CARTESIAN_POINT ( 'NONE',  ( 208.6470931340251695, 37.28147638844021117, 12.02381566707520300 ) ) ;
#1642 = CARTESIAN_POINT ( 'NONE',  ( -51.63041121882034901, -296.2723257764641289, -195.4590116835833271 ) ) ;
#1643 = CARTESIAN_POINT ( 'NONE',  ( 23.88339583151003254, -274.3480442087875986, -230.4189060645270217 ) ) ;
#1644 = CARTESIAN_POINT ( 'NONE',  ( -86.40492894914859789, -292.8767248358395818, -215.3059888203697483 ) ) ;
#1645 = CARTESIAN_POINT ( 'NONE',  ( -102.6247317423333527, -291.9440526826926430, -237.0594543679127071 ) ) ;
#1646 = CARTESIAN_POINT ( 'NONE',  ( -108.3332381675128033, -286.5875715375530035, -249.2505357775856112 ) ) ;
#1647 = CARTESIAN_POINT ( 'NONE',  ( 18.96906400359628719, -294.2692731210215129, -218.7112957561428175 ) ) ;
#1648 = CARTESIAN_POINT ( 'NONE',  ( 23.57236081994135191, -294.2462215614904153, -224.0494428861379674 ) ) ;
#1649 = CARTESIAN_POINT ( 'NONE',  ( -28.89808635804783421, -294.7755900316942643, -342.9221680128125058 ) ) ;
#1650 = CARTESIAN_POINT ( 'NONE',  ( 30.03535396789157730, -289.9866415594360092, -303.3055139700287555 ) ) ;
#1651 = CARTESIAN_POINT ( 'NONE',  ( -38.73041907186327393, -283.2357985498580888, -347.3485940044810150 ) ) ;
#1652 = CARTESIAN_POINT ( 'NONE',  ( -56.99122451320729965, -295.8806285197832153, -197.3465436105504409 ) ) ;
#1653 = CARTESIAN_POINT ( 'NONE',  ( -98.04573195976770705, -283.7525300390229290, -317.7322117414312288 ) ) ;
#1654 = CARTESIAN_POINT ( 'NONE',  ( -21.27495461195972126, -278.8251003981005738, -343.3094607102461282 ) ) ;
#1655 = EDGE_CURVE ( 'NONE', #7585, #19412, #71553, .T. ) ;
#1656 = CARTESIAN_POINT ( 'NONE',  ( -68.93200677907188378, -284.4221688895109423, -204.0963455160231206 ) ) ;
#1657 = CARTESIAN_POINT ( 'NONE',  ( 34.46303846749501787, -285.8316026620146886, -292.0639301913859640 ) ) ;
#1658 = CARTESIAN_POINT ( 'NONE',  ( -105.0607483084268523, -277.1372776232107071, -236.2673513917142714 ) ) ;
#1659 = CARTESIAN_POINT ( 'NONE',  ( 5.045406874201050940, -57.93311274753654061, -355.0152878038887820 ) ) ;
#1660 = CARTESIAN_POINT ( 'NONE',  ( -110.3706500880485493, -284.0885611170499487, -268.1791672015494328 ) ) ;
#1661 = CARTESIAN_POINT ( 'NONE',  ( 23.94669089585513788, -283.3719839339678401, -316.3148103849359813 ) ) ;
#1662 = CARTESIAN_POINT ( 'NONE',  ( -54.46084228448783904, -288.3255161109215692, -345.2471763931627606 ) ) ;
#1663 = CARTESIAN_POINT ( 'NONE',  ( -101.4131643431225314, -279.6042918162672777, -311.7040340098704974 ) ) ;
#1664 = CARTESIAN_POINT ( 'NONE',  ( -4.193266073220160095, -277.9394237644120267, -339.3282602488646944 ) ) ;
#1665 = CARTESIAN_POINT ( 'NONE',  ( -93.93918323399981318, -279.0380998051352890, -224.2555336070021212 ) ) ;
#1666 = CARTESIAN_POINT ( 'NONE',  ( 16.61875949127060892, -276.8037087073536782, -218.7100151731984852 ) ) ;
#1667 = CARTESIAN_POINT ( 'NONE',  ( 33.58617426899444069, -285.2428112634257218, -246.5018418112450433 ) ) ;
#1668 = CARTESIAN_POINT ( 'NONE',  ( -100.0109376011833859, -291.5737769913471880, -313.7086333703326204 ) ) ;
#1669 = CARTESIAN_POINT ( 'NONE',  ( -28.87386692168243840, -293.8627457906940776, -343.2307640320604492 ) ) ;
#1670 = EDGE_LOOP ( 'NONE', ( #9116, #72630, #35817, #56102 ) ) ;
#1671 = EDGE_CURVE ( 'NONE', #70513, #36421, #78434, .T. ) ;
#1672 = CARTESIAN_POINT ( 'NONE',  ( 8.238055427622166249, -294.0756715581831031, -327.4749674202749361 ) ) ;
#1673 = CARTESIAN_POINT ( 'NONE',  ( -92.59894787587302289, -292.3634276051635652, -217.1053951106169677 ) ) ;
#1674 = CARTESIAN_POINT ( 'NONE',  ( 27.86857600094925047, -281.7542677208724058, -237.2108550677822052 ) ) ;
#1675 = CARTESIAN_POINT ( 'NONE',  ( -99.36982232666682080, -272.2140105371391883, -225.0476431559881405 ) ) ;
#1676 = CARTESIAN_POINT ( 'NONE',  ( 38.01006813017163921, -288.3957084094379297, -285.7046445438832052 ) ) ;
#1677 = CARTESIAN_POINT ( 'NONE',  ( -71.89317434194919088, -289.8296844647853732, -339.1502153838598019 ) ) ;
#1678 = CARTESIAN_POINT ( 'NONE',  ( 6.936376980029636208, -287.0068658301630080, -212.2322763371211352 ) ) ;
#1679 = CARTESIAN_POINT ( 'NONE',  ( 193.6317248235833404, 279.2590636267979107, -125.8091547552216696 ) ) ;
#1680 = CARTESIAN_POINT ( 'NONE',  ( -40.95723928608203579, -138.9634190178281017, -362.8174797514035959 ) ) ;
#1681 = CARTESIAN_POINT ( 'NONE',  ( -110.1558835859493968, -268.3047593149524914, -295.2634325463859000 ) ) ;
#1682 = CIRCLE ( 'NONE', #34945, 24.50000000000000355 ) ;
#1683 = CARTESIAN_POINT ( 'NONE',  ( -68.11462822946306517, -276.6640491675283329, -336.7498066479569729 ) ) ;
#1684 = CARTESIAN_POINT ( 'NONE',  ( -109.0700602599650608, -277.2735774419044787, -285.5027304255098670 ) ) ;
#1685 = CARTESIAN_POINT ( 'NONE',  ( -104.2090589165651693, -272.7155564601540050, -232.1162379136689538 ) ) ;
#1686 = CARTESIAN_POINT ( 'NONE',  ( 140.1414760274805076, 178.0338941539027928, -239.0129668939350722 ) ) ;
#1687 = CARTESIAN_POINT ( 'NONE',  ( -72.62822590452525162, -276.1942376163574977, -338.2591537605787835 ) ) ;
#1688 = CARTESIAN_POINT ( 'NONE',  ( -63.89086097342256210, -297.1538220072495164, -341.5588431689091635 ) ) ;
#1689 = CARTESIAN_POINT ( 'NONE',  ( -99.76743922069182702, -291.5668651502261923, -232.4004075003451248 ) ) ;
#1690 = CARTESIAN_POINT ( 'NONE',  ( -40.44399816664863323, -298.8170463662104339, -193.5332289811452142 ) ) ;
#1691 = CARTESIAN_POINT ( 'NONE',  ( 10.42314873493027605, -287.0616546680848842, -326.2832302609623980 ) ) ;
#1692 = CARTESIAN_POINT ( 'NONE',  ( -70.09590052288301365, -274.2833510363454934, -200.7731998446884063 ) ) ;
#1693 = CARTESIAN_POINT ( 'NONE',  ( -105.8065692134149742, -297.0583119299714099, -244.8862325304627632 ) ) ;
#1694 = ORIENTED_EDGE ( 'NONE', *, *, #2190, .F. ) ;
#1695 = CARTESIAN_POINT ( 'NONE',  ( 196.8803347170859865, 20.19615242270661426, 12.49999999999999289 ) ) ;
#1696 = CARTESIAN_POINT ( 'NONE',  ( -70.62278491564876504, -281.5368598035303194, -202.5254076392495506 ) ) ;
#1697 = CARTESIAN_POINT ( 'NONE',  ( -99.73802623321135741, -280.1613682758161303, -231.7814645895975048 ) ) ;
#1698 = CARTESIAN_POINT ( 'NONE',  ( -102.5536271241169999, -280.8288154844870519, -231.2539062438021062 ) ) ;
#1699 = CARTESIAN_POINT ( 'NONE',  ( -69.77886387602367790, -272.0968963081243146, -204.1905946158020697 ) ) ;
#1700 = CYLINDRICAL_SURFACE ( 'NONE', #14009, 2.000000000000000888 ) ;
#1701 = DIRECTION ( 'NONE',  ( -0.000000000000000000, -1.000000000000000000, -0.000000000000000000 ) ) ;
#1702 = CARTESIAN_POINT ( 'NONE',  ( 27.78043308788700472, -281.2696125430865663, -237.2625616980432994 ) ) ;
#1703 = CARTESIAN_POINT ( 'NONE',  ( 21.61332023554981419, -277.0195259890290345, -319.6405700392683684 ) ) ;
#1704 = CARTESIAN_POINT ( 'NONE',  ( 37.63089621855161226, -277.5262850220284463, -268.3336952890500129 ) ) ;
#1705 = CARTESIAN_POINT ( 'NONE',  ( -73.83156038324176507, -276.1016415619488953, -337.5109186801022929 ) ) ;
#1706 = ORIENTED_EDGE ( 'NONE', *, *, #90632, .F. ) ;
#1707 = CARTESIAN_POINT ( 'NONE',  ( 208.6208076322478746, 32.98517505407394168, 10.00000000000000000 ) ) ;
#1708 = CARTESIAN_POINT ( 'NONE',  ( 14.63759705836963931, -284.3045538116586499, -324.9189722741356832 ) ) ;
#1709 = CARTESIAN_POINT ( 'NONE',  ( -41.59201825942352571, -291.1945583554368113, -197.2732493876959268 ) ) ;
#1710 = CARTESIAN_POINT ( 'NONE',  ( -57.72092388568977128, -285.1444226616906690, -196.1573414579531232 ) ) ;
#1711 = CARTESIAN_POINT ( 'NONE',  ( -98.38058555856424903, -282.2162676906381193, -312.3101062699920476 ) ) ;
#1713 = CARTESIAN_POINT ( 'NONE',  ( -16.75054076332084563, -284.3998962782931130, -198.7717882874051156 ) ) ;
#1712 = CARTESIAN_POINT ( 'NONE',  ( -93.88638208250931427, -282.4639869158099259, -317.4575494970145542 ) ) ;
#1714 = CARTESIAN_POINT ( 'NONE',  ( 17.34849390122006696, -282.0606634836764215, -221.4110088670058474 ) ) ;
#1715 = CARTESIAN_POINT ( 'NONE',  ( -93.56973896943168256, -271.2420196192170465, -220.7283838381425483 ) ) ;
#1716 = CARTESIAN_POINT ( 'NONE',  ( -19.12955568641073612, -281.2215781850163694, -344.4071103187382619 ) ) ;
#1717 = CARTESIAN_POINT ( 'NONE',  ( 37.65509890419795624, -295.5154156613767782, -267.4871558678684664 ) ) ;
#1718 = CARTESIAN_POINT ( 'NONE',  ( -99.25701812256976098, -278.6665012165066742, -309.3193415530338939 ) ) ;
#1719 = CARTESIAN_POINT ( 'NONE',  ( -32.45174577122553217, -288.1138060289943610, -195.3408202976878556 ) ) ;
#1720 = DIRECTION ( 'NONE',  ( 0.3428573139466625785, 0.000000000000000000, -0.9393874931428880526 ) ) ;
#1721 = CARTESIAN_POINT ( 'NONE',  ( -1.508721186066707354, -294.4436026337680232, -203.8381007628641157 ) ) ;
#1722 = CARTESIAN_POINT ( 'NONE',  ( -5.448659697826840898, -274.6324594844787725, -338.2562938210186303 ) ) ;
#1723 = CARTESIAN_POINT ( 'NONE',  ( -36.09972708781004513, -288.2341572508835839, -347.2026873767308075 ) ) ;
#1724 = CARTESIAN_POINT ( 'NONE',  ( 34.43051265496536928, -291.7271723914418544, -253.1259753565562391 ) ) ;
#1725 = CARTESIAN_POINT ( 'NONE',  ( -43.30989527892933921, -271.8033297790818779, -432.4918912919293916 ) ) ;
#1726 = CARTESIAN_POINT ( 'NONE',  ( -87.44387726973756969, -276.4538294353628203, -324.1292807067435433 ) ) ;
#1727 = CARTESIAN_POINT ( 'NONE',  ( -82.68008778736489717, -295.5650021513290540, -211.5142173663683707 ) ) ;
#1728 = CARTESIAN_POINT ( 'NONE',  ( -58.81734638578565466, -290.6508741178286641, -340.6996931017167753 ) ) ;
#1729 = CARTESIAN_POINT ( 'NONE',  ( 104.2209783822911646, -299.5541904835127980, -197.2595231212879128 ) ) ;
#1730 = CARTESIAN_POINT ( 'NONE',  ( 209.7513585654923816, 282.2246705312486483, -40.00000000000000711 ) ) ;
#1731 = CARTESIAN_POINT ( 'NONE',  ( 12.83723111402624717, -291.2176547326198488, -212.8738793080092933 ) ) ;
#1732 = CARTESIAN_POINT ( 'NONE',  ( -10.47754207642720381, -288.0086995450054133, -201.6105746577587468 ) ) ;
#1733 = CARTESIAN_POINT ( 'NONE',  ( -109.4619355597749433, -289.0991326456193065, -246.2665912077229109 ) ) ;
#1734 = CARTESIAN_POINT ( 'NONE',  ( -9.285407649390574392, -287.8515147177142808, -202.3164850531241257 ) ) ;
#1735 = CARTESIAN_POINT ( 'NONE',  ( 199.0061125298537377, 250.5000000000000568, -7.725424859374024678 ) ) ;
#1736 = CARTESIAN_POINT ( 'NONE',  ( 17.89139397278936272, -287.6724992839841661, -222.3829245675862296 ) ) ;
#1737 = EDGE_CURVE ( 'NONE', #23799, #17402, #5377, .T. ) ;
#1738 = CARTESIAN_POINT ( 'NONE',  ( -16.92769768841934308, -296.7698506742665927, -342.9525830315375856 ) ) ;
#1739 = FACE_OUTER_BOUND ( 'NONE', #32338, .T. ) ;
#1740 = CARTESIAN_POINT ( 'NONE',  ( -67.88140272164058331, -290.6492842725307924, -340.6130594856963398 ) ) ;
#1741 = CARTESIAN_POINT ( 'NONE',  ( -83.53826820392886532, -277.4427159650949193, -210.7612128747612701 ) ) ;
#1742 = CARTESIAN_POINT ( 'NONE',  ( -107.5550754441970440, -278.4808297995886051, -302.0475220878240634 ) ) ;
#1743 = CARTESIAN_POINT ( 'NONE',  ( -59.29205138593874835, -279.4422652223107661, -196.5781499539828587 ) ) ;
#1744 = CARTESIAN_POINT ( 'NONE',  ( -111.6275770537671264, -274.5438608122422011, -264.8303458579267726 ) ) ;
#1745 = CARTESIAN_POINT ( 'NONE',  ( -110.8852626855045571, -282.7408513014555069, -255.6524450881647113 ) ) ;
#1746 = CARTESIAN_POINT ( 'NONE',  ( 197.3748232817348764, 249.5000000000000568, -12.45182892472558756 ) ) ;
#1747 = CARTESIAN_POINT ( 'NONE',  ( -32.86525229271969550, -278.2487364192615473, -196.2610039735248790 ) ) ;
#1748 = CARTESIAN_POINT ( 'NONE',  ( -47.02406441949805327, -281.1749854335209307, -344.7335084835086718 ) ) ;
#1749 = DIRECTION ( 'NONE',  ( 0.000000000000000000, 0.000000000000000000, 1.000000000000000000 ) ) ;
#1750 = CARTESIAN_POINT ( 'NONE',  ( 34.54124994593603049, -274.3598898357928988, -296.1204461415946980 ) ) ;
#1751 = AXIS2_PLACEMENT_3D ( 'NONE', #1735, #81729, #16877 ) ;
#1752 = CARTESIAN_POINT ( 'NONE',  ( -95.00583646348886191, -298.7141436636807157, -224.4747895665826150 ) ) ;
#1753 = CARTESIAN_POINT ( 'NONE',  ( -113.8424131155087764, -283.5491046231293240, -264.2590879456490711 ) ) ;
#1754 = CARTESIAN_POINT ( 'NONE',  ( -105.5705267591125249, -273.7087470362338308, -243.8124391693121424 ) ) ;
#1755 = CARTESIAN_POINT ( 'NONE',  ( -71.15848572856612009, -275.0397685359516231, -201.8408194792957033 ) ) ;
#1756 = CARTESIAN_POINT ( 'NONE',  ( 32.91704035997975808, -275.4823496738562199, -290.3015106855962131 ) ) ;
#1757 = CARTESIAN_POINT ( 'NONE',  ( -74.26544743721966313, -297.5432225604704399, -335.6423368310926207 ) ) ;
#1758 = CARTESIAN_POINT ( 'NONE',  ( -70.63714881898405906, -289.6457532169164892, -339.8047985140610194 ) ) ;
#1759 = CARTESIAN_POINT ( 'NONE',  ( -96.55293578398048737, -277.2721440031359066, -223.4213291589378230 ) ) ;
#1760 = CARTESIAN_POINT ( 'NONE',  ( -106.5144451201724678, -289.9497529572378767, -304.3073330078760819 ) ) ;
#1761 = EDGE_CURVE ( 'NONE', #65093, #10127, #91797, .T. ) ;
#1762 = EDGE_CURVE ( 'NONE', #5855, #73562, #18431, .T. ) ;
#1763 = B_SPLINE_CURVE_WITH_KNOTS ( 'NONE', 3,
 ( #706, #29590, #44697, #7785, #81151, #43765 ),
 .UNSPECIFIED., .F., .F.,
 ( 4, 2, 4 ),
 ( 0.000000000000000000, 0.0005961816168538936920, 0.001192363233707787384 ),
 .UNSPECIFIED. ) ;
#1764 = CARTESIAN_POINT ( 'NONE',  ( -108.5820832139279304, -289.3876441017661705, -287.3380513535951195 ) ) ;
#1765 = CARTESIAN_POINT ( 'NONE',  ( 35.82698505982688886, -291.7642438145344954, -286.8915267809055081 ) ) ;
#1766 = ORIENTED_EDGE ( 'NONE', *, *, #4077, .T. ) ;
#1767 = DIRECTION ( 'NONE',  ( 0.000000000000000000, 0.000000000000000000, 1.000000000000000000 ) ) ;
#1768 = CARTESIAN_POINT ( 'NONE',  ( -106.0925958599700465, -289.7307947647781248, -295.0856559489138249 ) ) ;
#1769 = DIRECTION ( 'NONE',  ( 0.000000000000000000, 0.000000000000000000, 1.000000000000000000 ) ) ;
#1770 = CARTESIAN_POINT ( 'NONE',  ( 1.392570185844214992, -287.4976627473723738, -204.0700665931116475 ) ) ;
#1771 = CARTESIAN_POINT ( 'NONE',  ( -102.0455923789670294, -293.4805209788416391, -239.2376011013261916 ) ) ;
#1772 = CARTESIAN_POINT ( 'NONE',  ( 27.89960822025720688, -293.1427056974741845, -310.9133012240417884 ) ) ;
#1773 = CARTESIAN_POINT ( 'NONE',  ( 23.02420457184907931, -283.4994896818116672, -317.3850154914642872 ) ) ;
#1774 = CARTESIAN_POINT ( 'NONE',  ( -106.5316306012337861, -284.6965418625353550, -246.9272506044068507 ) ) ;
#1775 = CARTESIAN_POINT ( 'NONE',  ( 35.50714259502728964, -276.7400963198646764, -260.6508351919949291 ) ) ;
#1776 = CARTESIAN_POINT ( 'NONE',  ( 14.05351214020076256, -290.7980791656141832, -216.2281432195725870 ) ) ;
#1777 = CARTESIAN_POINT ( 'NONE',  ( -59.58142725297764031, -272.5526756193522147, -200.3613257485492909 ) ) ;
#1778 = ORIENTED_EDGE ( 'NONE', *, *, #19590, .F. ) ;
#1779 = CARTESIAN_POINT ( 'NONE',  ( 197.0349383350915105, 285.8449894349855640, -111.9383547020201064 ) ) ;
#1780 = CARTESIAN_POINT ( 'NONE',  ( 36.34821029528860237, -293.5004040039983124, -292.8024142208167291 ) ) ;
#1781 = CARTESIAN_POINT ( 'NONE',  ( -69.41714365519545993, -287.5468926363182049, -203.1720575300506368 ) ) ;
#1782 = CARTESIAN_POINT ( 'NONE',  ( -97.11410897010547671, -298.2783381992039722, -222.3116470947955747 ) ) ;
#1783 = EDGE_CURVE ( 'NONE', #27568, #44950, #62480, .T. ) ;
#1784 = CARTESIAN_POINT ( 'NONE',  ( 0.2139193248535528891, -287.2176141071593634, -207.5847406664543939 ) ) ;
#1785 = CARTESIAN_POINT ( 'NONE',  ( -110.4462887999276006, -277.3135881266629212, -293.9532670338982712 ) ) ;
#1786 = CARTESIAN_POINT ( 'NONE',  ( 36.60385736321685357, -293.9381248450672501, -249.2094290896874895 ) ) ;
#1787 = CARTESIAN_POINT ( 'NONE',  ( 6.843122370839409996, -284.7854164591011568, -208.7497002104346677 ) ) ;
#1788 = CARTESIAN_POINT ( 'NONE',  ( 39.58590878396767465, -293.9205655783236466, -273.1695478845242064 ) ) ;
#1789 = CARTESIAN_POINT ( 'NONE',  ( -38.90228509564093429, -292.3653207151177753, -197.3566519450759245 ) ) ;
#1790 = DIRECTION ( 'NONE',  ( -0.000000000000000000, -0.000000000000000000, -1.000000000000000000 ) ) ;
#1791 = DIRECTION ( 'NONE',  ( 0.000000000000000000, 0.000000000000000000, -1.000000000000000000 ) ) ;
#1792 = LINE ( 'NONE', #80865, #778 ) ;
#1793 = CARTESIAN_POINT ( 'NONE',  ( -111.1989583166938615, -285.8294593436967261, -289.5913245281645914 ) ) ;
#1794 = CARTESIAN_POINT ( 'NONE',  ( -2.602324593224659921, -289.9809262143061233, -198.2974183793908196 ) ) ;
#1795 = ORIENTED_EDGE ( 'NONE', *, *, #45672, .T. ) ;
#1796 = CARTESIAN_POINT ( 'NONE',  ( -100.6750664868626473, -282.9679147868390601, -307.2814481363535606 ) ) ;
#1797 = CARTESIAN_POINT ( 'NONE',  ( -112.3801697928137457, -278.4337261398576970, -253.1863585357417321 ) ) ;
#1798 = CARTESIAN_POINT ( 'NONE',  ( 33.98635713539291459, -283.8470210494004959, -293.1649254477694058 ) ) ;
#1799 = CARTESIAN_POINT ( 'NONE',  ( -68.75627247708085577, -197.2056770039593800, -358.9513570765641362 ) ) ;
#1800 = CARTESIAN_POINT ( 'NONE',  ( -102.0100645232851235, -283.6639919249153081, -229.6596568464721884 ) ) ;
#1801 = CARTESIAN_POINT ( 'NONE',  ( -33.12099484864842935, -284.1255411062354597, -195.7847949867546333 ) ) ;
#1802 = CARTESIAN_POINT ( 'NONE',  ( -73.37858195186689159, -275.4402094594785240, -203.6570937117227516 ) ) ;
#1803 = CARTESIAN_POINT ( 'NONE',  ( -103.7771577347053409, -297.4556265425305810, -239.8367178318573849 ) ) ;
#1804 = CARTESIAN_POINT ( 'NONE',  ( -9.056457237376076108, -293.3591745649421227, -338.2068753026957211 ) ) ;
#1805 = CARTESIAN_POINT ( 'NONE',  ( -100.3771874552530221, -278.6205601094512758, -314.4047341385949039 ) ) ;
#1806 = CARTESIAN_POINT ( 'NONE',  ( -5.066084614251986196, -276.6150721985752057, -335.8523681797399263 ) ) ;
#1807 = CARTESIAN_POINT ( 'NONE',  ( -29.10309227451535463, -299.0941803680265707, -193.5951300305619327 ) ) ;
#1808 = CARTESIAN_POINT ( 'NONE',  ( -41.38196488513791849, -276.0222064098941814, -346.9586636101758472 ) ) ;
#1809 = DIRECTION ( 'NONE',  ( -0.7453559924999200170, 0.000000000000000000, -0.6666666666666777319 ) ) ;
#1810 = CARTESIAN_POINT ( 'NONE',  ( 1.642048719780067723, -274.5311979272196368, -334.4928091907234489 ) ) ;
#1811 = CARTESIAN_POINT ( 'NONE',  ( -94.20088447847305702, -297.2792722567077135, -321.4260710656061519 ) ) ;
#1812 = FACE_OUTER_BOUND ( 'NONE', #17774, .T. ) ;
#1813 = CIRCLE ( 'NONE', #47133, 7.999911143031724237 ) ;
#1814 = CARTESIAN_POINT ( 'NONE',  ( 210.6911334572095598, 1.334076891925523281E-16, -7.166221634559009956 ) ) ;
#1815 = VECTOR ( 'NONE', #7572, 1000.000000000000000 ) ;
#1816 = CARTESIAN_POINT ( 'NONE',  ( -51.06232668424904375, -284.3111810020899384, -342.4265939081700481 ) ) ;
#1817 = CARTESIAN_POINT ( 'NONE',  ( -58.18695516619104069, -285.0779114967170926, -343.4874171420436824 ) ) ;
#1818 = CARTESIAN_POINT ( 'NONE',  ( 26.46039246488074070, -286.4121096519637035, -234.5758016373251280 ) ) ;
#1819 = CARTESIAN_POINT ( 'NONE',  ( -109.9151448130932636, -277.1268606013946396, -256.9620305849495026 ) ) ;
#1820 = CARTESIAN_POINT ( 'NONE',  ( -108.1571726745488746, -286.1222769201293090, -292.6329461194868031 ) ) ;
#1821 = CARTESIAN_POINT ( 'NONE',  ( -94.46582077498722185, -277.6848769671270816, -223.8042431424522931 ) ) ;
#1822 = CARTESIAN_POINT ( 'NONE',  ( -69.37412025191891018, -278.5634823524354147, -336.3155171318732073 ) ) ;
#1823 = CARTESIAN_POINT ( 'NONE',  ( 201.2104617360081704, 15.00000000000000000, 10.00000000000000000 ) ) ;
#1824 = CARTESIAN_POINT ( 'NONE',  ( -89.29032893170928276, -273.7885074658303779, -218.9867235136785553 ) ) ;
#1825 = CARTESIAN_POINT ( 'NONE',  ( 30.93834349328282229, -282.8102028399933943, -305.6030598001290173 ) ) ;
#1826 = CARTESIAN_POINT ( 'NONE',  ( 4.517479994103495322, -282.9962868592525069, -334.9789950446512989 ) ) ;
#1827 = ORIENTED_EDGE ( 'NONE', *, *, #52934, .F. ) ;
#1828 = VERTEX_POINT ( 'NONE', #68169 ) ;
#1829 = CARTESIAN_POINT ( 'NONE',  ( 196.8803347170860150, 20.19615242270657163, -12.49999999999990941 ) ) ;
#1830 = CARTESIAN_POINT ( 'NONE',  ( 25.32221201533798194, -288.8416344733199139, -227.7522788152095927 ) ) ;
#1831 = ADVANCED_FACE ( 'NONE', ( #40648 ), #55492, .T. ) ;
#1832 = CARTESIAN_POINT ( 'NONE',  ( -94.57125394193877810, -296.3915653539483515, -224.7828348002563814 ) ) ;
#1833 = CARTESIAN_POINT ( 'NONE',  ( 23.89908980660779747, -292.2799524007357945, -223.8326897184352049 ) ) ;
#1834 = CARTESIAN_POINT ( 'NONE',  ( 34.38961951593933719, -285.8105842117641373, -253.4149402577371006 ) ) ;
#1835 = CARTESIAN_POINT ( 'NONE',  ( -82.92535760314615345, -288.2647439289552835, -328.1322620478383669 ) ) ;
#1836 = CARTESIAN_POINT ( 'NONE',  ( -11.89864875897552565, -287.5959707400330103, -201.5150458956920829 ) ) ;
#1837 = CARTESIAN_POINT ( 'NONE',  ( -110.8389557672072527, -276.3593710714950475, -285.3630322165855659 ) ) ;
#1838 = CARTESIAN_POINT ( 'NONE',  ( 19.01866782242020193, -286.6565357626554373, -321.6635789817046316 ) ) ;
#1839 = CARTESIAN_POINT ( 'NONE',  ( 24.68852241357335942, -288.9813564656793687, -228.1807187303758440 ) ) ;
#1840 = CARTESIAN_POINT ( 'NONE',  ( -43.06863983722212197, -287.1241451343416884, -345.3093040083568894 ) ) ;
#1841 = CARTESIAN_POINT ( 'NONE',  ( 16.00545805336161465, -283.2140681170793641, -320.6088823929226237 ) ) ;
#1842 = CARTESIAN_POINT ( 'NONE',  ( -89.53178805703595344, -293.3193760021130743, -216.1942795588795718 ) ) ;
#1843 = CARTESIAN_POINT ( 'NONE',  ( 82.12427740513938090, -301.4850002582832076, -194.7971909733571465 ) ) ;
#1844 = CARTESIAN_POINT ( 'NONE',  ( 197.1123855246549113, 19.09807621135331601, -10.09807621135331246 ) ) ;
#1845 = CARTESIAN_POINT ( 'NONE',  ( -111.1924547142390480, -298.2686324635848223, -286.3417390321903326 ) ) ;
#1846 = CARTESIAN_POINT ( 'NONE',  ( 23.82313755043268699, -280.1929156344815510, -230.1266894730004253 ) ) ;
#1847 = CARTESIAN_POINT ( 'NONE',  ( 32.17914147324426466, -279.9187893134987348, -298.5010047866445575 ) ) ;
#1848 = CARTESIAN_POINT ( 'NONE',  ( 38.44531723469279427, -292.9090891060177455, -283.1091178266061661 ) ) ;
#1849 = CARTESIAN_POINT ( 'NONE',  ( -93.67062233099235868, -271.4657820610185581, -222.3308699401059698 ) ) ;
#1850 = CARTESIAN_POINT ( 'NONE',  ( 34.27671884510021272, -273.8957331200357999, -290.7083564287921718 ) ) ;
#1851 = CARTESIAN_POINT ( 'NONE',  ( -94.31428307769847663, -297.2143428639839726, -316.8068356223033106 ) ) ;
#1852 = CARTESIAN_POINT ( 'NONE',  ( -96.46848757314708678, -271.7819539807804858, -221.9399898264381648 ) ) ;
#1853 = CARTESIAN_POINT ( 'NONE',  ( -109.8394696117295126, -295.0838166859329021, -247.4262068561842227 ) ) ;
#1854 = CARTESIAN_POINT ( 'NONE',  ( 17.53195956483178009, -295.6733726494643406, -319.4133392857546028 ) ) ;
#1855 = LINE ( 'NONE', #38761, #18792 ) ;
#1856 = CARTESIAN_POINT ( 'NONE',  ( 21.92953655819888681, -293.7560323184541176, -227.4501664748423764 ) ) ;
#1857 = CARTESIAN_POINT ( 'NONE',  ( 82.64890176555634582, -299.5541904835127980, -195.3611179825600175 ) ) ;
#1859 = CARTESIAN_POINT ( 'NONE',  ( -95.60433081934026234, -295.9340658417783061, -314.3642732270483293 ) ) ;
#1858 = CARTESIAN_POINT ( 'NONE',  ( -72.81592691475427159, -283.6051548763372807, -203.8203578936656868 ) ) ;
#1860 = CARTESIAN_POINT ( 'NONE',  ( -105.7841473901820422, -284.0961375919898728, -305.7567879993230804 ) ) ;
#1861 = CARTESIAN_POINT ( 'NONE',  ( 35.58859047254066610, -283.2195487465161818, -250.5513702828071132 ) ) ;
#1862 = CARTESIAN_POINT ( 'NONE',  ( -35.14458656851743257, -285.7457197627905430, -193.4004832215970282 ) ) ;
#1863 = CARTESIAN_POINT ( 'NONE',  ( -107.4187059640009920, -288.8953773174212643, -243.9608039593103967 ) ) ;
#1864 = CARTESIAN_POINT ( 'NONE',  ( -54.42813229853332757, -271.3380690714489560, -195.3538533559490702 ) ) ;
#1865 = CARTESIAN_POINT ( 'NONE',  ( -35.90716019710459506, -284.7553419901889242, -196.8819673709639062 ) ) ;
#1866 = CARTESIAN_POINT ( 'NONE',  ( -70.51784693657312175, -288.3996036156115110, -339.5191348611854210 ) ) ;
#1867 = DIRECTION ( 'NONE',  ( 1.000000000000000000, 0.000000000000000000, -0.000000000000000000 ) ) ;
#1868 = CARTESIAN_POINT ( 'NONE',  ( -109.0718056553745186, -297.9251130639506187, -287.7703970369654485 ) ) ;
#1869 = CARTESIAN_POINT ( 'NONE',  ( -113.1350557789254196, -280.1046753220382470, -260.2638623962227484 ) ) ;
#1871 = CARTESIAN_POINT ( 'NONE',  ( 4.938849726082819913, -280.3081393567618989, -210.8258965525135409 ) ) ;
#1870 = CARTESIAN_POINT ( 'NONE',  ( -36.32253863583939335, -293.0595834506718802, -345.7222541343576836 ) ) ;
#1872 = CARTESIAN_POINT ( 'NONE',  ( 23.17299005405337908, -294.3557628267265045, -317.9950054099700765 ) ) ;
#1873 = CARTESIAN_POINT ( 'NONE',  ( -112.9154323579523975, -282.6011897958714485, -272.7783060923707694 ) ) ;
#1874 = CARTESIAN_POINT ( 'NONE',  ( -112.3774048961945198, -280.5723370782346819, -268.8019203644975050 ) ) ;
#1875 = CARTESIAN_POINT ( 'NONE',  ( -28.88065716900909408, -294.0011428959697355, -343.1571866385416456 ) ) ;
#1876 = CIRCLE ( 'NONE', #32091, 1.000000000000000888 ) ;
#1877 = CARTESIAN_POINT ( 'NONE',  ( 72.74377771393429271, -297.4299603653872168, -195.3986477740726571 ) ) ;
#1878 = ORIENTED_EDGE ( 'NONE', *, *, #16109, .T. ) ;
#1879 = FACE_OUTER_BOUND ( 'NONE', #84407, .T. ) ;
#1881 = CARTESIAN_POINT ( 'NONE',  ( -2.401004102695674991, -282.4966363137678513, -204.3845538203418357 ) ) ;
#1880 = CIRCLE ( 'NONE', #15465, 1.897123461337413275 ) ;
#1882 = CARTESIAN_POINT ( 'NONE',  ( -108.3603156578023174, -295.8329766546326596, -287.5703708434563168 ) ) ;
#1883 = CARTESIAN_POINT ( 'NONE',  ( 175.2296996224750103, 275.0000000000000568, 0.000000000000000000 ) ) ;
#1884 = CARTESIAN_POINT ( 'NONE',  ( 10.59707575819633618, -279.9094976428775681, -330.5268031993606428 ) ) ;
#1885 = CARTESIAN_POINT ( 'NONE',  ( -78.74592237100219450, -272.7065600718952396, -205.6320734918893152 ) ) ;
#1886 = MECHANICAL_DESIGN_GEOMETRIC_PRESENTATION_REPRESENTATION (  '', ( #88040 ), #32101 ) ;
#1887 = CARTESIAN_POINT ( 'NONE',  ( 38.85778703060388040, -288.9535576762977485, -277.2121345951974263 ) ) ;
#1888 = CARTESIAN_POINT ( 'NONE',  ( -81.72736291092070360, -291.2620429128496085, -212.3410244009469068 ) ) ;
#1889 = AXIS2_PLACEMENT_3D ( 'NONE', #75536, #46175, #8792 ) ;
#1890 = CARTESIAN_POINT ( 'NONE',  ( -19.38416620746206576, -281.8073654388558111, -198.8364195858591756 ) ) ;
#1891 = CARTESIAN_POINT ( 'NONE',  ( -31.29424783336095217, -275.7299018712960219, -196.7965199544862571 ) ) ;
#1892 = ADVANCED_FACE ( 'NONE', ( #39254 ), #63083, .T. ) ;
#1893 = CARTESIAN_POINT ( 'NONE',  ( -68.67897335434874151, -278.4257154487294201, -203.9901468210984206 ) ) ;
#1894 = CARTESIAN_POINT ( 'NONE',  ( 19.84959410240758970, -278.2237576180907013, -318.8807688055062499 ) ) ;
#1895 = ORIENTED_EDGE ( 'NONE', *, *, #3875, .T. ) ;
#1896 = CARTESIAN_POINT ( 'NONE',  ( 20.03728855721349689, -274.6883701056705718, -218.9344227371128113 ) ) ;
#1897 = CARTESIAN_POINT ( 'NONE',  ( -90.86842919715634537, -293.2053341827048598, -218.6290827174546223 ) ) ;
#1898 = DIRECTION ( 'NONE',  ( -1.000000000000000000, -0.000000000000000000, -0.000000000000000000 ) ) ;
#1899 = EDGE_CURVE ( 'NONE', #23580, #14315, #57008, .T. ) ;
#1900 = DIRECTION ( 'NONE',  ( -1.000000000000000000, -0.000000000000000000, -0.000000000000000000 ) ) ;
#1901 = CARTESIAN_POINT ( 'NONE',  ( 14.60873643673612676, -290.9132248203426911, -215.1396494589304211 ) ) ;
#1902 = CARTESIAN_POINT ( 'NONE',  ( -65.57697277464507124, -297.3391754524017756, -203.0197720991061487 ) ) ;
#1903 = DIRECTION ( 'NONE',  ( 0.000000000000000000, 0.000000000000000000, 1.000000000000000000 ) ) ;
#1904 = CARTESIAN_POINT ( 'NONE',  ( -6.187879255811044032, -293.9742057759335125, -200.6896045566093107 ) ) ;
#1905 = CARTESIAN_POINT ( 'NONE',  ( -20.25526795762937127, -276.7662352645559167, -195.3538533559490702 ) ) ;
#1906 = CARTESIAN_POINT ( 'NONE',  ( 35.78217053628306843, -289.3476537067894014, -254.4574086725481834 ) ) ;
#1907 = CARTESIAN_POINT ( 'NONE',  ( 20.58495107737903496, -274.2066185441614721, -317.7577882374013143 ) ) ;
#1908 = CARTESIAN_POINT ( 'NONE',  ( 26.49844309758927707, -276.9546802578913116, -231.9762101116281769 ) ) ;
#1909 = CARTESIAN_POINT ( 'NONE',  ( 19.59345793328936480, -290.9639099877106787, -222.4059099524203589 ) ) ;
#1910 = CARTESIAN_POINT ( 'NONE',  ( -45.16969867192311483, -281.8145663304621849, -194.9496519062343225 ) ) ;
#1911 = VERTEX_POINT ( 'NONE', #48237 ) ;
#1912 = CARTESIAN_POINT ( 'NONE',  ( -67.83443920917248704, -282.8118873294255309, -336.7997026443087520 ) ) ;
#1913 = CARTESIAN_POINT ( 'NONE',  ( -71.42108493270252723, -278.5713655525021295, -339.0640148827815210 ) ) ;
#1914 = CARTESIAN_POINT ( 'NONE',  ( -38.74076183257472650, -281.8642647045426770, -346.9512697412765192 ) ) ;
#1915 = CARTESIAN_POINT ( 'NONE',  ( -48.44806128341126339, -278.1313398783293565, -346.3718670637045420 ) ) ;
#1916 = CARTESIAN_POINT ( 'NONE',  ( 39.01381927215583545, -277.0821662604436710, -271.1450238814580302 ) ) ;
#1917 = CARTESIAN_POINT ( 'NONE',  ( -21.39648532958013050, -294.7662352645559736, -200.3538533559491555 ) ) ;
#1918 = EDGE_LOOP ( 'NONE', ( #64552, #5227, #88401, #55731 ) ) ;
#1919 = CARTESIAN_POINT ( 'NONE',  ( -103.2120358628387038, -298.0758436231525366, -306.2233476429284451 ) ) ;
#1920 = CARTESIAN_POINT ( 'NONE',  ( -53.46318296759645250, -290.3435385386808321, -341.8756190553006604 ) ) ;
#1921 = CARTESIAN_POINT ( 'NONE',  ( -103.3223180562658854, -276.1072893575904459, -305.2667745100243906 ) ) ;
#1922 = CARTESIAN_POINT ( 'NONE',  ( -97.34544202693207637, -291.6813317710332285, -316.9821966407765217 ) ) ;
#1923 = CARTESIAN_POINT ( 'NONE',  ( -52.38265163569526095, -291.2031314741498704, -198.7713067025153748 ) ) ;
#1924 = CARTESIAN_POINT ( 'NONE',  ( 0.6834181077674537086, -288.0672774831495531, -337.3064253655680318 ) ) ;
#1925 = DIRECTION ( 'NONE',  ( 1.000000000000000000, 0.000000000000000000, 0.000000000000000000 ) ) ;
#1926 = CARTESIAN_POINT ( 'NONE',  ( -92.27400092603585335, -282.2541756316520605, -319.6638362964998805 ) ) ;
#1927 = CARTESIAN_POINT ( 'NONE',  ( -111.6040573325567635, -292.4373244364466586, -268.4532604835364396 ) ) ;
#1928 = CARTESIAN_POINT ( 'NONE',  ( -99.62730959340170500, -282.4917718055924070, -309.8420990877393706 ) ) ;
#1929 = CARTESIAN_POINT ( 'NONE',  ( 24.08557108479768516, -282.3105806660759072, -229.9217102993035837 ) ) ;
#1930 = CARTESIAN_POINT ( 'NONE',  ( -96.20289959529432622, -290.8279826483581019, -319.6580630310674564 ) ) ;
#1931 = CARTESIAN_POINT ( 'NONE',  ( -100.8684032164926094, -279.5383306389525160, -234.2730806816644531 ) ) ;
#1932 = CARTESIAN_POINT ( 'NONE',  ( -42.01433136976206129, -290.7894136091798600, -193.9008326300244391 ) ) ;
#1933 = CARTESIAN_POINT ( 'NONE',  ( 0.1959575774732144893, -287.3416398683646094, -203.3007221444231334 ) ) ;
#1934 = CARTESIAN_POINT ( 'NONE',  ( 36.32828523687043543, -288.3237080016547793, -292.5938250956721163 ) ) ;
#1935 = CARTESIAN_POINT ( 'NONE',  ( -109.6125242434319631, -284.8546033590928914, -260.0689857353383445 ) ) ;
#1936 = ORIENTED_EDGE ( 'NONE', *, *, #63556, .T. ) ;
#1937 = DIRECTION ( 'NONE',  ( -1.000000000000000000, 0.000000000000000000, 0.000000000000000000 ) ) ;
#1938 = CARTESIAN_POINT ( 'NONE',  ( 37.10702458874491327, -295.2338532478886464, -256.3007883043370612 ) ) ;
#1939 = CARTESIAN_POINT ( 'NONE',  ( 8.596599729177000881, -293.1221787080729086, -331.5409420889323542 ) ) ;
#1940 = CARTESIAN_POINT ( 'NONE',  ( -37.82329950544600905, -276.1170400994602119, -343.6073223787289521 ) ) ;
#1941 = CARTESIAN_POINT ( 'NONE',  ( -107.6764350356030349, -296.2993689792376131, -239.1435218707934496 ) ) ;
#1942 = CARTESIAN_POINT ( 'NONE',  ( 31.22360272392403147, -292.3914795338272370, -297.5100297038638928 ) ) ;
#1943 = CARTESIAN_POINT ( 'NONE',  ( -68.45332359307698766, -295.8775789098493192, -203.1904272105183225 ) ) ;
#1944 = AXIS2_PLACEMENT_3D ( 'NONE', #34809, #13512, #28646 ) ;
#1945 = CARTESIAN_POINT ( 'NONE',  ( -3.466565670280920664, -293.7149322609615183, -205.2488628282713705 ) ) ;
#1946 = CARTESIAN_POINT ( 'NONE',  ( 30.13490306836979471, -294.2471641990571811, -241.5758669598086215 ) ) ;
#1947 = CARTESIAN_POINT ( 'NONE',  ( 208.4306832106270804, -199.2391364535880882, 0.000000000000000000 ) ) ;
#1948 = AXIS2_PLACEMENT_3D ( 'NONE', #59364, #23828, #23372 ) ;
#1949 = CARTESIAN_POINT ( 'NONE',  ( -9.101046344283929557, -292.6837187558634810, -340.0760895588767880 ) ) ;
#1950 = CARTESIAN_POINT ( 'NONE',  ( -82.28888259837283670, -299.4394134775402563, -210.2575296171674495 ) ) ;
#1951 = CARTESIAN_POINT ( 'NONE',  ( 33.31208926155937178, -288.7494412400940291, -289.8224719517164090 ) ) ;
#1952 = EDGE_CURVE ( 'NONE', #64179, #15573, #34061, .T. ) ;
#1953 = CIRCLE ( 'NONE', #71531, 5.000000000000000888 ) ;
#1954 = EDGE_CURVE ( 'NONE', #44950, #76130, #84195, .T. ) ;
#1955 = AXIS2_PLACEMENT_3D ( 'NONE', #93178, #10133, #31007 ) ;
#1956 = CARTESIAN_POINT ( 'NONE',  ( 15.81326990028412283, -278.2842661999981146, -323.8470756747084351 ) ) ;
#1957 = CARTESIAN_POINT ( 'NONE',  ( -67.15474507633625478, -278.3541955935785381, -199.9020474208194855 ) ) ;
#1958 = PRODUCT ( 'Metal Foot Protection Guard', 'Metal Foot Protection Guard', '', ( #38817 ) ) ;
#1959 = CARTESIAN_POINT ( 'NONE',  ( -106.7476530637889169, -272.3257423396635772, -237.2533170384528773 ) ) ;
#1960 = CARTESIAN_POINT ( 'NONE',  ( -5.437532595103494515, -280.7090473537692219, -337.6316490276136619 ) ) ;
#1961 = CARTESIAN_POINT ( 'NONE',  ( -72.12328436148176536, -277.9998443741489496, -202.5477870108646528 ) ) ;
#1962 = VECTOR ( 'NONE', #90749, 1000.000000000000000 ) ;
#1963 = CARTESIAN_POINT ( 'NONE',  ( -109.6302219920987540, -295.0624182200518817, -283.6828267874411154 ) ) ;
#1964 = CARTESIAN_POINT ( 'NONE',  ( -87.02632044705406145, -275.3610118057939076, -214.1103711793309969 ) ) ;
#1965 = CARTESIAN_POINT ( 'NONE',  ( -31.33959885877072438, -274.7813397628189591, -197.4933380385196529 ) ) ;
#1966 = DIRECTION ( 'NONE',  ( -0.000000000000000000, -1.000000000000000000, -0.000000000000000000 ) ) ;
#1967 = CARTESIAN_POINT ( 'NONE',  ( -101.7956337022391722, -289.0941016233005598, -231.2208794897481425 ) ) ;
#1968 = CARTESIAN_POINT ( 'NONE',  ( -75.66368098456607072, -289.5489432952361994, -337.1475371352232173 ) ) ;
#1969 = CARTESIAN_POINT ( 'NONE',  ( -46.67911778174227777, -275.9340286220564167, -195.7766621180727498 ) ) ;
#1970 = CARTESIAN_POINT ( 'NONE',  ( -96.72882652426994810, -295.1771302697427473, -224.8078669088284016 ) ) ;
#1971 = CARTESIAN_POINT ( 'NONE',  ( -4.242673219856334832, -281.8240457468197633, -339.7197407501331554 ) ) ;
#1972 = CARTESIAN_POINT ( 'NONE',  ( 165.2494399300530290, 8.542400036368780647, 10.00000000000000000 ) ) ;
#1973 = CARTESIAN_POINT ( 'NONE',  ( 22.03161527036013112, -280.1801386287440323, -316.2054480051863266 ) ) ;
#1974 = TOROIDAL_SURFACE ( 'NONE', #45753, 2.000000000000000000, 1.000000000000000000 ) ;
#1975 = DIRECTION ( 'NONE',  ( 0.000000000000000000, 0.000000000000000000, 1.000000000000000000 ) ) ;
#1976 = CARTESIAN_POINT ( 'NONE',  ( -107.7720124723185933, -289.6194163490811775, -249.6597668280071503 ) ) ;
#1977 = CARTESIAN_POINT ( 'NONE',  ( -35.88588397217707637, -284.2101882754647022, -196.1401904582852751 ) ) ;
#1978 = CARTESIAN_POINT ( 'NONE',  ( 158.6539576904058606, 276.0000000000000568, -11.60392986742922439 ) ) ;
#1979 = CARTESIAN_POINT ( 'NONE',  ( 219.8344101925596021, 3.000000000000000000, -9.000000000000001776 ) ) ;
#1980 = CARTESIAN_POINT ( 'NONE',  ( 37.70920793677652938, -291.5575744195288621, -270.7962710752898943 ) ) ;
#1981 = CARTESIAN_POINT ( 'NONE',  ( -36.43613440273270498, -278.6407826863052151, -344.1681683069380142 ) ) ;
#1982 = CARTESIAN_POINT ( 'NONE',  ( -0.5525842283535833399, -283.7795395071905205, -337.5665288592011279 ) ) ;
#1984 = CARTESIAN_POINT ( 'NONE',  ( -39.97391833633340497, -286.0181600753365387, -197.4085893951001367 ) ) ;
#1983 = CARTESIAN_POINT ( 'NONE',  ( 22.50752180093631338, -273.0045209359668661, -224.2164673674942890 ) ) ;
#1985 = CARTESIAN_POINT ( 'NONE',  ( 17.88938769955537111, -277.6664278175513800, -319.0103906305160422 ) ) ;
#1986 = CARTESIAN_POINT ( 'NONE',  ( -43.20987102546752112, -277.9309823070757375, -343.2868767880636938 ) ) ;
#1987 = CARTESIAN_POINT ( 'NONE',  ( -80.39215963328472014, -285.6351848317096369, -331.8381158696838042 ) ) ;
#1988 = VERTEX_POINT ( 'NONE', #39717 ) ;
#1989 = DIRECTION ( 'NONE',  ( 0.01273136352371030157, 0.9999189529070979798, 0.000000000000000000 ) ) ;
#1990 = CARTESIAN_POINT ( 'NONE',  ( -86.39694989274904913, -295.5451879507772901, -329.7124656927044839 ) ) ;
#1991 = CARTESIAN_POINT ( 'NONE',  ( -3.879320491256792902, -288.4757104310828595, -203.6369397903436038 ) ) ;
#1992 = DIRECTION ( 'NONE',  ( -0.000000000000000000, -1.000000000000000000, -0.000000000000000000 ) ) ;
#1993 = CARTESIAN_POINT ( 'NONE',  ( -88.52914483777347243, -287.1952119285918457, -334.4957818155094174 ) ) ;
#1994 = CARTESIAN_POINT ( 'NONE',  ( -111.7825392023984250, -277.7047219313773212, -251.8667266803492168 ) ) ;
#1995 = CARTESIAN_POINT ( 'NONE',  ( -101.0042560621475900, -289.5093916096729458, -228.3914229997147629 ) ) ;
#1996 = CARTESIAN_POINT ( 'NONE',  ( -81.91315779100871453, -286.9522013627462229, -211.6747233722719557 ) ) ;
#1997 = CARTESIAN_POINT ( 'NONE',  ( -110.6283986156055335, -280.4515435532562719, -259.6590341996831057 ) ) ;
#1998 = CARTESIAN_POINT ( 'NONE',  ( 17.91276743108515745, -288.2493991783006209, -217.5065192596706538 ) ) ;
#1999 = CARTESIAN_POINT ( 'NONE',  ( -3.913476057354651427, -284.6113574538759394, -337.4994415272765309 ) ) ;
#2000 = CARTESIAN_POINT ( 'NONE',  ( -11.86418208911024053, -276.8962747227436125, -343.0799387615849128 ) ) ;
#2001 = CARTESIAN_POINT ( 'NONE',  ( -107.1166455203094472, -270.9062053245839934, -243.1723182243472365 ) ) ;
#2002 = CARTESIAN_POINT ( 'NONE',  ( -42.42793438594448219, -279.8229892678264719, -193.5292871727605757 ) ) ;
#2004 = CARTESIAN_POINT ( 'NONE',  ( -44.73598588289178224, -299.8781409322182867, -196.2378934212745207 ) ) ;
#2003 = AXIS2_PLACEMENT_3D ( 'NONE', #71866, #337, #86031 ) ;
#2005 = CARTESIAN_POINT ( 'NONE',  ( 156.3466120839441089, 16.19322481500840993, 7.221609175748572973 ) ) ;
#2006 = CARTESIAN_POINT ( 'NONE',  ( -4.829096099716510437, -282.9805209788416391, -202.7746430608542312 ) ) ;
#2007 = CARTESIAN_POINT ( 'NONE',  ( 19.29575570832072273, -273.0951662187703732, -219.6263609375178589 ) ) ;
#2009 = VECTOR ( 'NONE', #39902, 1000.000000000000000 ) ;
#2008 = DIRECTION ( 'NONE',  ( -1.000000000000000000, -0.000000000000000000, -0.000000000000000000 ) ) ;
#2010 = CARTESIAN_POINT ( 'NONE',  ( -61.81634175569918455, -276.8865265792036894, -339.2551582312770506 ) ) ;
#2011 = AXIS2_PLACEMENT_3D ( 'NONE', #16154, #66807, #89023 ) ;
#2012 = CARTESIAN_POINT ( 'NONE',  ( -41.18826645213862037, -275.2099551193472848, -193.8028367402565095 ) ) ;
#2013 = CARTESIAN_POINT ( 'NONE',  ( -4.276076615609534670, -281.6856487468970727, -339.6538752760456532 ) ) ;
#2014 = CARTESIAN_POINT ( 'NONE',  ( -42.71541642840033148, -290.8808796353594630, -344.2304245617198717 ) ) ;
#2015 = CARTESIAN_POINT ( 'NONE',  ( -95.05948908248903706, -298.7532897346009690, -220.3686610771193841 ) ) ;
#2016 = CARTESIAN_POINT ( 'NONE',  ( -100.4323919280489008, -298.3340155440513968, -226.8918481742781523 ) ) ;
#2017 = CARTESIAN_POINT ( 'NONE',  ( 0.8226664419661585681, -294.5626779565457127, -205.9910197163725343 ) ) ;
#2018 = CARTESIAN_POINT ( 'NONE',  ( 27.12578989863462553, -280.0623675370210890, -308.4630762548672465 ) ) ;
#2019 = AXIS2_PLACEMENT_3D ( 'NONE', #11166, #32490, #12101 ) ;
#2020 = CARTESIAN_POINT ( 'NONE',  ( 20.78542030481310121, -282.8279840764689084, -223.8578700069980414 ) ) ;
#2021 = CARTESIAN_POINT ( 'NONE',  ( -67.70395980963517957, -271.6718903748085836, -202.1563572596103029 ) ) ;
#2022 = CARTESIAN_POINT ( 'NONE',  ( -81.08546537373352692, -285.2352171238882192, -332.8185952326336974 ) ) ;
#2023 = EDGE_CURVE ( 'NONE', #3915, #44324, #61085, .T. ) ;
#2024 = CARTESIAN_POINT ( 'NONE',  ( -71.32822682572701467, -288.4322730365837515, -335.3302249025298920 ) ) ;
#2025 = CARTESIAN_POINT ( 'NONE',  ( 201.1547583153258358, 288.4971606646042233, -97.45162841053168279 ) ) ;
#2026 = ORIENTED_EDGE ( 'NONE', *, *, #60434, .F. ) ;
#2027 = CARTESIAN_POINT ( 'NONE',  ( -4.602114273523942423, -287.2039942887722077, -339.4169636361654057 ) ) ;
#2028 = CARTESIAN_POINT ( 'NONE',  ( 12.16702034026408263, -288.0074480611583567, -324.1045288833065570 ) ) ;
#2029 = ORIENTED_EDGE ( 'NONE', *, *, #54431, .F. ) ;
#2030 = CARTESIAN_POINT ( 'NONE',  ( -107.9371932011896575, -285.2473543258305995, -300.4597063634721508 ) ) ;
#2031 = VECTOR ( 'NONE', #28536, 1000.000000000000227 ) ;
#2032 = CARTESIAN_POINT ( 'NONE',  ( 25.29178249154562153, -275.3680629837697325, -232.7247502308229912 ) ) ;
#2033 = CARTESIAN_POINT ( 'NONE',  ( -42.02130980168755059, -290.9147976919833809, -193.8131345778098193 ) ) ;
#2034 = CARTESIAN_POINT ( 'NONE',  ( 6.873188760179909096, -283.1195543310718108, -333.3417071995940546 ) ) ;
#2035 = CARTESIAN_POINT ( 'NONE',  ( 37.74681026919502358, -283.2445694927249065, -284.0140511247211634 ) ) ;
#2036 = CARTESIAN_POINT ( 'NONE',  ( -90.42048600183871088, -284.1120019392710674, -326.1871110726198140 ) ) ;
#2037 = CARTESIAN_POINT ( 'NONE',  ( -57.11321054484388782, -279.7898631630807245, -200.0895919151701605 ) ) ;
#2038 = CARTESIAN_POINT ( 'NONE',  ( 10.64812456238590777, -272.1952119285918457, -210.2361428286349110 ) ) ;
#2039 = CARTESIAN_POINT ( 'NONE',  ( -95.22016405621698709, -240.3877380467951639, -341.9231918056108270 ) ) ;
#2040 = ORIENTED_EDGE ( 'NONE', *, *, #56462, .T. ) ;
#2041 = CARTESIAN_POINT ( 'NONE',  ( 37.20209665873868943, -277.4604354044789147, -263.2211078531785802 ) ) ;
#2042 = CARTESIAN_POINT ( 'NONE',  ( 138.0606683641728409, 180.7651495054645920, -241.0585848927976258 ) ) ;
#2043 = AXIS2_PLACEMENT_3D ( 'NONE', #53323, #2683, #31562 ) ;
#2044 = CARTESIAN_POINT ( 'NONE',  ( -94.52587752461543857, -296.5429601974807383, -224.8214372187032382 ) ) ;
#2045 = CARTESIAN_POINT ( 'NONE',  ( 21.26764366597424072, -292.3870628483946348, -220.4965133666736676 ) ) ;
#2046 = CARTESIAN_POINT ( 'NONE',  ( 180.0836269057962795, 251.0244910124412172, -164.3671539780329454 ) ) ;
#2048 = CARTESIAN_POINT ( 'NONE',  ( -110.5859630443777775, -288.8340604813959089, -279.4009390329691200 ) ) ;
#2047 = CARTESIAN_POINT ( 'NONE',  ( -93.21936848272368081, -295.8435837508641271, -218.1658974459102183 ) ) ;
#2049 = CARTESIAN_POINT ( 'NONE',  ( -96.57585051210328686, -297.7941808949692017, -315.1277865623907815 ) ) ;
#2050 = CARTESIAN_POINT ( 'NONE',  ( 13.46848417807374254, -288.0963321584071650, -217.1913126699191992 ) ) ;
#2051 = ORIENTED_EDGE ( 'NONE', *, *, #5681, .F. ) ;
#2052 = CARTESIAN_POINT ( 'NONE',  ( 17.40218351614037573, -295.2351209530521601, -324.2505576784660093 ) ) ;
#2053 = CARTESIAN_POINT ( 'NONE',  ( -78.40604531219229045, -284.1139214789589573, -330.7904816738076192 ) ) ;
#2054 = CARTESIAN_POINT ( 'NONE',  ( -114.0325882487032914, -271.4726545306050980, -270.3474016006499596 ) ) ;
#2055 = VECTOR ( 'NONE', #50209, 1000.000000000000000 ) ;
#2056 = CARTESIAN_POINT ( 'NONE',  ( 11.00922700175544833, -293.5044262244004472, -210.5737734599591988 ) ) ;
#2057 = CARTESIAN_POINT ( 'NONE',  ( 37.02148816262170072, -293.7965949533668777, -250.5709245253850384 ) ) ;
#2058 = CARTESIAN_POINT ( 'NONE',  ( -49.69081312820068774, -292.0570746453730635, -198.3618984261759408 ) ) ;
#2059 = ORIENTED_EDGE ( 'NONE', *, *, #38620, .T. ) ;
#2060 = CARTESIAN_POINT ( 'NONE',  ( 157.4471379844591752, 15.78783268421836183, 9.037979834337678042 ) ) ;
#2061 = CARTESIAN_POINT ( 'NONE',  ( -26.45528139451065286, -300.0474666281319855, -194.5929036537726518 ) ) ;
#2062 = CARTESIAN_POINT ( 'NONE',  ( -15.87385002818944280, -273.1186214841131346, -196.7728019898977152 ) ) ;
#2063 = VERTEX_POINT ( 'NONE', #61546 ) ;
#2064 = CARTESIAN_POINT ( 'NONE',  ( -54.12393806463698809, -276.7696001028011210, -345.5015556906572556 ) ) ;
#2065 = CARTESIAN_POINT ( 'NONE',  ( -93.50954456418412519, -271.6257690309754480, -222.4708157400283142 ) ) ;
#2066 = CARTESIAN_POINT ( 'NONE',  ( -109.3648041150566570, -280.1785363210345281, -288.4006138067650795 ) ) ;
#2067 = CARTESIAN_POINT ( 'NONE',  ( -73.46341564798592572, -275.6762773280892702, -335.2300986960959790 ) ) ;
#2068 = CARTESIAN_POINT ( 'NONE',  ( -101.5694060139669546, -298.2401026749955122, -234.8374315116672335 ) ) ;
#2069 = CARTESIAN_POINT ( 'NONE',  ( -110.5774403763021212, -273.5291849198071645, -267.6404355218357409 ) ) ;
#2070 = CARTESIAN_POINT ( 'NONE',  ( -33.40664285205567552, -299.7007609888386810, -194.1600618764771582 ) ) ;
#2071 = CARTESIAN_POINT ( 'NONE',  ( 8.529493450450990721, -272.6970729445243933, -210.5761667032649882 ) ) ;
#2072 = CARTESIAN_POINT ( 'NONE',  ( 33.87661159185390858, -294.4214209168420666, -286.9040071116637591 ) ) ;
#2073 = CARTESIAN_POINT ( 'NONE',  ( -68.03050189274372883, -290.2158688182970536, -203.4625054185326576 ) ) ;
#2074 = DIRECTION ( 'NONE',  ( -1.000000000000000000, -0.000000000000000000, -0.000000000000000000 ) ) ;
#2075 = CARTESIAN_POINT ( 'NONE',  ( -48.47887736332177866, -277.6825073734515286, -346.5430856636735939 ) ) ;
#2076 = EDGE_CURVE ( 'NONE', #44526, #16441, #7114, .T. ) ;
#2077 = CARTESIAN_POINT ( 'NONE',  ( -24.59852022289694062, -274.3858610515175656, -198.4303855360653301 ) ) ;
#2078 = CARTESIAN_POINT ( 'NONE',  ( -112.9971824448755200, -283.3846358296967765, -258.6304402422449584 ) ) ;
#2079 = CARTESIAN_POINT ( 'NONE',  ( -98.50159136657043746, -297.9583063324445789, -314.1465297772388112 ) ) ;
#2080 = CARTESIAN_POINT ( 'NONE',  ( 207.8229135343381131, 36.37371623600424186, 14.86900317285956064 ) ) ;
#2081 = CIRCLE ( 'NONE', #86680, 1.000000000000000888 ) ;
#2082 = CARTESIAN_POINT ( 'NONE',  ( 11.24892245177460737, -285.9427870572646384, -215.5979501576665598 ) ) ;
#2083 = CARTESIAN_POINT ( 'NONE',  ( -34.57263458211485130, -281.0172621161066786, -345.4767668524411874 ) ) ;
#2084 = CARTESIAN_POINT ( 'NONE',  ( -36.47651045864730435, -275.2810569442526116, -344.3820383394859164 ) ) ;
#2085 = CARTESIAN_POINT ( 'NONE',  ( -35.11786842070824832, -275.5984073651620747, -343.9167397327077538 ) ) ;
#2086 = CARTESIAN_POINT ( 'NONE',  ( 30.10818696972672370, -283.9858643997600893, -303.2733891445327004 ) ) ;
#2087 = CARTESIAN_POINT ( 'NONE',  ( 35.41208883775818350, -276.6300157962704134, -260.6648972799100648 ) ) ;
#2088 = DIRECTION ( 'NONE',  ( 0.000000000000000000, 1.000000000000000000, 0.000000000000000000 ) ) ;
#2089 = CARTESIAN_POINT ( 'NONE',  ( -106.1123779067414006, -271.3771798491576988, -237.5429173728900878 ) ) ;
#2090 = AXIS2_PLACEMENT_3D ( 'NONE', #30133, #58563, #59492 ) ;
#2091 = CARTESIAN_POINT ( 'NONE',  ( -9.562898643533312537, -282.4144454992721194, -200.5158130911784440 ) ) ;
#2092 = LINE ( 'NONE', #15363, #46809 ) ;
#2093 = CARTESIAN_POINT ( 'NONE',  ( 19.19276175889717351, -288.7795142148936520, -220.1523971396397314 ) ) ;
#2094 = DIRECTION ( 'NONE',  ( 0.000000000000000000, 0.000000000000000000, 1.000000000000000000 ) ) ;
#2095 = CARTESIAN_POINT ( 'NONE',  ( -107.6956553187080630, -288.8909507053044763, -244.2265189771908354 ) ) ;
#2096 = FACE_OUTER_BOUND ( 'NONE', #81756, .T. ) ;
#2097 = CARTESIAN_POINT ( 'NONE',  ( -90.32191148886263932, -296.0768748765642044, -219.4924588635598468 ) ) ;
#2098 = CARTESIAN_POINT ( 'NONE',  ( -102.1913712050967149, -289.1788048894101735, -234.1254742418522596 ) ) ;
#2099 = CARTESIAN_POINT ( 'NONE',  ( -107.5887910744927609, -275.4946769126667618, -270.3985833712262092 ) ) ;
#2100 = CARTESIAN_POINT ( 'NONE',  ( 54.76408350478209996, -297.2049266773145177, -195.3925142569238744 ) ) ;
#2101 = CARTESIAN_POINT ( 'NONE',  ( 19.09826794285438822, -286.7365292651955997, -321.7346180336016346 ) ) ;
#2102 = CARTESIAN_POINT ( 'NONE',  ( -21.95339105724425011, -281.0974418033774782, -344.7733075435555747 ) ) ;
#2103 = CARTESIAN_POINT ( 'NONE',  ( -92.55649793336425546, -291.2325886586795036, -222.6083578181284395 ) ) ;
#2104 = VECTOR ( 'NONE', #19329, 1000.000000000000000 ) ;
#2105 = CIRCLE ( 'NONE', #32385, 1.897123461337413275 ) ;
#2106 = CARTESIAN_POINT ( 'NONE',  ( 34.63776245489370353, -282.7763513045014179, -254.9932462029766498 ) ) ;
#2107 = CARTESIAN_POINT ( 'NONE',  ( -13.46703237403166042, -283.5370432515453558, -339.5712027365387371 ) ) ;
#2108 = CARTESIAN_POINT ( 'NONE',  ( -64.82316766814668085, -291.3890356585741870, -340.5815942037149853 ) ) ;
#2109 = CARTESIAN_POINT ( 'NONE',  ( -110.0832714527496279, -273.2030633494566700, -245.1736589463104679 ) ) ;
#2110 = AXIS2_PLACEMENT_3D ( 'NONE', #15492, #87900, #51930 ) ;
#2111 = CARTESIAN_POINT ( 'NONE',  ( -6.241949309262166068, -286.7265899512405554, -339.2241683085647423 ) ) ;
#2112 = CARTESIAN_POINT ( 'NONE',  ( 37.63491125693305150, -275.3321891305067197, -252.7678633170977207 ) ) ;
#2113 = CARTESIAN_POINT ( 'NONE',  ( -84.89585910391330970, -293.3723453931884251, -212.8246185782433315 ) ) ;
#2114 = CYLINDRICAL_SURFACE ( 'NONE', #34879, 3.000000000000000888 ) ;
#2115 = CARTESIAN_POINT ( 'NONE',  ( -54.42813229853333468, -279.7662352645560304, -345.3683826091709648 ) ) ;
#2116 = CARTESIAN_POINT ( 'NONE',  ( -51.00496992666680995, -275.2262152499130821, -344.2755514994900068 ) ) ;
#2117 = CARTESIAN_POINT ( 'NONE',  ( 170.4537599243631405, 250.0000000000000568, -23.51999999999999602 ) ) ;
#2118 = CARTESIAN_POINT ( 'NONE',  ( -67.83836636071875148, -296.0585325629652971, -200.4737381892856831 ) ) ;
#2119 = CARTESIAN_POINT ( 'NONE',  ( -99.36258011767341713, -272.4340756826957204, -231.6661168403955742 ) ) ;
#2120 = CARTESIAN_POINT ( 'NONE',  ( -70.55032696535013770, -293.1261357774674252, -204.5743802770932689 ) ) ;
#2121 = VECTOR ( 'NONE', #87459, 1000.000000000000000 ) ;
#2122 = CARTESIAN_POINT ( 'NONE',  ( -105.9352276611975725, -291.8363160362087001, -244.5590881221161226 ) ) ;
#2123 = CARTESIAN_POINT ( 'NONE',  ( -92.40412902279267371, -285.6139025892744598, -319.8382743476557266 ) ) ;
#2124 = CARTESIAN_POINT ( 'NONE',  ( 37.21304882180386642, -295.1891219558214630, -287.1592840552299890 ) ) ;
#2125 = CARTESIAN_POINT ( 'NONE',  ( 30.45410925536853242, -294.4056411055672697, -234.7925460162518050 ) ) ;
#2126 = CARTESIAN_POINT ( 'NONE',  ( 17.97104195241555757, -294.0641211834099522, -318.0194522114629194 ) ) ;
#2127 = CARTESIAN_POINT ( 'NONE',  ( 37.63039947879230596, -289.5968253745170955, -273.8275428787123928 ) ) ;
#2128 = CARTESIAN_POINT ( 'NONE',  ( 9.210491383358622386, -282.5990530749176628, -331.6953944514881414 ) ) ;
#2129 = CARTESIAN_POINT ( 'NONE',  ( -15.30887110482980340, -296.4057675595481101, -194.8082513318286146 ) ) ;
#2130 = CARTESIAN_POINT ( 'NONE',  ( -80.93645673547408137, -285.3117699972636956, -206.8263170742234536 ) ) ;
#2131 = CARTESIAN_POINT ( 'NONE',  ( 6.380162456785919645, -278.4353498808865766, -330.9249243190263883 ) ) ;
#2132 = CARTESIAN_POINT ( 'NONE',  ( -110.7057658001759819, -283.3759472869606384, -268.1601246309364797 ) ) ;
#2133 = CARTESIAN_POINT ( 'NONE',  ( 37.35323648695389664, -285.6387572774202681, -277.1188610237232979 ) ) ;
#2134 = CARTESIAN_POINT ( 'NONE',  ( -92.16335732991835528, -277.4191286299256376, -217.9899962859443860 ) ) ;
#2135 = DIRECTION ( 'NONE',  ( 0.000000000000000000, 1.000000000000000000, -0.000000000000000000 ) ) ;
#2136 = CARTESIAN_POINT ( 'NONE',  ( -85.76224650306876640, -284.8681506636110612, -215.5811734984633290 ) ) ;
#2137 = CARTESIAN_POINT ( 'NONE',  ( -38.18102986284067413, -281.2469223001485830, -193.7627874137964454 ) ) ;
#2138 = CARTESIAN_POINT ( 'NONE',  ( 37.27287069503110217, -286.8378896028766007, -288.4578431553505311 ) ) ;
#2139 = CARTESIAN_POINT ( 'NONE',  ( -5.079819362040934649, -296.3816686781034377, -336.9870216331694905 ) ) ;
#2140 = CARTESIAN_POINT ( 'NONE',  ( -62.12632313572955667, -278.9691406889381255, -342.4734999533521886 ) ) ;
#2141 = CARTESIAN_POINT ( 'NONE',  ( -97.53050330547524993, -279.2318537549370490, -317.5904123559145091 ) ) ;
#2142 = CARTESIAN_POINT ( 'NONE',  ( -101.8579128402041647, -277.9202096510903743, -304.5174980859699190 ) ) ;
#2143 = CARTESIAN_POINT ( 'NONE',  ( -95.04310408981875469, -299.2114048706596350, -222.6906102932771887 ) ) ;
#2144 = CARTESIAN_POINT ( 'NONE',  ( -19.35104256547869639, -284.2839792348823380, -197.7225286248480813 ) ) ;
#2145 = CARTESIAN_POINT ( 'NONE',  ( -112.3877150568496290, -292.3192350521095477, -257.1499083572876430 ) ) ;
#2146 = CARTESIAN_POINT ( 'NONE',  ( 14.52530201901463691, -293.2218347199890331, -322.2402020043435300 ) ) ;
#2147 = ORIENTED_EDGE ( 'NONE', *, *, #33369, .F. ) ;
#2148 = CARTESIAN_POINT ( 'NONE',  ( 33.13599404509604796, -293.4717298116592588, -289.5131541331921881 ) ) ;
#2149 = CARTESIAN_POINT ( 'NONE',  ( -112.8699938290462654, -291.7988621492231687, -257.0581348260722052 ) ) ;
#2150 = CARTESIAN_POINT ( 'NONE',  ( -74.56482774962780979, -280.1945662622522946, -207.3876600772935888 ) ) ;
#2151 = CARTESIAN_POINT ( 'NONE',  ( -97.62083320307297640, -272.2486007453424577, -222.8295881325881851 ) ) ;
#2152 = CARTESIAN_POINT ( 'NONE',  ( 36.68853772482916042, -288.4651707061570391, -291.2141542374308187 ) ) ;
#2153 = CARTESIAN_POINT ( 'NONE',  ( 25.83678602795502854, -288.4678089045153797, -314.4324517823617384 ) ) ;
#2154 = CARTESIAN_POINT ( 'NONE',  ( 0.1758841609052546329, -286.8995333785741764, -207.6561946568479868 ) ) ;
#2155 = DIRECTION ( 'NONE',  ( 0.000000000000000000, 0.000000000000000000, 1.000000000000000000 ) ) ;
#2156 = CIRCLE ( 'NONE', #21833, 25.50000000000000355 ) ;
#2157 = CARTESIAN_POINT ( 'NONE',  ( 201.3567858607021606, 295.1816420246623238, -54.00000000001949019 ) ) ;
#2158 = CARTESIAN_POINT ( 'NONE',  ( 198.2830375120520046, 286.1211273803923518, -96.28769358250616506 ) ) ;
#2159 = CARTESIAN_POINT ( 'NONE',  ( -18.98628338888636335, -276.0069143675299301, -341.1825864986541319 ) ) ;
#2160 = CARTESIAN_POINT ( 'NONE',  ( -105.7980234881359252, -277.8229843096455056, -243.9900548994116321 ) ) ;
#2161 = CARTESIAN_POINT ( 'NONE',  ( -34.04393657811251472, -297.6000597370594392, -193.4229229018398541 ) ) ;
#2162 = CARTESIAN_POINT ( 'NONE',  ( -29.26882874936469037, -125.6146630139821951, -361.3924731419004388 ) ) ;
#2163 = CARTESIAN_POINT ( 'NONE',  ( -88.89226258380361401, -276.4434881388031613, -326.8928593510478890 ) ) ;
#2164 = CIRCLE ( 'NONE', #17308, 0.4999999999999922839 ) ;
#2165 = CARTESIAN_POINT ( 'NONE',  ( -50.27273100689873075, -296.9750370634604337, -345.2926686585216203 ) ) ;
#2166 = CARTESIAN_POINT ( 'NONE',  ( -82.57946348516480839, -290.1820548303577993, -327.7330031520684770 ) ) ;
#2167 = CARTESIAN_POINT ( 'NONE',  ( -36.55297263512778727, -298.8646194353156602, -193.5224886275879328 ) ) ;
#2168 = CARTESIAN_POINT ( 'NONE',  ( -68.80994990612290962, -274.3006431686073370, -200.1822055469266672 ) ) ;
#2169 = CARTESIAN_POINT ( 'NONE',  ( -108.2985123843628088, -296.4918970600967327, -287.5640672187727205 ) ) ;
#2170 = VERTEX_POINT ( 'NONE', #46370 ) ;
#2171 = LINE ( 'NONE', #86456, #14506 ) ;
#2172 = CONICAL_SURFACE ( 'NONE', #71746, 5.751884811727114410, 0.09862129276975223346 ) ;
#2173 = CIRCLE ( 'NONE', #35437, 20.00000000000000355 ) ;
#2174 = CARTESIAN_POINT ( 'NONE',  ( -107.3135515301804332, -280.1032050792717314, -298.8787302077540744 ) ) ;
#2175 = EDGE_CURVE ( 'NONE', #55409, #59842, #55372, .T. ) ;
#2176 = CARTESIAN_POINT ( 'NONE',  ( 28.24925827808030121, -281.5868286147847357, -310.6783973071230207 ) ) ;
#2177 = CARTESIAN_POINT ( 'NONE',  ( -97.12986316287404520, -279.0416937208063928, -312.8046259114348686 ) ) ;
#2178 = CARTESIAN_POINT ( 'NONE',  ( -113.0672085133617202, -280.2248409079646194, -277.2616554735079717 ) ) ;
#2179 = CARTESIAN_POINT ( 'NONE',  ( -37.12983572553468292, -296.6295895495666741, -196.7690653795428091 ) ) ;
#2180 = DIRECTION ( 'NONE',  ( 0.000000000000000000, 1.000000000000000000, 0.000000000000000000 ) ) ;
#2181 = CARTESIAN_POINT ( 'NONE',  ( 155.7140808774800007, 21.00000000000000000, 15.62500000000000000 ) ) ;
#2182 = CARTESIAN_POINT ( 'NONE',  ( -1.967936964375852638, -280.7013088756389152, -206.5042711753958145 ) ) ;
#2183 = CARTESIAN_POINT ( 'NONE',  ( 37.08489092440437673, -276.5945191054177030, -289.4619390470704161 ) ) ;
#2184 = AXIS2_PLACEMENT_3D ( 'NONE', #63537, #78191, #92363 ) ;
#2185 = CARTESIAN_POINT ( 'NONE',  ( 29.45714011259948961, -277.1013848038942342, -236.2595698035918872 ) ) ;
#2186 = CARTESIAN_POINT ( 'NONE',  ( 35.92328741275411375, -274.4017415834833287, -292.1062735238747905 ) ) ;
#2187 = VERTEX_POINT ( 'NONE', #4695 ) ;
#2188 = CARTESIAN_POINT ( 'NONE',  ( 200.1258905644044432, 39.98499045671346153, 10.50000000000114753 ) ) ;
#2189 = CARTESIAN_POINT ( 'NONE',  ( -90.87037250449097314, -290.4650436712174724, -220.4699305656451713 ) ) ;
#2190 = EDGE_CURVE ( 'NONE', #83649, #26494, #40004, .T. ) ;
#2191 = CARTESIAN_POINT ( 'NONE',  ( 7.491243797183925857, -285.9942245840188662, -207.8189745828121602 ) ) ;
#2192 = CARTESIAN_POINT ( 'NONE',  ( -83.44318099377669284, -281.9335766161375432, -328.3287769936021618 ) ) ;
#2194 = CARTESIAN_POINT ( 'NONE',  ( 0.9295821358342835072, -284.6464615516525214, -206.4525739628948600 ) ) ;
#2193 = CARTESIAN_POINT ( 'NONE',  ( -45.72447033844620279, -281.7350656210365401, -343.5227434028674907 ) ) ;
#2195 = CARTESIAN_POINT ( 'NONE',  ( 1.454519360038549980, -290.5343190514456069, -334.6069610176664355 ) ) ;
#2196 = CARTESIAN_POINT ( 'NONE',  ( 29.32696467460198875, -282.3438574566447983, -239.5405191740171915 ) ) ;
#2197 = CARTESIAN_POINT ( 'NONE',  ( -71.48679578107388011, -195.9896643738506157, -360.3036384909707976 ) ) ;
#2198 = CARTESIAN_POINT ( 'NONE',  ( -33.12361566198947571, -281.3997657408445434, -346.4572828301221534 ) ) ;
#2199 = CARTESIAN_POINT ( 'NONE',  ( 34.46253570979931879, -295.8334690828931457, -292.1971763898333734 ) ) ;
#2200 = CARTESIAN_POINT ( 'NONE',  ( -73.26651385536025884, -277.8223967714851597, -203.3883061970796575 ) ) ;
#2201 = CARTESIAN_POINT ( 'NONE',  ( -80.87344174830758448, -278.3124224331256755, -329.0882849443885334 ) ) ;
#2202 = CARTESIAN_POINT ( 'NONE',  ( -109.9569423336974978, -286.8036344208911146, -250.7473301568039403 ) ) ;
#2203 = FACE_OUTER_BOUND ( 'NONE', #28399, .T. ) ;
#2204 = CARTESIAN_POINT ( 'NONE',  ( -35.02944484669908576, -294.0010962748318661, -194.8235972500390005 ) ) ;
#2205 = CARTESIAN_POINT ( 'NONE',  ( 22.41543008159820971, -274.1719576823524562, -315.6831439879010759 ) ) ;
#2206 = CARTESIAN_POINT ( 'NONE',  ( -87.28725171546295769, -288.9247472652098736, -328.8227987163301691 ) ) ;
#2207 = CARTESIAN_POINT ( 'NONE',  ( 13.46854512744152110, -291.1777817917465541, -216.8376708685118217 ) ) ;
#2208 = CARTESIAN_POINT ( 'NONE',  ( -48.18343439340325318, -266.1601729329962609, -435.2001266877076660 ) ) ;
#2209 = CARTESIAN_POINT ( 'NONE',  ( -96.49986287289850395, -276.6296810931860364, -313.9890440177367736 ) ) ;
#2210 = CARTESIAN_POINT ( 'NONE',  ( -110.4889849235264876, -294.8559942294779148, -257.6985665523233706 ) ) ;
#2211 = CARTESIAN_POINT ( 'NONE',  ( -103.2805671625126962, -291.4304952868459395, -302.8158447689691570 ) ) ;
#2212 = CARTESIAN_POINT ( 'NONE',  ( 175.2296996224750103, 142.2541816238762920, 0.000000000000000000 ) ) ;
#2213 = DIRECTION ( 'NONE',  ( 0.000000000000000000, 1.000000000000000000, 0.000000000000000000 ) ) ;
#2214 = CARTESIAN_POINT ( 'NONE',  ( 18.91768952103209855, -291.3243543124797270, -218.8093107466258971 ) ) ;
#2215 = CARTESIAN_POINT ( 'NONE',  ( 36.25134222208720303, -289.2327586950282239, -276.5281224241958284 ) ) ;
#2216 = CARTESIAN_POINT ( 'NONE',  ( -111.9259605917659002, -288.9770328163453996, -255.7620185274782614 ) ) ;
#2217 = CARTESIAN_POINT ( 'NONE',  ( 35.71132314271395103, -289.0934693570068248, -279.2285137563272883 ) ) ;
#2218 = FACE_OUTER_BOUND ( 'NONE', #21146, .T. ) ;
#2219 = CARTESIAN_POINT ( 'NONE',  ( 1.405749720908947120, -289.3226808537093007, -332.4194522901951245 ) ) ;
#2220 = CARTESIAN_POINT ( 'NONE',  ( -73.78824644324126325, -297.5130670652411027, -336.3745011791797879 ) ) ;
#2221 = CARTESIAN_POINT ( 'NONE',  ( 201.2104617360081704, 0.000000000000000000, 10.00000000000000000 ) ) ;
#2222 = CARTESIAN_POINT ( 'NONE',  ( -62.61807503945496478, -290.5788577575258955, -342.7298173787915516 ) ) ;
#2223 = CARTESIAN_POINT ( 'NONE',  ( -67.98017750926324254, -277.6720681022069925, -201.5016318467622796 ) ) ;
#2224 = CARTESIAN_POINT ( 'NONE',  ( -77.80017677024424927, -277.9127130900238285, -335.9124174681257955 ) ) ;
#2225 = CARTESIAN_POINT ( 'NONE',  ( -1.141626563160716090, -280.1859037399913746, -202.4251263030592725 ) ) ;
#2226 = CARTESIAN_POINT ( 'NONE',  ( -109.3390285280996892, -274.7195291724283379, -251.2502868355318526 ) ) ;
#2227 = CARTESIAN_POINT ( 'NONE',  ( -35.86934699209479049, -284.0704663254091997, -195.3755671829415235 ) ) ;
#2228 = EDGE_CURVE ( 'NONE', #26085, #32648, #28827, .T. ) ;
#2229 = CARTESIAN_POINT ( 'NONE',  ( -48.18343439339130896, -269.7890444396779230, -499.6173591251650237 ) ) ;
#2230 = CARTESIAN_POINT ( 'NONE',  ( 5.657576158118884813, -278.7812504572832495, -209.8472541431163734 ) ) ;
#2231 = CARTESIAN_POINT ( 'NONE',  ( -64.55098927550875487, -281.4071551661360786, -340.2652635527532539 ) ) ;
#2232 = CARTESIAN_POINT ( 'NONE',  ( 200.6103193995254230, 275.5000000000000568, -2.464576988612312114 ) ) ;
#2233 = CARTESIAN_POINT ( 'NONE',  ( -68.74786636221647029, -275.9373961078078423, -339.9193412242318573 ) ) ;
#2234 = CARTESIAN_POINT ( 'NONE',  ( -55.95995789428866374, -296.8162748563663058, -341.7166470610565625 ) ) ;
#2235 = CARTESIAN_POINT ( 'NONE',  ( 11.28594217932069554, -281.3170560725138216, -329.7328204633518567 ) ) ;
#2236 = CARTESIAN_POINT ( 'NONE',  ( -69.37122856281865779, -298.5612167196425162, -204.5012838102906585 ) ) ;
#2237 = CARTESIAN_POINT ( 'NONE',  ( -85.45141967122081894, -274.8269922462721411, -210.9973143917986818 ) ) ;
#2238 = CARTESIAN_POINT ( 'NONE',  ( -91.13524100074610601, -272.9275398589860515, -220.9630344600264777 ) ) ;
#2239 = CARTESIAN_POINT ( 'NONE',  ( 37.64258315267473165, -295.5932523154244222, -273.5492605342137722 ) ) ;
#2240 = CARTESIAN_POINT ( 'NONE',  ( 36.69063261085982219, -287.4512972533717630, -249.0007533794227186 ) ) ;
#2241 = CARTESIAN_POINT ( 'NONE',  ( -83.66447488269824362, -277.5024444815465472, -210.5997397295432165 ) ) ;
#2242 = CIRCLE ( 'NONE', #50642, 2.999999999999999556 ) ;
#2243 = CARTESIAN_POINT ( 'NONE',  ( -111.9225647292233674, -290.1452350983350357, -289.5631431920322711 ) ) ;
#2244 = CARTESIAN_POINT ( 'NONE',  ( -84.84673796580017324, -288.7846177701384818, -326.1656610729313570 ) ) ;
#2245 = CARTESIAN_POINT ( 'NONE',  ( 29.13824727379464008, -291.0908401482650447, -235.5301247027963711 ) ) ;
#2246 = ORIENTED_EDGE ( 'NONE', *, *, #76301, .T. ) ;
#2247 = CARTESIAN_POINT ( 'NONE',  ( 198.0748556046041244, 67.35408903922716206, 11.09505092893674139 ) ) ;
#2248 = CARTESIAN_POINT ( 'NONE',  ( -80.44886470512516041, -289.1615874664133798, -329.4135744628986799 ) ) ;
#2249 = LINE ( 'NONE', #31133, #23268 ) ;
#2250 = CARTESIAN_POINT ( 'NONE',  ( 28.49057261907564254, -287.9757378242036339, -230.7753117105941101 ) ) ;
#2251 = CARTESIAN_POINT ( 'NONE',  ( -102.0172624299486870, -286.6233781216988064, -301.5434626090942061 ) ) ;
#2252 =( GEOMETRIC_REPRESENTATION_CONTEXT ( 3 ) GLOBAL_UNCERTAINTY_ASSIGNED_CONTEXT ( ( #85447 ) ) GLOBAL_UNIT_ASSIGNED_CONTEXT ( ( #20907, #28483, #57377 ) ) REPRESENTATION_CONTEXT ( 'NONE', 'WORKASPACE' ) );
#2253 = CARTESIAN_POINT ( 'NONE',  ( 30.68826836215341558, -293.0711394019737099, -305.9243517995561206 ) ) ;
#2254 = CARTESIAN_POINT ( 'NONE',  ( 34.13279988806474563, -283.2150239726330483, -297.6502022334577191 ) ) ;
#2255 = CARTESIAN_POINT ( 'NONE',  ( -3.623269331515478253, -282.4274979234524494, -335.1212998712824742 ) ) ;
#2256 = CARTESIAN_POINT ( 'NONE',  ( -73.94673581903742843, -273.7467471864824233, -202.5591599092967101 ) ) ;
#2257 = CARTESIAN_POINT ( 'NONE',  ( 33.37693755792928840, -277.1305385795566849, -290.4101538631343828 ) ) ;
#2258 = CARTESIAN_POINT ( 'NONE',  ( -4.077959936533853025, -290.5130121382752577, -203.5234506636695357 ) ) ;
#2259 = AXIS2_PLACEMENT_3D ( 'NONE', #79399, #14535, #43390 ) ;
#2260 = CARTESIAN_POINT ( 'NONE',  ( -27.22032104452931733, -272.9784339480717676, -197.6140809357097794 ) ) ;
#2261 = ORIENTED_EDGE ( 'NONE', *, *, #4649, .T. ) ;
#2262 = DIRECTION ( 'NONE',  ( -0.000000000000000000, -1.000000000000000000, -0.000000000000000000 ) ) ;
#2263 = CARTESIAN_POINT ( 'NONE',  ( -65.66330152257987152, -287.5991558815953226, -201.4643838546886911 ) ) ;
#2264 = CARTESIAN_POINT ( 'NONE',  ( -105.6760030247050395, -297.1803814325327835, -305.2906364265959951 ) ) ;
#2265 = CARTESIAN_POINT ( 'NONE',  ( -67.59744818887935480, -286.2957780997120949, -203.8142744977607208 ) ) ;
#2266 = CARTESIAN_POINT ( 'NONE',  ( -111.2173512151290282, -277.3486471424189972, -291.2227667612635855 ) ) ;
#2267 = CARTESIAN_POINT ( 'NONE',  ( 39.40103137295275104, -294.2744720669308549, -276.0233666051173032 ) ) ;
#2268 = CARTESIAN_POINT ( 'NONE',  ( 36.81942048749449725, -285.4938575322436805, -254.7922843445198282 ) ) ;
#2269 = CARTESIAN_POINT ( 'NONE',  ( 24.87169684607839315, -294.4875369327571093, -315.7180509856348181 ) ) ;
#2270 = CARTESIAN_POINT ( 'NONE',  ( -90.77755225477530132, -291.6009740928693645, -220.5762030113426704 ) ) ;
#2271 = DIRECTION ( 'NONE',  ( 0.000000000000000000, 0.000000000000000000, -1.000000000000000000 ) ) ;
#2272 = DIRECTION ( 'NONE',  ( 1.000000000000000000, 0.000000000000000000, 0.000000000000000000 ) ) ;
#2273 = CARTESIAN_POINT ( 'NONE',  ( -76.15440596509891691, -208.4761271767464166, -353.6627180100853138 ) ) ;
#2274 = CARTESIAN_POINT ( 'NONE',  ( -103.4495602201036490, -286.5733906563336291, -232.1448614068082463 ) ) ;
#2275 = CARTESIAN_POINT ( 'NONE',  ( 13.79469577742117181, -273.9094976428776818, -334.5364918783848793 ) ) ;
#2276 = VERTEX_POINT ( 'NONE', #93668 ) ;
#2277 = CARTESIAN_POINT ( 'NONE',  ( -102.0505166742203471, -283.0036781961101724, -304.9219922368613993 ) ) ;
#2278 = CARTESIAN_POINT ( 'NONE',  ( -112.6959718101545320, -278.4164608696051459, -254.5661333235538279 ) ) ;
#2279 = CARTESIAN_POINT ( 'NONE',  ( 35.22735075649669767, -283.3165065662468010, -252.0399938651215450 ) ) ;
#2280 = CARTESIAN_POINT ( 'NONE',  ( 175.7400943157809934, 241.1710852490582795, -178.6611720099773493 ) ) ;
#2281 = CARTESIAN_POINT ( 'NONE',  ( -93.01475989681885892, -282.4069054273312531, -322.7168764665680669 ) ) ;
#2282 = CARTESIAN_POINT ( 'NONE',  ( 36.58593835799844385, -285.7066235022497835, -280.7763149029742635 ) ) ;
#2283 = CARTESIAN_POINT ( 'NONE',  ( -69.62729786191843573, -275.4921578734091554, -201.8053726309009051 ) ) ;
#2284 = CARTESIAN_POINT ( 'NONE',  ( -110.4455981908226079, -297.0298829515062948, -271.4703025446996776 ) ) ;
#2285 = CARTESIAN_POINT ( 'NONE',  ( 34.70322114486324239, -292.0467435590864511, -255.8431016554352766 ) ) ;
#2286 = CARTESIAN_POINT ( 'NONE',  ( -95.12870360745725407, -278.5160725051208033, -321.0954753319850852 ) ) ;
#2287 = CARTESIAN_POINT ( 'NONE',  ( 0.8714263338593288832, -276.5272476975952145, -332.6198467689641234 ) ) ;
#2288 = CARTESIAN_POINT ( 'NONE',  ( -110.7452984687751751, -273.9138284787135831, -247.9667738070575069 ) ) ;
#2289 = CARTESIAN_POINT ( 'NONE',  ( -35.73183820551313516, -275.9527672792785893, -347.0481797648846509 ) ) ;
#2290 = CARTESIAN_POINT ( 'NONE',  ( -56.60324186025278692, -169.1846951021010170, -364.3055494911728829 ) ) ;
#2291 = CARTESIAN_POINT ( 'NONE',  ( -95.68291027872491838, -275.9030506399489013, -317.5118654783422585 ) ) ;
#2292 = CARTESIAN_POINT ( 'NONE',  ( 15.08767394035932163, -295.7547411620569733, -325.9467908356010071 ) ) ;
#2293 = ADVANCED_FACE ( 'NONE', ( #78552 ), #42068, .F. ) ;
#2294 = CARTESIAN_POINT ( 'NONE',  ( 180.2262870919856823, 214.9642003054772488, -24.76688354601323283 ) ) ;
#2295 = CARTESIAN_POINT ( 'NONE',  ( 151.9709352735115147, -299.5541904835127980, -195.3611179825600175 ) ) ;
#2296 = CARTESIAN_POINT ( 'NONE',  ( -110.1782350143009808, -285.5169185262721498, -279.1088324629775457 ) ) ;
#2297 = CARTESIAN_POINT ( 'NONE',  ( -47.10368354335948737, -284.9346812822123525, -345.7181195953769475 ) ) ;
#2298 = CARTESIAN_POINT ( 'NONE',  ( -52.10142168324821910, -285.2067626783365881, -198.7647264013608606 ) ) ;
#2299 = CARTESIAN_POINT ( 'NONE',  ( -110.9680387438430813, -276.8768546226355625, -276.1212530909722318 ) ) ;
#2300 = CARTESIAN_POINT ( 'NONE',  ( -105.2335585894003600, -286.0151975573086816, -300.3871239151109194 ) ) ;
#2301 = CARTESIAN_POINT ( 'NONE',  ( -77.18055106536478149, -277.9877595503423890, -208.3037345103906546 ) ) ;
#2302 = CARTESIAN_POINT ( 'NONE',  ( -37.79794088248138451, -278.1376362845738299, -343.6813172707657600 ) ) ;
#2303 = CARTESIAN_POINT ( 'NONE',  ( 207.3561592308186334, 36.17070937851315193, 14.95737379494689456 ) ) ;
#2304 = CARTESIAN_POINT ( 'NONE',  ( -100.7743049724189177, -273.5420382400129711, -234.0061868943173806 ) ) ;
#2305 = CARTESIAN_POINT ( 'NONE',  ( 10.71403707775604630, -281.4996777104981334, -210.3362354427328853 ) ) ;
#2306 = CARTESIAN_POINT ( 'NONE',  ( -17.01428821104827094, -280.8001592551700014, -196.1565141643202423 ) ) ;
#2307 = ORIENTED_EDGE ( 'NONE', *, *, #76975, .F. ) ;
#2308 = VERTEX_POINT ( 'NONE', #13233 ) ;
#2309 = CARTESIAN_POINT ( 'NONE',  ( 199.1517898866434848, 16.71555987447352720, -10.28330198088200120 ) ) ;
#2310 = CARTESIAN_POINT ( 'NONE',  ( -0.3404726754234554398, -288.3990524599335004, -204.2311519053499751 ) ) ;
#2311 = CARTESIAN_POINT ( 'NONE',  ( -79.81349927328808747, -296.6582700005264996, -210.7897489880191984 ) ) ;
#2312 = ADVANCED_FACE ( 'NONE', ( #65297 ), #79334, .T. ) ;
#2313 = ADVANCED_FACE ( 'NONE', ( #57710 ), #13689, .T. ) ;
#2314 = CARTESIAN_POINT ( 'NONE',  ( -86.44156338526975958, -290.7397834800261194, -211.1099247157329444 ) ) ;
#2315 = CARTESIAN_POINT ( 'NONE',  ( 16.50445825212031536, -286.7495665182208882, -320.7477781803256107 ) ) ;
#2316 = ADVANCED_BREP_SHAPE_REPRESENTATION ( '', ( #28963, #18940 ), #47644 ) ;
#2317 = CARTESIAN_POINT ( 'NONE',  ( -72.65745444598745451, -288.1042941246570877, -334.9225028419774048 ) ) ;
#2318 = CARTESIAN_POINT ( 'NONE',  ( -96.09295359081254162, -286.3713954302164097, -226.3677011752311046 ) ) ;
#2319 = CARTESIAN_POINT ( 'NONE',  ( -76.78532099673294908, -275.5796475823318019, -334.2117729292891113 ) ) ;
#2320 = CARTESIAN_POINT ( 'NONE',  ( 9.717715720091057108, -286.8169561901785869, -330.3602902612408343 ) ) ;
#2321 = CARTESIAN_POINT ( 'NONE',  ( 29.62429522301378171, -289.1061269922853967, -236.5889976418591232 ) ) ;
#2322 = CARTESIAN_POINT ( 'NONE',  ( -20.92229114266228507, -286.8418832625529262, -343.7659035601654978 ) ) ;
#2323 = VECTOR ( 'NONE', #62128, 1000.000000000000114 ) ;
#2324 = CARTESIAN_POINT ( 'NONE',  ( 12.08428806789046739, -283.2854833372259122, -324.4025848245134398 ) ) ;
#2325 = CARTESIAN_POINT ( 'NONE',  ( -112.5553537023478441, -292.5411397825399717, -271.2335204130772581 ) ) ;
#2326 = DIRECTION ( 'NONE',  ( 0.000000000000000000, 1.000000000000000000, 0.000000000000000000 ) ) ;
#2327 = DIRECTION ( 'NONE',  ( -0.000000000000000000, -0.000000000000000000, 1.000000000000000000 ) ) ;
#2328 = CARTESIAN_POINT ( 'NONE',  ( -97.11024979582101935, -299.1013985599712441, -224.1121546556895510 ) ) ;
#2329 = VECTOR ( 'NONE', #75642, 1000.000000000000000 ) ;
#2330 = CARTESIAN_POINT ( 'NONE',  ( 33.91999220654804503, -280.5312872617810172, -253.7969115975176067 ) ) ;
#2331 = CARTESIAN_POINT ( 'NONE',  ( 37.01910815044121961, -279.4215622442448534, -260.2030912569527459 ) ) ;
#2332 = CARTESIAN_POINT ( 'NONE',  ( -13.84117010841714901, -293.9519134314286362, -343.5176891770710199 ) ) ;
#2333 = CARTESIAN_POINT ( 'NONE',  ( -70.81236020727760661, -296.0029299564718031, -204.5735400505934081 ) ) ;
#2334 = CARTESIAN_POINT ( 'NONE',  ( -15.99078679757546340, -274.8538637697693616, -341.7275270703441947 ) ) ;
#2335 = CARTESIAN_POINT ( 'NONE',  ( -2.897907067329185349, -295.9020067124427555, -335.2831373490424198 ) ) ;
#2336 = DIRECTION ( 'NONE',  ( 0.8429829950866641886, 0.5379402104274390028, -0.000000000000000000 ) ) ;
#2337 = CARTESIAN_POINT ( 'NONE',  ( -73.64876197396921498, -272.1550520232934787, -203.0683588118110379 ) ) ;
#2338 = CARTESIAN_POINT ( 'NONE',  ( -63.93285093123521534, -293.6341073546713005, -341.5431712844045933 ) ) ;
#2339 = CARTESIAN_POINT ( 'NONE',  ( -37.56985275435032179, -293.4745510285827095, -196.7596968199149501 ) ) ;
#2340 = DIRECTION ( 'NONE',  ( -0.000000000000000000, 0.000000000000000000, 1.000000000000000000 ) ) ;
#2341 = CARTESIAN_POINT ( 'NONE',  ( 23.07210063998580196, -294.9289462310797489, -311.7144138195880601 ) ) ;
#2342 = CARTESIAN_POINT ( 'NONE',  ( 208.4306832106271088, 0.000000000000000000, 0.000000000000000000 ) ) ;
#2344 = CARTESIAN_POINT ( 'NONE',  ( 27.15807033942866155, -294.0191603917574525, -304.6565546054134188 ) ) ;
#2343 = CARTESIAN_POINT ( 'NONE',  ( -110.2892195143455041, -282.3300111003733832, -289.3085383194310225 ) ) ;
#2345 = B_SPLINE_CURVE_WITH_KNOTS ( 'NONE', 3,
 ( #61003, #39638, #53881, #91241, #19759, #70446, #11261, #68563, #40573, #69029, #83679, #25010, #91717, #55294, #18841, #47698, #11719, #89848 ),
 .UNSPECIFIED., .F., .F.,
 ( 4, 2, 2, 2, 2, 2, 2, 2, 4 ),
 ( 0.000000000000000000, 0.0005979543124017953383, 0.001195908624803590677, 0.001793862937205386015, 0.002391817249607181353, 0.002989771562008976691, 0.003587725874410772030, 0.004185680186812567802, 0.004783634499214362706 ),
 .UNSPECIFIED. ) ;
#2346 = CARTESIAN_POINT ( 'NONE',  ( -66.57625017306888537, -283.4246095075651510, -341.6097132827006817 ) ) ;
#2347 = CARTESIAN_POINT ( 'NONE',  ( 35.21007397252864735, -283.2020155370854013, -249.2066292902416365 ) ) ;
#2348 = CARTESIAN_POINT ( 'NONE',  ( -93.90131680918844381, -284.9307287537023399, -218.0646712839107693 ) ) ;
#2349 = CARTESIAN_POINT ( 'NONE',  ( -100.4000020614363393, -288.0083156824197204, -310.6560181938254459 ) ) ;
#2350 = CARTESIAN_POINT ( 'NONE',  ( 142.6449502718966755, 0.000000000000000000, 21.50000000000000000 ) ) ;
#2351 = CARTESIAN_POINT ( 'NONE',  ( 19.25612745805068471, -280.7340573207635543, -321.6184119485980659 ) ) ;
#2352 = CARTESIAN_POINT ( 'NONE',  ( 11.47404437362297180, -285.4305280864174961, -215.3539756115959563 ) ) ;
#2353 = CARTESIAN_POINT ( 'NONE',  ( 36.84190215760990839, -286.7169291577924923, -289.8106851383240041 ) ) ;
#2354 = CARTESIAN_POINT ( 'NONE',  ( 19.46176235605588900, -295.8132373981581509, -317.4759465088477555 ) ) ;
#2355 = CARTESIAN_POINT ( 'NONE',  ( -97.24635011782608274, -280.6170286888922760, -222.9265398223296302 ) ) ;
#2357 = CARTESIAN_POINT ( 'NONE',  ( -16.91173510106462174, -279.9900987005459569, -200.2561679740749980 ) ) ;
#2356 = CARTESIAN_POINT ( 'NONE',  ( -52.97321076489322422, -293.2715185747370583, -344.1305950818194219 ) ) ;
#2358 = CARTESIAN_POINT ( 'NONE',  ( 37.76083416989510511, -293.5056996349703127, -253.3135023623635504 ) ) ;
#2359 = CARTESIAN_POINT ( 'NONE',  ( -108.8695594198320720, -282.3193183739194865, -294.7143424573694688 ) ) ;
#2360 = CARTESIAN_POINT ( 'NONE',  ( -39.86935474058879691, -279.0840375942528340, -345.3312437491790092 ) ) ;
#2361 = CARTESIAN_POINT ( 'NONE',  ( -73.42875210752718829, -294.6022849606284240, -334.0881383726343756 ) ) ;
#2362 = CARTESIAN_POINT ( 'NONE',  ( -51.40008341153777849, -295.8723580452389115, -196.6375582276594969 ) ) ;
#2363 = ORIENTED_EDGE ( 'NONE', *, *, #88613, .F. ) ;
#2364 = CARTESIAN_POINT ( 'NONE',  ( 200.2349812190172713, 66.43136063442170780, -7.741079165001061746 ) ) ;
#2365 = CARTESIAN_POINT ( 'NONE',  ( -1.191090837588199225, -282.5142281842524312, -205.0543017072447185 ) ) ;
#2366 = CARTESIAN_POINT ( 'NONE',  ( -45.10350010521774777, -294.6606065751674350, -343.0597130516309221 ) ) ;
#2367 = DIRECTION ( 'NONE',  ( 0.000000000000000000, 0.000000000000000000, 1.000000000000000000 ) ) ;
#2368 = CARTESIAN_POINT ( 'NONE',  ( -37.37352853689063181, -274.5523547857346784, -345.3611179825600175 ) ) ;
#2369 = CARTESIAN_POINT ( 'NONE',  ( 11.69052944090781310, -273.9097949304809276, -211.1311788300132264 ) ) ;
#2370 = CARTESIAN_POINT ( 'NONE',  ( -26.19972767792013713, -290.2283118574376886, -346.0522979289643786 ) ) ;
#2371 = CARTESIAN_POINT ( 'NONE',  ( -106.9527405965465476, -290.0920538385502709, -292.5124797387500166 ) ) ;
#2372 = CARTESIAN_POINT ( 'NONE',  ( -30.21441684358461544, -281.6639377239478677, -196.9624178316807956 ) ) ;
#2373 = CARTESIAN_POINT ( 'NONE',  ( -109.9202075428785577, -274.3303380581464808, -256.7157215857342294 ) ) ;
#2374 = CARTESIAN_POINT ( 'NONE',  ( 7.396438086658410072, -279.4723336308808257, -212.1106403080696907 ) ) ;
#2375 = ORIENTED_EDGE ( 'NONE', *, *, #74127, .F. ) ;
#2376 = CARTESIAN_POINT ( 'NONE',  ( 11.78732464390185797, -274.5458451004375320, -211.0015375460011740 ) ) ;
#2377 = CARTESIAN_POINT ( 'NONE',  ( -36.20825719148006527, -293.9865892983897311, -195.9170205862630496 ) ) ;
#2378 = CARTESIAN_POINT ( 'NONE',  ( 214.2238915819278589, 32.98517505407394168, 9.000000000000001776 ) ) ;
#2379 = EDGE_CURVE ( 'NONE', #14296, #31036, #74788, .T. ) ;
#2380 = CARTESIAN_POINT ( 'NONE',  ( 196.0742305401642511, 73.02742819586271139, 11.89621339062204264 ) ) ;
#2381 = CARTESIAN_POINT ( 'NONE',  ( -36.37002147508545846, -290.2038029420513681, -194.5897215437361751 ) ) ;
#2382 = CARTESIAN_POINT ( 'NONE',  ( -36.47883191666217328, -297.7299650106613740, -197.3400242297411182 ) ) ;
#2383 = CARTESIAN_POINT ( 'NONE',  ( 175.2296996224750103, 247.0000000000001137, -8.550761578869359170 ) ) ;
#2384 = PRODUCT_DEFINITION_FORMATION_WITH_SPECIFIED_SOURCE ( 'ANY', '', #44255, .NOT_KNOWN. ) ;
#2385 = CARTESIAN_POINT ( 'NONE',  ( -113.5578456738071935, -292.0253799048121550, -274.0768829384814467 ) ) ;
#2386 = CARTESIAN_POINT ( 'NONE',  ( -19.11405058567862625, -294.7662352645559736, -190.3538533559490702 ) ) ;
#2387 = CARTESIAN_POINT ( 'NONE',  ( 30.46055287969270253, -289.1351492837338242, -238.6927913698075372 ) ) ;
#2388 = CARTESIAN_POINT ( 'NONE',  ( -10.62266284991046028, -274.7026527243753549, -340.2619153569320929 ) ) ;
#2389 = CARTESIAN_POINT ( 'NONE',  ( 20.96851465639591439, -276.8315246912528096, -224.0672715805402504 ) ) ;
#2390 = CARTESIAN_POINT ( 'NONE',  ( 3.041837134920090335, -290.6784192119872614, -207.7661812040237805 ) ) ;
#2391 = CARTESIAN_POINT ( 'NONE',  ( -56.27131836490882932, -281.6713580191880055, -196.9450497220784086 ) ) ;
#2392 = MECHANICAL_DESIGN_GEOMETRIC_PRESENTATION_REPRESENTATION (  '', ( #31117 ), #84023 ) ;
#2393 = ORIENTED_EDGE ( 'NONE', *, *, #76002, .F. ) ;
#2394 = CARTESIAN_POINT ( 'NONE',  ( -53.72056482496905261, -282.6163832278657537, -341.6567004821625915 ) ) ;
#2395 = CARTESIAN_POINT ( 'NONE',  ( -77.64072628188118586, -278.6589829938239973, -335.6721994885797358 ) ) ;
#2396 = CARTESIAN_POINT ( 'NONE',  ( 17.53107308459359714, -281.0844438218102823, -323.8876904598456008 ) ) ;
#2397 = CARTESIAN_POINT ( 'NONE',  ( -100.2657439814591385, -278.9103520919917401, -314.3313911027744894 ) ) ;
#2398 = CARTESIAN_POINT ( 'NONE',  ( -2.888072313469212116, -276.0192265579439663, -202.2609024276526668 ) ) ;
#2399 = CARTESIAN_POINT ( 'NONE',  ( 27.36219212280431989, -284.4805209788416391, -301.4846348637938149 ) ) ;
#2400 = ORIENTED_EDGE ( 'NONE', *, *, #55197, .T. ) ;
#2401 = CARTESIAN_POINT ( 'NONE',  ( -112.3848973411877950, -298.5374536137122732, -271.5187285978493037 ) ) ;
#2402 = CARTESIAN_POINT ( 'NONE',  ( -86.92839002084259903, -290.8411630607247957, -324.4242874364562681 ) ) ;
#2403 = CARTESIAN_POINT ( 'NONE',  ( -13.27849275885741065, -274.7583160877609316, -341.0752561779326015 ) ) ;
#2404 = CARTESIAN_POINT ( 'NONE',  ( -70.18057860147415283, -291.2389563376514161, -338.8997289832494744 ) ) ;
#2405 = CARTESIAN_POINT ( 'NONE',  ( -94.36521346548927625, -290.5465004580488539, -224.6005297093131219 ) ) ;
#2406 = CARTESIAN_POINT ( 'NONE',  ( 37.31863131032162784, -286.8271222588363116, -251.7772052354250718 ) ) ;
#2407 = CARTESIAN_POINT ( 'NONE',  ( 189.9243309297870610, 215.0000000000000568, 25.22542485937348644 ) ) ;
#2408 = CARTESIAN_POINT ( 'NONE',  ( -110.2077907440444022, -283.1057778829976996, -258.5776496901708583 ) ) ;
#2409 = CARTESIAN_POINT ( 'NONE',  ( -106.2509406892953052, -292.0475346752432984, -298.1102357068517676 ) ) ;
#2410 = CARTESIAN_POINT ( 'NONE',  ( -62.78424581810185146, -284.1948704720394403, -201.1446866725465838 ) ) ;
#2411 = CARTESIAN_POINT ( 'NONE',  ( 0.6405716419054025002, -281.8848009400309707, -207.3848841765032773 ) ) ;
#2412 = CARTESIAN_POINT ( 'NONE',  ( 31.48180083919579886, -288.9330326451807878, -304.4831849100746126 ) ) ;
#2413 = CARTESIAN_POINT ( 'NONE',  ( -91.34652890947378978, -279.7495179408469426, -221.1527151429708056 ) ) ;
#2414 = CARTESIAN_POINT ( 'NONE',  ( 34.09810750059581608, -291.9933715860795473, -242.5673455710627593 ) ) ;
#2415 = CARTESIAN_POINT ( 'NONE',  ( 38.51723649147143647, -288.5123174863997519, -282.9151757114605061 ) ) ;
#2416 = CARTESIAN_POINT ( 'NONE',  ( -69.77261671130307263, -286.1288604391023114, -200.5774111389115149 ) ) ;
#2417 = CARTESIAN_POINT ( 'NONE',  ( -84.86017187945472529, -283.8959858414048654, -325.7776754983261753 ) ) ;
#2418 = ORIENTED_EDGE ( 'NONE', *, *, #35543, .T. ) ;
#2419 = CARTESIAN_POINT ( 'NONE',  ( 175.2296996224750103, 133.0000000000000000, 0.000000000000000000 ) ) ;
#2420 = CARTESIAN_POINT ( 'NONE',  ( 33.30238579561800805, -295.0583696151126105, -242.8352620235359609 ) ) ;
#2421 = CARTESIAN_POINT ( 'NONE',  ( 17.19816457336363058, -292.9790586830068833, -324.0899834076009256 ) ) ;
#2422 = CARTESIAN_POINT ( 'NONE',  ( -16.32477394961795980, -275.8326082407812123, -340.5691043169587147 ) ) ;
#2423 = CARTESIAN_POINT ( 'NONE',  ( -70.67734101756153109, -296.9725667447256683, -201.0643082889385767 ) ) ;
#2424 = CARTESIAN_POINT ( 'NONE',  ( 35.59671247223678847, -291.8945387362592214, -259.8399146305260388 ) ) ;
#2425 = CARTESIAN_POINT ( 'NONE',  ( -110.8131974872760139, -294.6703414406898673, -279.7119362418612241 ) ) ;
#2426 = CARTESIAN_POINT ( 'NONE',  ( -4.670041263478490023, -293.6974645934221826, -204.6227457080949250 ) ) ;
#2427 = CARTESIAN_POINT ( 'NONE',  ( 23.59055957170356521, -294.0681241304459377, -229.5997907031644161 ) ) ;
#2428 = CARTESIAN_POINT ( 'NONE',  ( 208.0521033162707738, 35.78478885999048487, 14.36581762243483773 ) ) ;
#2429 = CARTESIAN_POINT ( 'NONE',  ( -22.48541094444601995, -292.8622030144426844, -344.0450313913269724 ) ) ;
#2430 = CARTESIAN_POINT ( 'NONE',  ( -104.9446028033678431, -298.9813624462061057, -237.7643205647046614 ) ) ;
#2431 = CARTESIAN_POINT ( 'NONE',  ( 27.24360732475430780, -288.9638346358789249, -304.9965575090857897 ) ) ;
#2432 = CARTESIAN_POINT ( 'NONE',  ( -64.47869382042421194, -279.3843633652002154, -340.7154844104159110 ) ) ;
#2433 = CARTESIAN_POINT ( 'NONE',  ( 3.277872121411345763, -275.3145317421886489, -335.3701372609937721 ) ) ;
#2434 = ADVANCED_FACE ( 'NONE', ( #42541 ), #63901, .T. ) ;
#2435 = CARTESIAN_POINT ( 'NONE',  ( 1.151591253278470894, -273.9005858307074277, -203.7757440722843967 ) ) ;
#2436 = CARTESIAN_POINT ( 'NONE',  ( 25.32983365565038980, -280.1780890191662934, -310.6253857454715899 ) ) ;
#2437 = CARTESIAN_POINT ( 'NONE',  ( -25.91030507356118662, -275.3087558394569214, -345.6987820090255354 ) ) ;
#2438 = ADVANCED_FACE ( 'NONE', ( #27420 ), #34527, .T. ) ;
#2439 = CARTESIAN_POINT ( 'NONE',  ( -110.7350194627203450, -295.1867942690556674, -274.1904983298594516 ) ) ;
#2440 = CARTESIAN_POINT ( 'NONE',  ( -65.99069756724364311, -275.6774747864053552, -201.0348621853013356 ) ) ;
#2441 = CARTESIAN_POINT ( 'NONE',  ( -92.99677433997791809, -273.8769465895456960, -222.9455333364743126 ) ) ;
#2442 = CYLINDRICAL_SURFACE ( 'NONE', #62544, 2.842139515347646750 ) ;
#2444 = CARTESIAN_POINT ( 'NONE',  ( -32.68891170524955925, -273.9457094342653818, -197.4970195534421293 ) ) ;
#2443 = CARTESIAN_POINT ( 'NONE',  ( -106.2380124564062953, -288.1727745790136623, -301.0133967033503950 ) ) ;
#2445 = CARTESIAN_POINT ( 'NONE',  ( -9.563331133520202698, -288.6990254255125024, -342.1758951248863809 ) ) ;
#2446 = CARTESIAN_POINT ( 'NONE',  ( -15.43315215435428911, -300.3050012637568784, -194.9985599119324604 ) ) ;
#2447 = CARTESIAN_POINT ( 'NONE',  ( -93.58499416087970246, -293.8646530689550218, -319.7242652163323555 ) ) ;
#2448 = CARTESIAN_POINT ( 'NONE',  ( -41.57049742590108110, -282.3011711864564859, -347.1354049258234227 ) ) ;
#2449 = CYLINDRICAL_SURFACE ( 'NONE', #86484, 4.000000000000003553 ) ;
#2450 = CARTESIAN_POINT ( 'NONE',  ( 32.33756184536254352, -279.9149438931633540, -298.2448987394334949 ) ) ;
#2451 = VECTOR ( 'NONE', #84118, 1000.000000000000000 ) ;
#2452 = PRODUCT_RELATED_PRODUCT_CATEGORY ( 'part', '', ( #1958 ) ) ;
#2453 = CARTESIAN_POINT ( 'NONE',  ( 200.4566814582243808, 25.65177970828076681, 10.50000000000112799 ) ) ;
#2454 = CARTESIAN_POINT ( 'NONE',  ( -108.8106150073328564, -289.5670728927869959, -253.5933460248497227 ) ) ;
#2455 = CARTESIAN_POINT ( 'NONE',  ( -102.8725561325814226, -282.2230593162726677, -305.3499860189297692 ) ) ;
#2456 = CARTESIAN_POINT ( 'NONE',  ( 200.3284360491938116, 214.9642003054772488, -2.901350841306745476 ) ) ;
#2457 = SURFACE_SIDE_STYLE ('',( #74401 ) ) ;
#2458 = CARTESIAN_POINT ( 'NONE',  ( -107.5747994095082873, -288.8953773185871228, -243.9020588889401893 ) ) ;
#2459 = CARTESIAN_POINT ( 'NONE',  ( -59.70429240495381151, -275.2774344503241650, -200.0892990232544548 ) ) ;
#2460 = CARTESIAN_POINT ( 'NONE',  ( -81.32097392682602788, -284.8402280689018085, -333.1459105784276744 ) ) ;
#2462 = CARTESIAN_POINT ( 'NONE',  ( -10.74997186824332474, -286.4088293835263812, -202.3631822162128344 ) ) ;
#2461 = CARTESIAN_POINT ( 'NONE',  ( -13.49336395985828752, -272.4392708445743665, -198.6633421562725630 ) ) ;
#2463 = CARTESIAN_POINT ( 'NONE',  ( 35.69318083708846245, -277.1007374102973699, -279.7839234860754232 ) ) ;
#2464 = CARTESIAN_POINT ( 'NONE',  ( 30.43146551669902422, -276.7249088396201273, -298.0531741480480150 ) ) ;
#2465 = CARTESIAN_POINT ( 'NONE',  ( -34.52782412456014782, -285.0169364489924533, -345.3083177512349948 ) ) ;
#2466 = VERTEX_POINT ( 'NONE', #402 ) ;
#2467 = CARTESIAN_POINT ( 'NONE',  ( 200.4551663813218170, 64.49084098419280053, 2.617322427804800622 ) ) ;
#2468 = CARTESIAN_POINT ( 'NONE',  ( -41.94768288338276108, -294.9418706406960382, -347.2756277286085265 ) ) ;
#2469 = CARTESIAN_POINT ( 'NONE',  ( 32.50494542338549309, -289.1867028367436205, -243.8848862199949963 ) ) ;
#2470 = CYLINDRICAL_SURFACE ( 'NONE', #63999, 5.000000000000004441 ) ;
#2471 = CARTESIAN_POINT ( 'NONE',  ( 40.64545035920995986, -291.2666405000203440, -288.1938231032136741 ) ) ;
#2472 = CARTESIAN_POINT ( 'NONE',  ( -112.1857616634828645, -277.2624241539681407, -287.0901037333476893 ) ) ;
#2473 = CARTESIAN_POINT ( 'NONE',  ( -103.9011893556237141, -289.4380373701298481, -233.2629400291850175 ) ) ;
#2474 = CARTESIAN_POINT ( 'NONE',  ( -110.6864656399369693, -286.1724318225008687, -262.6970049916134258 ) ) ;
#2475 = CARTESIAN_POINT ( 'NONE',  ( -95.60222064919906870, -280.9472530154350807, -224.6933035624708168 ) ) ;
#2476 = CARTESIAN_POINT ( 'NONE',  ( -54.84737931417252099, -287.2566344071678941, -195.9826433577420630 ) ) ;
#2477 = CARTESIAN_POINT ( 'NONE',  ( -12.85290433956945577, -284.7341782101797207, -341.3055452751005987 ) ) ;
#2478 = CARTESIAN_POINT ( 'NONE',  ( -42.80405109958635990, -277.2859728771105097, -347.1671250807937668 ) ) ;
#2479 = CARTESIAN_POINT ( 'NONE',  ( -102.2967516304183846, -271.0499318740187960, -233.0969194531548396 ) ) ;
#2480 = CARTESIAN_POINT ( 'NONE',  ( -19.75416020125787142, -280.1054263353923375, -195.3418325556406216 ) ) ;
#2481 = CARTESIAN_POINT ( 'NONE',  ( -109.2326051827405280, -298.7230397365784142, -250.9984197659080394 ) ) ;
#2482 = CARTESIAN_POINT ( 'NONE',  ( 0.000000000000000000, 0.000000000000000000, 10.00000000000000000 ) ) ;
#2483 = CARTESIAN_POINT ( 'NONE',  ( -85.28047601435908120, -280.1948066931273047, -330.5268031993605859 ) ) ;
#2484 = CARTESIAN_POINT ( 'NONE',  ( -31.99397031523169943, -296.2580116381537323, -194.5979839244863285 ) ) ;
#2485 = DIRECTION ( 'NONE',  ( -0.6056179655966483777, 0.7957555401921979632, -0.000000000000000000 ) ) ;
#2486 = CARTESIAN_POINT ( 'NONE',  ( -72.87741659627590707, -277.0441251465967412, -334.2128157899669532 ) ) ;
#2487 = CARTESIAN_POINT ( 'NONE',  ( -29.89284046659686922, -275.3495337395068532, -194.1212123687265603 ) ) ;
#2488 = CARTESIAN_POINT ( 'NONE',  ( 39.17812565146557091, -280.5340444180471877, -264.2344161684337678 ) ) ;
#2489 = CARTESIAN_POINT ( 'NONE',  ( 29.14777769934636709, -289.7466609382010461, -302.8745513465544263 ) ) ;
#2490 = CARTESIAN_POINT ( 'NONE',  ( -111.6041093367672801, -298.2936890885879961, -252.8168216423337640 ) ) ;
#2491 = CARTESIAN_POINT ( 'NONE',  ( -90.42579470457449986, -296.9883760940584239, -325.6617309611877999 ) ) ;
#2492 = CARTESIAN_POINT ( 'NONE',  ( 14.14656434473762658, -294.7774907196733807, -216.0565413230712863 ) ) ;
#2493 = CARTESIAN_POINT ( 'NONE',  ( 23.28257652777596221, -280.1509791272385428, -314.2547421445567579 ) ) ;
#2494 = CARTESIAN_POINT ( 'NONE',  ( 37.00532661597684836, -283.5204280807112127, -274.0805009427418781 ) ) ;
#2495 = CARTESIAN_POINT ( 'NONE',  ( -103.8072740394163418, -295.0795299535373033, -236.7256545338261731 ) ) ;
#2496 = CARTESIAN_POINT ( 'NONE',  ( -15.77377628421712252, -287.6869322676240017, -340.4787815142049112 ) ) ;
#2497 = CARTESIAN_POINT ( 'NONE',  ( 7.406912897105986104, -59.46167575493636548, -354.1292707482897413 ) ) ;
#2498 = EDGE_LOOP ( 'NONE', ( #7623, #46944, #48481, #11345, #33708, #19609, #82707 ) ) ;
#2499 = CARTESIAN_POINT ( 'NONE',  ( 18.20392823275637539, -286.8490286691834399, -322.8329148141617679 ) ) ;
#2500 = CARTESIAN_POINT ( 'NONE',  ( 2.462092760079154452, -286.2687590341921577, -209.1422846185902529 ) ) ;
#2501 = ORIENTED_EDGE ( 'NONE', *, *, #85025, .T. ) ;
#2502 = CARTESIAN_POINT ( 'NONE',  ( -52.84164399697896641, -284.3258424455721070, -345.5236060886878136 ) ) ;
#2503 = CARTESIAN_POINT ( 'NONE',  ( -0.5392800613394916898, -274.8890477393947549, -207.2777563747063425 ) ) ;
#2504 = CARTESIAN_POINT ( 'NONE',  ( -70.75058481462328075, -290.5420937758617015, -201.3296835817472470 ) ) ;
#2505 = CARTESIAN_POINT ( 'NONE',  ( 39.17755701731379503, -282.3054800828855377, -278.4994843734720575 ) ) ;
#2506 = CARTESIAN_POINT ( 'NONE',  ( 37.57030566641581260, -282.8889962433487426, -255.8387510213572114 ) ) ;
#2507 = CARTESIAN_POINT ( 'NONE',  ( 37.65593532437416258, -281.6677040430466832, -252.9510138777561394 ) ) ;
#2508 = ADVANCED_FACE ( 'NONE', ( #7499 ), #66273, .F. ) ;
#2509 = CARTESIAN_POINT ( 'NONE',  ( -22.19440711724928050, -280.2514718432173595, -198.8980604804226289 ) ) ;
#2510 = CARTESIAN_POINT ( 'NONE',  ( -6.998514795304330072, -292.1237833571632336, -333.4427485647536855 ) ) ;
#2511 = CARTESIAN_POINT ( 'NONE',  ( -12.44406248820926209, -91.84162952613797870, -360.1898987475070157 ) ) ;
#2512 = EDGE_LOOP ( 'NONE', ( #77006, #1795, #22729, #21511 ) ) ;
#2513 = CARTESIAN_POINT ( 'NONE',  ( 30.74374590970317911, -277.1423916912688696, -239.1810597560504732 ) ) ;
#2514 = CARTESIAN_POINT ( 'NONE',  ( 201.3707903610551284, 293.7126099848096032, -83.13998816544706472 ) ) ;
#2515 = CARTESIAN_POINT ( 'NONE',  ( 29.26011548929556128, -279.1233857181673557, -236.5411674088905727 ) ) ;
#2516 = CARTESIAN_POINT ( 'NONE',  ( -96.96107154359567915, -296.4906081440020102, -228.0595433029909884 ) ) ;
#2517 = CARTESIAN_POINT ( 'NONE',  ( 39.44027207793104850, -293.1308958315894415, -276.0408537448790867 ) ) ;
#2518 = CARTESIAN_POINT ( 'NONE',  ( -87.90885014101696981, -230.0150033563139402, -344.6602624353737951 ) ) ;
#2520 = CARTESIAN_POINT ( 'NONE',  ( -50.91841670740115688, -287.6282379403374421, -342.9537902857447875 ) ) ;
#2519 = CARTESIAN_POINT ( 'NONE',  ( -113.0537791265368242, -271.3799681904797581, -259.0012581418058630 ) ) ;
#2521 = CARTESIAN_POINT ( 'NONE',  ( -4.982016089098304512, -296.4819271545327979, -337.1862143980148971 ) ) ;
#2522 = CARTESIAN_POINT ( 'NONE',  ( 19.02931575992503355, -288.2022787021525119, -223.1869628898460292 ) ) ;
#2523 = ORIENTED_EDGE ( 'NONE', *, *, #63231, .F. ) ;
#2524 = CARTESIAN_POINT ( 'NONE',  ( 39.26821225858289921, -294.5642641755329691, -276.0098559517900298 ) ) ;
#2525 = CARTESIAN_POINT ( 'NONE',  ( -95.00949098850031760, -285.6762450448375716, -225.4808599488853531 ) ) ;
#2526 = CARTESIAN_POINT ( 'NONE',  ( -20.60231402624690134, -297.0522746590115162, -193.7615258097368383 ) ) ;
#2527 = CARTESIAN_POINT ( 'NONE',  ( 27.90981592257615418, -293.8219320403491110, -229.6847659620191280 ) ) ;
#2528 = CARTESIAN_POINT ( 'NONE',  ( 13.23330608872579361, -293.2297999278542875, -212.3809864784209367 ) ) ;
#2529 = CARTESIAN_POINT ( 'NONE',  ( -37.26588755854434254, -289.2178574890489244, -343.3610786469021718 ) ) ;
#2530 = ORIENTED_EDGE ( 'NONE', *, *, #24991, .T. ) ;
#2531 = FACE_OUTER_BOUND ( 'NONE', #25162, .T. ) ;
#2532 = CARTESIAN_POINT ( 'NONE',  ( -112.9026085236913275, -274.5078588213003172, -267.5716711293979415 ) ) ;
#2533 = CARTESIAN_POINT ( 'NONE',  ( -43.99290773345275340, -272.7649013582303041, -193.9944547808171933 ) ) ;
#2534 = CARTESIAN_POINT ( 'NONE',  ( 22.77107744012160850, -281.1920887869873127, -312.1924748982626738 ) ) ;
#2535 = VERTEX_POINT ( 'NONE', #9822 ) ;
#2536 = ORIENTED_EDGE ( 'NONE', *, *, #16849, .T. ) ;
#2537 = CARTESIAN_POINT ( 'NONE',  ( -71.54912814171433411, -276.9996013626940794, -339.2768547356664044 ) ) ;
#2538 = CARTESIAN_POINT ( 'NONE',  ( -107.0554866604049522, -271.2705947266883868, -246.1448345789588643 ) ) ;
#2539 = CARTESIAN_POINT ( 'NONE',  ( -86.31654927378168907, -281.2242287095804159, -214.5728608944492635 ) ) ;
#2540 = CARTESIAN_POINT ( 'NONE',  ( -29.60790894028053089, -275.0929057533552395, -344.2441374449350633 ) ) ;
#2541 = CARTESIAN_POINT ( 'NONE',  ( -110.6373970823285475, -297.7066383063740318, -274.2174519674525186 ) ) ;
#2542 = CARTESIAN_POINT ( 'NONE',  ( -64.66767662082524737, -274.6276639750179811, -202.4012952673230359 ) ) ;
#2543 = CARTESIAN_POINT ( 'NONE',  ( -109.1516566367420751, -274.6296933770493638, -245.5155115500938621 ) ) ;
#2544 = CARTESIAN_POINT ( 'NONE',  ( -31.36483227772994553, -272.1473641846681062, -195.2303203988417977 ) ) ;
#2545 = CARTESIAN_POINT ( 'NONE',  ( -0.6996809299530281079, -295.2033419772033653, -333.6743699023965064 ) ) ;
#2546 = CARTESIAN_POINT ( 'NONE',  ( 33.88304251360246155, -291.8845381301766793, -251.8567683817265959 ) ) ;
#2547 = CYLINDRICAL_SURFACE ( 'NONE', #81948, 2.000000000000010658 ) ;
#2548 = CARTESIAN_POINT ( 'NONE',  ( -37.12084208011064135, -277.5417658976462576, -347.3123111203240114 ) ) ;
#2549 = CARTESIAN_POINT ( 'NONE',  ( -106.3070804325457033, -273.0371183426586299, -246.4283721317634388 ) ) ;
#2550 = CARTESIAN_POINT ( 'NONE',  ( -24.63210283262489853, -281.5781880969284430, -345.8586685824480469 ) ) ;
#2551 = CARTESIAN_POINT ( 'NONE',  ( 0.8601589686108198629, -296.5439030361696382, -335.0963200612210358 ) ) ;
#2552 = DIRECTION ( 'NONE',  ( -0.000000000000000000, -0.000000000000000000, 1.000000000000000000 ) ) ;
#2553 = CARTESIAN_POINT ( 'NONE',  ( -99.17296782236479658, -283.2089455778507272, -309.5647525014836674 ) ) ;
#2554 = CARTESIAN_POINT ( 'NONE',  ( -92.11352308361404084, -281.8321099972962998, -321.8588820916905320 ) ) ;
#2555 = CARTESIAN_POINT ( 'NONE',  ( 34.46425203079156319, -274.3383407293333676, -286.5205346050232720 ) ) ;
#2556 = CARTESIAN_POINT ( 'NONE',  ( 37.70456885433146965, -283.5635385328668008, -271.2350607696074007 ) ) ;
#2557 = CARTESIAN_POINT ( 'NONE',  ( 114.7448031289451222, -299.5541904835127980, -195.3611179825600175 ) ) ;
#2558 = CARTESIAN_POINT ( 'NONE',  ( 204.6539576904058606, 287.9062406767683910, -59.00000000000003553 ) ) ;
#2559 = CARTESIAN_POINT ( 'NONE',  ( -24.27651914122143140, -272.6160209731764894, -195.2359364707425868 ) ) ;
#2560 = CARTESIAN_POINT ( 'NONE',  ( -111.1996555297763507, -280.7321098390859220, -256.3268153080034608 ) ) ;
#2561 = CARTESIAN_POINT ( 'NONE',  ( 114.7448031289451222, -299.5541904835127980, -195.3611179825600175 ) ) ;
#2562 = CARTESIAN_POINT ( 'NONE',  ( 1.970543960950341456, -288.4941262155559230, -205.8331266759901439 ) ) ;
#2563 = CARTESIAN_POINT ( 'NONE',  ( 155.0786878258419392, 18.48484813926942749, -9.250287988715951926 ) ) ;
#2564 = CARTESIAN_POINT ( 'NONE',  ( -101.6889802861403069, -289.0689421451108387, -231.7330867662568323 ) ) ;
#2565 = CARTESIAN_POINT ( 'NONE',  ( 82.12944418934898749, -301.0792019753940849, -196.6542615346262153 ) ) ;
#2566 = CARTESIAN_POINT ( 'NONE',  ( -94.26015771298604307, -294.6945015618919115, -316.7211354578644773 ) ) ;
#2567 = CARTESIAN_POINT ( 'NONE',  ( -96.77117493611734744, -288.0774781237683442, -314.8683269722934597 ) ) ;
#2568 = CARTESIAN_POINT ( 'NONE',  ( -109.0101294763935016, -268.7602059993127455, -295.2240039188629339 ) ) ;
#2569 = CARTESIAN_POINT ( 'NONE',  ( -58.44376093788498139, -295.7791764765509015, -198.3909597514329732 ) ) ;
#2570 = CARTESIAN_POINT ( 'NONE',  ( 18.12740474629692500, -286.7541943026544686, -322.7623217568016685 ) ) ;
#2571 = CARTESIAN_POINT ( 'NONE',  ( 31.08381006476750485, -283.5184984801657038, -298.0087212848238778 ) ) ;
#2572 = CARTESIAN_POINT ( 'NONE',  ( -67.50005802522657916, -281.6822348504491060, -340.1067089858914869 ) ) ;
#2573 = AXIS2_PLACEMENT_3D ( 'NONE', #3290, #26948, #69567 ) ;
#2574 = CARTESIAN_POINT ( 'NONE',  ( -38.89757915434391577, -292.0320934581004622, -197.3777004107880089 ) ) ;
#2575 = CARTESIAN_POINT ( 'NONE',  ( 35.06847423779945672, -283.1500458241283695, -283.5520949548027829 ) ) ;
#2576 = CARTESIAN_POINT ( 'NONE',  ( -10.90790624518023755, -283.5014575384147975, -338.6339987839949686 ) ) ;
#2577 = CARTESIAN_POINT ( 'NONE',  ( -40.24949435402463394, -291.0683929303470450, -345.6730011116519563 ) ) ;
#2578 = CARTESIAN_POINT ( 'NONE',  ( 53.58540442190474096, -299.3278094806844365, -193.3585760710489296 ) ) ;
#2579 = CARTESIAN_POINT ( 'NONE',  ( -71.28197762215567934, -287.5766138327124963, -337.8694268440394239 ) ) ;
#2580 = CARTESIAN_POINT ( 'NONE',  ( 39.55433251004694739, -275.4906040140362506, -265.4397775109711688 ) ) ;
#2581 = CARTESIAN_POINT ( 'NONE',  ( -80.50183842382482169, -293.4442452339447414, -209.3957841586187669 ) ) ;
#2582 = FACE_OUTER_BOUND ( 'NONE', #23796, .T. ) ;
#2583 = CARTESIAN_POINT ( 'NONE',  ( -37.30987171927208124, -285.5519495502701943, -345.3611179825600175 ) ) ;
#2584 = CARTESIAN_POINT ( 'NONE',  ( -112.4026414192340582, -276.5009297402772859, -274.3465309319217909 ) ) ;
#2585 = CARTESIAN_POINT ( 'NONE',  ( 175.2296996224750103, 133.0000000000000000, 24.00000000000001066 ) ) ;
#2586 = CARTESIAN_POINT ( 'NONE',  ( -36.88214745873715117, -296.4576934405298516, -194.1612352087267084 ) ) ;
#2587 = CARTESIAN_POINT ( 'NONE',  ( -30.75565191114682051, -293.7369253260489472, -196.8555781642556894 ) ) ;
#2588 = CARTESIAN_POINT ( 'NONE',  ( -83.24816674809036954, -272.7523357296409472, -213.4709695358284307 ) ) ;
#2589 = CARTESIAN_POINT ( 'NONE',  ( -98.67710828325509453, -291.5102581345895487, -311.2335064567484437 ) ) ;
#2590 = CARTESIAN_POINT ( 'NONE',  ( -33.50806778203349268, -293.0428103764843399, -197.2136983412937639 ) ) ;
#2591 = CARTESIAN_POINT ( 'NONE',  ( -106.5199209340004671, -286.6587904436104282, -244.0486156681365060 ) ) ;
#2592 = CARTESIAN_POINT ( 'NONE',  ( -96.13719915801695493, -292.6388694983503456, -221.5382730703051664 ) ) ;
#2593 = CARTESIAN_POINT ( 'NONE',  ( -97.96781482763074678, -292.4942450918965164, -223.6733031492414057 ) ) ;
#2594 = CARTESIAN_POINT ( 'NONE',  ( -47.79513500865209608, -295.0219697449707041, -342.6600672993502030 ) ) ;
#2595 = CARTESIAN_POINT ( 'NONE',  ( 29.42735459738318937, -289.0992210889988883, -236.0868579360104320 ) ) ;
#2596 = CARTESIAN_POINT ( 'NONE',  ( 35.32698080185477352, -281.3958981561121959, -244.7408750858148210 ) ) ;
#2597 = CARTESIAN_POINT ( 'NONE',  ( -37.57814693287620145, -296.1290649032766282, -194.8014839469518336 ) ) ;
#2598 = CARTESIAN_POINT ( 'NONE',  ( -114.1516837733771297, -284.4619489567068058, -264.2461254498870176 ) ) ;
#2599 = CARTESIAN_POINT ( 'NONE',  ( 29.31909782075390680, -277.0862027302344472, -236.7726554332141404 ) ) ;
#2600 = CARTESIAN_POINT ( 'NONE',  ( -30.47895674286609236, -284.9356444255347469, -197.2345115044694808 ) ) ;
#2601 = CARTESIAN_POINT ( 'NONE',  ( 33.18288295963861856, -285.8846397858544037, -296.0323353182214987 ) ) ;
#2602 = CARTESIAN_POINT ( 'NONE',  ( -59.32954263216747393, -275.4734228370343203, -342.8651886295908184 ) ) ;
#2603 = DIRECTION ( 'NONE',  ( 0.000000000000000000, 0.000000000000000000, -1.000000000000000000 ) ) ;
#2604 = CARTESIAN_POINT ( 'NONE',  ( -32.14757809627998597, -282.4925156143311256, -343.2377914661568639 ) ) ;
#2605 = CARTESIAN_POINT ( 'NONE',  ( -98.26991588888164131, -280.3795870676837012, -223.9095691879708738 ) ) ;
#2606 = CARTESIAN_POINT ( 'NONE',  ( 26.94727416595988601, -286.0581247976591044, -228.4117676061393354 ) ) ;
#2607 = CARTESIAN_POINT ( 'NONE',  ( -12.64933399778398559, -296.4869600891081518, -340.1880473644476979 ) ) ;
#2608 = CARTESIAN_POINT ( 'NONE',  ( 10.04466864528783354, -278.0119495135026000, -330.1023947800194946 ) ) ;
#2609 = ADVANCED_FACE ( 'NONE', ( #60040, #80389 ), #58637, .T. ) ;
#2610 = CARTESIAN_POINT ( 'NONE',  ( 37.42732865843625234, -277.0721754823205174, -286.6362892232604054 ) ) ;
#2612 = EDGE_CURVE ( 'NONE', #10377, #82490, #8425, .T. ) ;
#2611 = CARTESIAN_POINT ( 'NONE',  ( -76.35761310689036918, -277.4227705535585642, -332.1195040930644495 ) ) ;
#2613 = CARTESIAN_POINT ( 'NONE',  ( -111.9865001276049412, -274.5317257338260788, -270.3862691793228805 ) ) ;
#2614 = CARTESIAN_POINT ( 'NONE',  ( 34.80335845759631752, -285.2957740370831630, -250.4835187737770639 ) ) ;
#2615 = CARTESIAN_POINT ( 'NONE',  ( -95.76443986161672228, -291.4867524763847655, -319.3019374003989697 ) ) ;
#2616 = CARTESIAN_POINT ( 'NONE',  ( -37.00789244456584015, -293.9681698002687540, -343.6819476778110811 ) ) ;
#2617 = ORIENTED_EDGE ( 'NONE', *, *, #23208, .F. ) ;
#2618 = CARTESIAN_POINT ( 'NONE',  ( -3.622721304443028867, -292.1768241087224283, -205.5913877535546703 ) ) ;
#2619 = VERTEX_POINT ( 'NONE', #79936 ) ;
#2620 = CARTESIAN_POINT ( 'NONE',  ( -99.61121219932368831, -291.0357986268933246, -315.1496747525023352 ) ) ;
#2621 = CARTESIAN_POINT ( 'NONE',  ( -79.11990784704468638, -280.1231263425738689, -210.3738357661613350 ) ) ;
#2622 = CARTESIAN_POINT ( 'NONE',  ( -112.5827296610251267, -295.6596985770443098, -255.4518117481867137 ) ) ;
#2623 = CARTESIAN_POINT ( 'NONE',  ( 33.95095192629591452, -288.5715524420124893, -299.3243443023405916 ) ) ;
#2624 = CARTESIAN_POINT ( 'NONE',  ( -5.631326695201923194, -288.9796607209196964, -340.5052304109456713 ) ) ;
#2625 = CARTESIAN_POINT ( 'NONE',  ( -64.05915791857650277, -283.7438051644921302, -338.3189353106994872 ) ) ;
#2626 = CARTESIAN_POINT ( 'NONE',  ( -114.0438014765299215, -273.4268578961535354, -284.1485094271377534 ) ) ;
#2627 = CARTESIAN_POINT ( 'NONE',  ( -112.9922304011642495, -269.2718471480555991, -295.9038691064662316 ) ) ;
#2628 = CARTESIAN_POINT ( 'NONE',  ( -70.50382606843994893, -195.7257949056034931, -356.6408436669652247 ) ) ;
#2629 = CARTESIAN_POINT ( 'NONE',  ( 16.64341557793552084, -275.4562902256799362, -319.7580243250421859 ) ) ;
#2630 = CARTESIAN_POINT ( 'NONE',  ( -109.4335942592762052, -277.6472334744765931, -257.0575517376553307 ) ) ;
#2631 = CARTESIAN_POINT ( 'NONE',  ( -78.82658720551361853, -273.1760358027513007, -205.5170863709533364 ) ) ;
#2632 = CARTESIAN_POINT ( 'NONE',  ( -109.1074448185741090, -269.9587199336866661, -295.5484694788251545 ) ) ;
#2633 = CARTESIAN_POINT ( 'NONE',  ( -90.99521459593580630, -276.4792331045256901, -324.9752046622032822 ) ) ;
#2634 = ORIENTED_EDGE ( 'NONE', *, *, #56503, .T. ) ;
#2635 = CARTESIAN_POINT ( 'NONE',  ( -106.6316394200870548, -291.3519773509669903, -247.1901716369108328 ) ) ;
#2636 = CARTESIAN_POINT ( 'NONE',  ( -78.12543314815535211, -298.3213695714580354, -205.2393402026673357 ) ) ;
#2637 = CARTESIAN_POINT ( 'NONE',  ( 32.77912136034463231, -286.5286944658053585, -292.5375017262568917 ) ) ;
#2638 = CARTESIAN_POINT ( 'NONE',  ( -35.48006003109107809, -298.5672192782942602, -193.4225051656221410 ) ) ;
#2639 = CARTESIAN_POINT ( 'NONE',  ( -18.21845782763830357, -294.9654075725447910, -340.8118213743876481 ) ) ;
#2640 = VERTEX_POINT ( 'NONE', #51973 ) ;
#2641 = CARTESIAN_POINT ( 'NONE',  ( 197.1402318696357270, 70.11481179788400198, -10.20567219414501992 ) ) ;
#2642 = CARTESIAN_POINT ( 'NONE',  ( -70.90874729217547667, -279.4117121779906370, -338.0557820761433163 ) ) ;
#2643 = CARTESIAN_POINT ( 'NONE',  ( 4.506962441440763634, -282.0117511107029600, -334.9858077310677800 ) ) ;
#2644 = CARTESIAN_POINT ( 'NONE',  ( -93.33516388618359372, -280.3016055325900879, -223.0241738132965281 ) ) ;
#2645 = CARTESIAN_POINT ( 'NONE',  ( -111.7961672262611614, -280.1190645538988520, -285.6077653152621565 ) ) ;
#2646 = CARTESIAN_POINT ( 'NONE',  ( -109.2067726620527708, -271.2452017205010293, -254.0479605788654851 ) ) ;
#2647 = CARTESIAN_POINT ( 'NONE',  ( 150.7110049404234644, 21.00000000139189638, -5.101169899787367790 ) ) ;
#2648 = CARTESIAN_POINT ( 'NONE',  ( -49.14399963614311417, -280.0642257073692463, -198.3215057486694377 ) ) ;
#2649 = CARTESIAN_POINT ( 'NONE',  ( -104.0943289132476224, -273.8514872881061706, -232.1984954337163742 ) ) ;
#2650 = CARTESIAN_POINT ( 'NONE',  ( -66.77485199109769098, -275.6666780879847352, -201.3778575332219134 ) ) ;
#2651 = CARTESIAN_POINT ( 'NONE',  ( 14.47020840095260574, -274.9153759317688355, -326.5947789362264189 ) ) ;
#2652 = CARTESIAN_POINT ( 'NONE',  ( 197.4027394742815886, 40.84896208771629489, 12.00000000000000711 ) ) ;
#2653 = CARTESIAN_POINT ( 'NONE',  ( -109.8587725886749098, -289.8817878628083804, -260.2967924051071122 ) ) ;
#2654 = CARTESIAN_POINT ( 'NONE',  ( -73.55766334611128343, -284.9334191828816074, -202.4661896362791254 ) ) ;
#2655 = CARTESIAN_POINT ( 'NONE',  ( 28.69552017575814418, -279.3431013164529872, -236.8249705724439025 ) ) ;
#2657 = CARTESIAN_POINT ( 'NONE',  ( -35.88117069322078123, -284.1504598104225465, -195.9354432803787347 ) ) ;
#2656 = CARTESIAN_POINT ( 'NONE',  ( 24.61681697343333042, -280.6728910039685729, -310.1601392661329442 ) ) ;
#2658 = CARTESIAN_POINT ( 'NONE',  ( -94.95184532012282830, -291.8888978003984676, -318.4024147159449285 ) ) ;
#2659 = CARTESIAN_POINT ( 'NONE',  ( 18.25531823328056547, -282.0782529815833186, -222.4241710317243985 ) ) ;
#2660 = CARTESIAN_POINT ( 'NONE',  ( -109.1155130956874899, -270.8344936138795447, -248.4232685986743832 ) ) ;
#2661 = CARTESIAN_POINT ( 'NONE',  ( -35.93461544123370999, -281.4346933404005426, -346.5611091600961231 ) ) ;
#2662 = CARTESIAN_POINT ( 'NONE',  ( 21.61570878164945952, -296.1889464444973328, -316.7393043373006094 ) ) ;
#2663 = CARTESIAN_POINT ( 'NONE',  ( -33.93793638153591274, -278.3342854409783627, -194.4507207524731029 ) ) ;
#2664 = CARTESIAN_POINT ( 'NONE',  ( -105.0392711043689786, -286.9816329592233046, -237.6951217885156780 ) ) ;
#2665 = LINE ( 'NONE', #53304, #8085 ) ;
#2666 = CARTESIAN_POINT ( 'NONE',  ( -55.85998831275767174, -293.7358328630814981, -197.0515634965084359 ) ) ;
#2667 = CARTESIAN_POINT ( 'NONE',  ( 20.71399985140468303, -274.2066185410543540, -317.8633044961467249 ) ) ;
#2668 = CARTESIAN_POINT ( 'NONE',  ( -85.07238799403340579, -288.8888079768875627, -330.6447916969686389 ) ) ;
#2669 = CARTESIAN_POINT ( 'NONE',  ( 23.25634651762551997, -291.3710558232440349, -228.2161990809829035 ) ) ;
#2670 = CARTESIAN_POINT ( 'NONE',  ( -48.18343439339131606, -275.1386486105624272, -431.6459793673298009 ) ) ;
#2671 = CARTESIAN_POINT ( 'NONE',  ( 16.88377877123530268, -274.9440314979038362, -319.9867466582619500 ) ) ;
#2672 = CARTESIAN_POINT ( 'NONE',  ( -58.78733662842336116, -293.4720876267901417, -341.4311549408715223 ) ) ;
#2673 = CARTESIAN_POINT ( 'NONE',  ( -100.7208091274395372, -291.3586604831730824, -307.6679269964687364 ) ) ;
#2674 = DIRECTION ( 'NONE',  ( -1.000000000000000000, -0.000000000000000000, -0.000000000000000000 ) ) ;
#2675 = DIRECTION ( 'NONE',  ( -1.000000000000000000, 0.000000000000000000, 0.000000000000000000 ) ) ;
#2676 = CARTESIAN_POINT ( 'NONE',  ( 36.42133837648591310, -292.2788570749874566, -289.8988226797948187 ) ) ;
#2677 = CARTESIAN_POINT ( 'NONE',  ( -19.64352469057129724, -287.8836886899214846, -198.7146595968324050 ) ) ;
#2678 = CARTESIAN_POINT ( 'NONE',  ( -54.29759832383494711, -287.5067586405085649, -344.4858329171612468 ) ) ;
#2679 = CARTESIAN_POINT ( 'NONE',  ( -11.83462947236000140, -287.8161317901507914, -201.3338460998832602 ) ) ;
#2680 = CARTESIAN_POINT ( 'NONE',  ( 83.14890176555634582, -299.5541904835127980, -193.4651424135224147 ) ) ;
#2681 = CARTESIAN_POINT ( 'NONE',  ( 25.84064955516008055, -288.8613487350610853, -307.3475045084510953 ) ) ;
#2682 = CARTESIAN_POINT ( 'NONE',  ( -30.71004081858468382, -296.9485891865484177, -345.4239443177176554 ) ) ;
#2683 = DIRECTION ( 'NONE',  ( -0.000000000000000000, 1.000000000000000000, -0.000000000000000000 ) ) ;
#2684 = CARTESIAN_POINT ( 'NONE',  ( 19.97936702463683645, -288.0645513802183473, -219.4664596893020132 ) ) ;
#2685 = CARTESIAN_POINT ( 'NONE',  ( -86.18337649788358590, -275.8028604735632143, -328.0820451556562602 ) ) ;
#2686 = CARTESIAN_POINT ( 'NONE',  ( -96.13029495545859504, -278.2155036421382306, -320.0769888323100076 ) ) ;
#2687 = CARTESIAN_POINT ( 'NONE',  ( 19.14753053243669711, -280.5063427849576669, -218.0666525879390747 ) ) ;
#2688 = CARTESIAN_POINT ( 'NONE',  ( -111.3195000378592141, -274.5794567822068757, -262.0786474947299212 ) ) ;
#2689 = CARTESIAN_POINT ( 'NONE',  ( -68.35200798006037815, -283.6446333426938509, -202.0723088026354617 ) ) ;
#2690 = CARTESIAN_POINT ( 'NONE',  ( -48.18343439339133027, -253.8127106430751496, -479.5013660720742905 ) ) ;
#2691 = CARTESIAN_POINT ( 'NONE',  ( -60.08998674262525697, -277.8938816083247616, -199.6430583925055657 ) ) ;
#2692 = CARTESIAN_POINT ( 'NONE',  ( -91.99211653074637240, -281.8321099976639061, -321.7446551986965915 ) ) ;
#2693 = FACE_OUTER_BOUND ( 'NONE', #59104, .T. ) ;
#2694 = CARTESIAN_POINT ( 'NONE',  ( -59.48249724873398492, -275.8136620113664321, -343.3850377219923757 ) ) ;
#2695 = CARTESIAN_POINT ( 'NONE',  ( -110.4902678018330562, -297.9500757429140663, -279.7128525874268803 ) ) ;
#2696 = CARTESIAN_POINT ( 'NONE',  ( 36.17838733200018453, -280.7494716919017037, -292.3677470392498776 ) ) ;
#2697 = CARTESIAN_POINT ( 'NONE',  ( -105.1753486792967323, -297.1248144635013659, -297.9655482751671229 ) ) ;
#2698 = CARTESIAN_POINT ( 'NONE',  ( -46.09021219033369476, -299.2585613696900282, -194.3561062476720451 ) ) ;
#2699 = CARTESIAN_POINT ( 'NONE',  ( -81.08027928402636064, -273.1063478667110758, -211.8252506950797169 ) ) ;
#2700 = CARTESIAN_POINT ( 'NONE',  ( 0.9077138322254096892, -294.5626779567892299, -205.8476854246210337 ) ) ;
#2701 = CARTESIAN_POINT ( 'NONE',  ( 2.739199855610745971, -286.7409349505085174, -204.6152324763273782 ) ) ;
#2702 = CARTESIAN_POINT ( 'NONE',  ( -95.68955208083121988, -277.2894252167806712, -222.3322314468233856 ) ) ;
#2703 = CARTESIAN_POINT ( 'NONE',  ( -82.85435356233550408, -289.4890413853051996, -332.4706855374815291 ) ) ;
#2704 = CARTESIAN_POINT ( 'NONE',  ( -21.08874187012393620, -287.8971944043843223, -341.7701495908441416 ) ) ;
#2705 = CARTESIAN_POINT ( 'NONE',  ( 7.671467575295017660, -290.6659425368728762, -210.3061573505725050 ) ) ;
#2706 = EDGE_LOOP ( 'NONE', ( #8461, #84685, #42920, #69826 ) ) ;
#2707 = CARTESIAN_POINT ( 'NONE',  ( 207.9737475149031525, 296.4638663539913637, -68.98948423471202318 ) ) ;
#2708 = CARTESIAN_POINT ( 'NONE',  ( -37.27425110047372669, -288.5589369964210960, -343.4226255807204211 ) ) ;
#2709 = CARTESIAN_POINT ( 'NONE',  ( 41.08708295871279859, -293.9068999365417199, -472.6442049081569508 ) ) ;
#2710 = CARTESIAN_POINT ( 'NONE',  ( -96.98198631410483017, -284.8429599868558171, -318.7124702920821733 ) ) ;
#2711 = CARTESIAN_POINT ( 'NONE',  ( -19.43000539545679572, -291.3357273645840451, -195.6606881735908132 ) ) ;
#2712 = EDGE_CURVE ( 'NONE', #71577, #17995, #44862, .T. ) ;
#2713 = CARTESIAN_POINT ( 'NONE',  ( -41.52531235935615683, -284.4188357550344790, -346.8054895221640663 ) ) ;
#2714 = APPLICATION_CONTEXT ( 'automotive_design' ) ;
#2715 = CARTESIAN_POINT ( 'NONE',  ( -4.829069549432396968, -282.4448676174676507, -335.7211123016501801 ) ) ;
#2716 = CARTESIAN_POINT ( 'NONE',  ( -111.6220714087064039, -296.8084282231895372, -249.8804470308761552 ) ) ;
#2717 = CARTESIAN_POINT ( 'NONE',  ( 35.19664998397951194, -277.0260885663154795, -282.4771392354473392 ) ) ;
#2718 = CARTESIAN_POINT ( 'NONE',  ( -9.081911065104558034, -290.4434890716537438, -201.2175371920630766 ) ) ;
#2719 = CARTESIAN_POINT ( 'NONE',  ( -62.14954914469169722, -272.5171341220921590, -201.2836170738869157 ) ) ;
#2720 = EDGE_LOOP ( 'NONE', ( #34758, #77144, #38820, #57265 ) ) ;
#2721 = CARTESIAN_POINT ( 'NONE',  ( 194.5881128153457098, 0.000000000000000000, 10.00000000000000178 ) ) ;
#2722 = CARTESIAN_POINT ( 'NONE',  ( -88.70544114177731387, -287.2445392621377209, -216.4808775858933529 ) ) ;
#2723 = CARTESIAN_POINT ( 'NONE',  ( -47.57665820279462565, -296.2590341920533774, -346.3659740272857448 ) ) ;
#2724 = CARTESIAN_POINT ( 'NONE',  ( -103.1007377632841582, -284.7704860687312589, -302.4091723047908431 ) ) ;
#2725 = CARTESIAN_POINT ( 'NONE',  ( -28.63965096828158963, -276.0032425536001597, -346.6844086941429737 ) ) ;
#2726 = CARTESIAN_POINT ( 'NONE',  ( 29.38307255683859154, -293.7062620986482671, -232.1365513208092182 ) ) ;
#2727 = CARTESIAN_POINT ( 'NONE',  ( 22.89406244231098597, -285.0688448791775045, -224.3837900243584045 ) ) ;
#2728 = CARTESIAN_POINT ( 'NONE',  ( 36.35068573455915697, -294.1668587906486891, -292.7942859032173146 ) ) ;
#2729 = CARTESIAN_POINT ( 'NONE',  ( -108.6824671081372031, -290.6793230287998426, -285.9942879991552331 ) ) ;
#2730 = LINE ( 'NONE', #22180, #9659 ) ;
#2731 = CARTESIAN_POINT ( 'NONE',  ( 29.33919985515026596, -285.8906705383787994, 25.50000000000000000 ) ) ;
#2732 = CARTESIAN_POINT ( 'NONE',  ( -62.37129463845912625, -182.9780070361101991, -358.6976082868463891 ) ) ;
#2733 = CARTESIAN_POINT ( 'NONE',  ( -110.0192286520845073, -285.7767764354590554, -293.6567987104924669 ) ) ;
#2734 = CARTESIAN_POINT ( 'NONE',  ( 36.60358173371529489, -278.6237833571632905, -234.7871824221999191 ) ) ;
#2735 = ORIENTED_EDGE ( 'NONE', *, *, #52504, .T. ) ;
#2736 = CARTESIAN_POINT ( 'NONE',  ( -80.82047541408202562, -282.5779316952025511, -329.4481958337401011 ) ) ;
#2737 = CARTESIAN_POINT ( 'NONE',  ( -91.31723784293288304, -277.4609677338074221, -325.3209727301505154 ) ) ;
#2738 = CARTESIAN_POINT ( 'NONE',  ( 35.54026667780902216, -283.3338264541879425, -253.3832693056166079 ) ) ;
#2739 = CARTESIAN_POINT ( 'NONE',  ( -81.56226884185248593, -220.3210169592839520, -351.0985766935151560 ) ) ;
#2740 = CARTESIAN_POINT ( 'NONE',  ( 4.209938585483945062, -281.0789763095443732, -334.5490505033449722 ) ) ;
#2741 = CARTESIAN_POINT ( 'NONE',  ( 7.944381906164617924, -284.6940646746120933, -210.9576313398227398 ) ) ;
#2742 = CARTESIAN_POINT ( 'NONE',  ( -87.24096160769006758, -275.2262057935647590, -213.2793377503666079 ) ) ;
#2743 = CARTESIAN_POINT ( 'NONE',  ( -7.957809596465249768, -295.1488612952133508, -337.2669747142366532 ) ) ;
#2744 = CARTESIAN_POINT ( 'NONE',  ( 23.00236286806038422, -291.6559641898066957, -228.3885197761897246 ) ) ;
#2745 = CARTESIAN_POINT ( 'NONE',  ( -84.79694765792467592, -278.3380713043167702, -330.9375515814594451 ) ) ;
#2746 = CARTESIAN_POINT ( 'NONE',  ( 32.89785625263545654, -275.8155770141138419, -290.2916489331177559 ) ) ;
#2747 = CARTESIAN_POINT ( 'NONE',  ( 33.43361238478622965, -274.0938120734829226, -240.6883679346808265 ) ) ;
#2748 = LINE ( 'NONE', #18829, #53687 ) ;
#2749 = CARTESIAN_POINT ( 'NONE',  ( 29.52501195980105564, -274.0023074647206158, -304.4424623720775571 ) ) ;
#2750 = CARTESIAN_POINT ( 'NONE',  ( -13.94507580407868197, -296.1796593822725185, -343.1017824146418320 ) ) ;
#2751 = DIRECTION ( 'NONE',  ( 0.9531768234071978929, -0.3024135303179465994, 1.424463645888277034E-13 ) ) ;
#2752 = CARTESIAN_POINT ( 'NONE',  ( 200.4551663813218170, 64.49084098419280053, 0.000000000000000000 ) ) ;
#2753 = CARTESIAN_POINT ( 'NONE',  ( -106.4605913472635450, -285.3062854420732037, -294.9417921748872118 ) ) ;
#2754 = CARTESIAN_POINT ( 'NONE',  ( -113.3406613365604159, -286.2808928153247621, -272.8388528738504419 ) ) ;
#2755 = CARTESIAN_POINT ( 'NONE',  ( -72.41564051331070573, -284.9235527089034576, -206.2086614824857804 ) ) ;
#2756 = CARTESIAN_POINT ( 'NONE',  ( 32.00658406916826948, -274.2864893383505773, -295.7534321924774758 ) ) ;
#2757 = CARTESIAN_POINT ( 'NONE',  ( 35.92642766521837672, -283.5675041894049855, -282.3046070428194980 ) ) ;
#2758 = CARTESIAN_POINT ( 'NONE',  ( -18.86159556224215450, -275.2897404266887520, -341.6997014127180705 ) ) ;
#2759 = CARTESIAN_POINT ( 'NONE',  ( -56.66848074325722706, -278.3867687708254266, -341.1294742975649683 ) ) ;
#2760 = CARTESIAN_POINT ( 'NONE',  ( 206.7809450508160865, 35.77530089738195329, 15.00000000000000178 ) ) ;
#2761 = CARTESIAN_POINT ( 'NONE',  ( -82.15299265512079785, -280.2607854637705600, -207.9423156702887354 ) ) ;
#2762 = CARTESIAN_POINT ( 'NONE',  ( -59.29058944443922741, -280.2677606479604719, -196.6198597829484811 ) ) ;
#2763 = ORIENTED_EDGE ( 'NONE', *, *, #44799, .F. ) ;
#2764 = ORIENTED_EDGE ( 'NONE', *, *, #65408, .F. ) ;
#2765 = CARTESIAN_POINT ( 'NONE',  ( 36.90269544335986041, -289.6045155762329841, -285.4632770918300366 ) ) ;
#2766 = CARTESIAN_POINT ( 'NONE',  ( -109.5238969235007715, -295.5922831480214086, -282.2914236355272237 ) ) ;
#2767 = CARTESIAN_POINT ( 'NONE',  ( -82.79907439499299926, -289.0043862434667403, -332.3848224111608829 ) ) ;
#2769 = CARTESIAN_POINT ( 'NONE',  ( -111.1348562872789358, -288.7095986691595044, -276.6946171438947886 ) ) ;
#2768 = CARTESIAN_POINT ( 'NONE',  ( 16.41722005353504699, -285.4095778059436839, -220.0896226530646231 ) ) ;
#2770 = VECTOR ( 'NONE', #13795, 1000.000000000000000 ) ;
#2771 = CARTESIAN_POINT ( 'NONE',  ( 13.40305642130455155, -287.9862516103727330, -217.2617747311107337 ) ) ;
#2772 = CARTESIAN_POINT ( 'NONE',  ( -64.39798358256457789, -275.4049527941206748, -340.3656341580193612 ) ) ;
#2773 = CARTESIAN_POINT ( 'NONE',  ( -17.94780361404993840, -287.2060191304763066, -344.0518039034200797 ) ) ;
#2774 = CARTESIAN_POINT ( 'NONE',  ( -13.36776127044652007, -288.3636626835776156, -199.2960006397966310 ) ) ;
#2775 = CARTESIAN_POINT ( 'NONE',  ( -69.86933689767057842, -287.4792636309319960, -338.1394199468418265 ) ) ;
#2776 = CARTESIAN_POINT ( 'NONE',  ( -56.36851980457477396, -284.2446842523890496, -341.0816141660307608 ) ) ;
#2777 = CARTESIAN_POINT ( 'NONE',  ( -105.6063829402270642, -292.9660349814196820, -238.7733616052207140 ) ) ;
#2778 = CARTESIAN_POINT ( 'NONE',  ( 82.16487609371904455, -298.2963867135958935, -193.7956126067913658 ) ) ;
#2779 = CARTESIAN_POINT ( 'NONE',  ( 156.4851178187871312, 1.000000000000000000, -7.000000000000000888 ) ) ;
#2780 = CARTESIAN_POINT ( 'NONE',  ( -75.08227273479333519, -299.4740249117562598, -204.8414279612577786 ) ) ;
#2781 = CARTESIAN_POINT ( 'NONE',  ( -36.99732744133339679, -279.2537393160829993, -197.2004513985829135 ) ) ;
#2782 = CARTESIAN_POINT ( 'NONE',  ( 31.87685371402460532, -279.1749930218220470, -241.4856534825018741 ) ) ;
#2783 = CARTESIAN_POINT ( 'NONE',  ( 38.65532623992585570, -292.8914511685017033, -281.7017883206525539 ) ) ;
#2784 = CARTESIAN_POINT ( 'NONE',  ( -97.08625777033148552, -271.3964263819379426, -226.5889108564023218 ) ) ;
#2785 = CARTESIAN_POINT ( 'NONE',  ( 21.13884602993729445, -274.2693853264119070, -316.4396442319369385 ) ) ;
#2786 = CARTESIAN_POINT ( 'NONE',  ( -97.57803656960989258, -297.2841462128938588, -312.4660731617087208 ) ) ;
#2787 = FILL_AREA_STYLE_COLOUR ( '', #85218 ) ;
#2788 = CARTESIAN_POINT ( 'NONE',  ( -9.406579345672197334, -296.8757723994409616, -194.0615142604495134 ) ) ;
#2789 = CARTESIAN_POINT ( 'NONE',  ( 36.79030919207632166, -292.0042241912066743, -287.1056707402462962 ) ) ;
#2790 = CARTESIAN_POINT ( 'NONE',  ( -52.50879800661054730, -293.2794828443963411, -198.2995316729631838 ) ) ;
#2791 = CARTESIAN_POINT ( 'NONE',  ( 138.6539576904058606, 250.5000000000000568, -10.49999999999999822 ) ) ;
#2792 = CARTESIAN_POINT ( 'NONE',  ( 28.54441147741274065, -294.7858595178612973, -302.2839908343195248 ) ) ;
#2793 = DIRECTION ( 'NONE',  ( 0.000000000000000000, 0.000000000000000000, -1.000000000000000000 ) ) ;
#2795 = CARTESIAN_POINT ( 'NONE',  ( 8.228166959662209123, -294.4088991144729448, -327.4557880836728145 ) ) ;
#2794 = CARTESIAN_POINT ( 'NONE',  ( -69.78531745579915935, -281.4972470165252503, -338.3886424621617834 ) ) ;
#2796 = CARTESIAN_POINT ( 'NONE',  ( 11.49260014145638031, -282.3965537359416658, -329.9633923317568360 ) ) ;
#2797 = CARTESIAN_POINT ( 'NONE',  ( 36.26899276346060219, -283.2543199970677961, -253.2520769356646042 ) ) ;
#2798 = CARTESIAN_POINT ( 'NONE',  ( -85.49637932775860349, -285.0734653645772596, -210.3038855903564013 ) ) ;
#2799 = CARTESIAN_POINT ( 'NONE',  ( -111.9526576019002704, -288.4696180730693413, -276.7619910168854744 ) ) ;
#2800 = CARTESIAN_POINT ( 'NONE',  ( 38.18225885682601728, -280.1696088025414042, -281.2624652323590908 ) ) ;
#2801 = CARTESIAN_POINT ( 'NONE',  ( 23.95457119407326019, -285.6771258154308271, -229.7225497859528787 ) ) ;
#2802 = CARTESIAN_POINT ( 'NONE',  ( 12.20560971778196091, -287.3014911065483830, -328.8979149220623412 ) ) ;
#2803 = DIRECTION ( 'NONE',  ( 0.9764705882352960886, 0.000000000000000000, -0.2156506209390900708 ) ) ;
#2804 = CARTESIAN_POINT ( 'NONE',  ( -45.15539717101938777, -296.7527448739286910, -343.7973404873493450 ) ) ;
#2805 = CARTESIAN_POINT ( 'NONE',  ( -79.88295558156283960, -279.0401950349207709, -333.8980084025261021 ) ) ;
#2808 = EDGE_CURVE ( 'NONE', #31000, #20790, #31154, .T. ) ;
#2807 = CARTESIAN_POINT ( 'NONE',  ( -74.51289745166468492, -279.2100307053224242, -207.4508765930658285 ) ) ;
#2806 = CARTESIAN_POINT ( 'NONE',  ( 36.45459683255092642, -291.7671284948152675, -285.6095067920849715 ) ) ;
#2809 = CARTESIAN_POINT ( 'NONE',  ( 4.139746364101549503, -292.7609560338043480, -205.4265875402523989 ) ) ;
#2810 = CARTESIAN_POINT ( 'NONE',  ( -62.69480716997583158, -283.8045586427365947, -199.1815270844266763 ) ) ;
#2811 = CARTESIAN_POINT ( 'NONE',  ( -50.92474409682142777, -279.2258922889168957, -344.1208736928884377 ) ) ;
#2812 = ADVANCED_FACE ( 'NONE', ( #59099 ), #42773, .T. ) ;
#2813 = CARTESIAN_POINT ( 'NONE',  ( -47.83857301979428200, -294.2475225237496375, -342.8916930074684615 ) ) ;
#2814 = CARTESIAN_POINT ( 'NONE',  ( -54.12226128174090434, -295.8364965076098656, -197.2624626393473477 ) ) ;
#2815 = ORIENTED_EDGE ( 'NONE', *, *, #63406, .F. ) ;
#2816 = DIRECTION ( 'NONE',  ( 0.000000000000000000, 1.000000000000000000, 0.000000000000000000 ) ) ;
#2817 = CARTESIAN_POINT ( 'NONE',  ( 37.15999247101181169, -283.4724467757494040, -265.7410963307617067 ) ) ;
#2818 = CARTESIAN_POINT ( 'NONE',  ( -94.82573711846927722, -295.4244564360678282, -315.4562832795411964 ) ) ;
#2819 = LINE ( 'NONE', #65859, #32252 ) ;
#2820 = CARTESIAN_POINT ( 'NONE',  ( -54.49178911615187104, -274.7666405000204577, -345.3538533559490702 ) ) ;
#2821 = CARTESIAN_POINT ( 'NONE',  ( -36.17674695991064482, -297.1251560531955533, -193.5965911883371859 ) ) ;
#2822 = CARTESIAN_POINT ( 'NONE',  ( -9.725616075764879298, -290.0139872273785500, -341.7099103643789704 ) ) ;
#2823 = CARTESIAN_POINT ( 'NONE',  ( -50.75354785169238170, -289.0614556014573964, -342.1701823921899290 ) ) ;
#2824 = CARTESIAN_POINT ( 'NONE',  ( -93.63221653140652734, -280.7419848737471852, -222.7803136771873085 ) ) ;
#2825 = CARTESIAN_POINT ( 'NONE',  ( -109.3196191172755221, -274.3649467318228972, -254.0632777641390021 ) ) ;
#2826 = CARTESIAN_POINT ( 'NONE',  ( -7.825759062145887235, -279.2426718483865784, -203.1466276485403739 ) ) ;
#2827 = EDGE_LOOP ( 'NONE', ( #72963, #56833, #41843, #30949, #88679 ) ) ;
#2828 = CARTESIAN_POINT ( 'NONE',  ( -70.71603551743220351, -297.2906472624725325, -200.9932721964837867 ) ) ;
#2829 = CARTESIAN_POINT ( 'NONE',  ( -49.95634484765677286, -293.8102664243620552, -196.9454017739848837 ) ) ;
#2830 = CARTESIAN_POINT ( 'NONE',  ( 209.7827226070571385, 36.64741339240061535, 13.08022668053247983 ) ) ;
#2831 = ADVANCED_FACE ( 'NONE', ( #87479 ), #44889, .F. ) ;
#2832 = CARTESIAN_POINT ( 'NONE',  ( -104.8003338258955068, -291.5824069597491075, -242.0650969702264774 ) ) ;
#2833 = CARTESIAN_POINT ( 'NONE',  ( 209.7513585654923816, 282.2246705312486483, -40.00000000000000711 ) ) ;
#2834 = CARTESIAN_POINT ( 'NONE',  ( -8.951720534258400974, -290.5591488951637302, -200.1164417439935903 ) ) ;
#2835 = AXIS2_PLACEMENT_3D ( 'NONE', #93040, #42369, #58009 ) ;
#2836 = CARTESIAN_POINT ( 'NONE',  ( -49.95340010446486190, -297.5534975373815882, -198.4373214309470370 ) ) ;
#2837 = FACE_OUTER_BOUND ( 'NONE', #66330, .T. ) ;
#2838 = CARTESIAN_POINT ( 'NONE',  ( 196.1862243335229721, 25.40468116510840701, 14.05651170788187443 ) ) ;
#2839 = CARTESIAN_POINT ( 'NONE',  ( -96.05788420657935944, -292.7337038235289697, -221.6057418116824920 ) ) ;
#2840 = CARTESIAN_POINT ( 'NONE',  ( -119.3990491898856732, -287.0519495502701943, -270.3937649182068412 ) ) ;
#2841 = CARTESIAN_POINT ( 'NONE',  ( 1.088840022142868680, -288.5661438620001036, -206.0891764034962819 ) ) ;
#2842 = CARTESIAN_POINT ( 'NONE',  ( -9.325044589421599639, -274.6849535557645936, -339.7659108541024011 ) ) ;
#2843 = CARTESIAN_POINT ( 'NONE',  ( 34.23804555264609206, -277.2051688667561962, -249.7405601132960840 ) ) ;
#2844 = CARTESIAN_POINT ( 'NONE',  ( -70.84739378904981777, -289.6864163923318074, -203.8879452476151926 ) ) ;
#2845 = CARTESIAN_POINT ( 'NONE',  ( -100.8686835716760726, -280.9646906277680500, -228.9790026064348467 ) ) ;
#2846 = ORIENTED_EDGE ( 'NONE', *, *, #39352, .F. ) ;
#2847 = EDGE_CURVE ( 'NONE', #37463, #46977, #66092, .T. ) ;
#2848 = CARTESIAN_POINT ( 'NONE',  ( -64.10039669164578413, -282.7592697003752846, -338.3895298887953231 ) ) ;
#2849 = CARTESIAN_POINT ( 'NONE',  ( -93.09976414047308424, -278.9092381510017162, -323.0921328405184454 ) ) ;
#2850 = CARTESIAN_POINT ( 'NONE',  ( 1.187602918908520655, -279.3492116665115077, -204.0927027560734643 ) ) ;
#2851 = CARTESIAN_POINT ( 'NONE',  ( -71.49185695405026308, -195.2781849387351940, -357.0959408212342510 ) ) ;
#2852 = CARTESIAN_POINT ( 'NONE',  ( 27.45667162853909105, -277.0355815205247723, -311.6180747683662275 ) ) ;
#2853 = CARTESIAN_POINT ( 'NONE',  ( -67.28160103364130862, -275.1867171468312563, -200.1734403777877844 ) ) ;
#2854 = CARTESIAN_POINT ( 'NONE',  ( -92.08974858914540107, -275.6948066931273047, -226.7417163044926838 ) ) ;
#2855 = ORIENTED_EDGE ( 'NONE', *, *, #52014, .F. ) ;
#2856 = CARTESIAN_POINT ( 'NONE',  ( -78.33593093052400036, -290.6974386804960204, -331.1980336568678922 ) ) ;
#2857 = CARTESIAN_POINT ( 'NONE',  ( -45.88922343606126475, -290.9191123339097089, -345.9179412343022477 ) ) ;
#2858 = CARTESIAN_POINT ( 'NONE',  ( -65.35836473592824802, -291.0245960728885848, -202.8275208056123233 ) ) ;
#2859 = CARTESIAN_POINT ( 'NONE',  ( 2.714328192050878830, -286.0820139869255740, -204.6721425118038837 ) ) ;
#2860 = CARTESIAN_POINT ( 'NONE',  ( -29.37836264791282304, -281.3496091152964027, -343.7812803602099621 ) ) ;
#2861 = CARTESIAN_POINT ( 'NONE',  ( -5.237154793796259256, -290.4854685085708752, -337.2951426109901263 ) ) ;
#2862 = CARTESIAN_POINT ( 'NONE',  ( -91.26183937304736560, -282.3164937269717711, -320.5938397536647244 ) ) ;
#2863 = CARTESIAN_POINT ( 'NONE',  ( 15.60310234595508128, -282.1355650153560646, -219.3169602091612376 ) ) ;
#2864 = CARTESIAN_POINT ( 'NONE',  ( 36.56115665267015657, -288.7549626652714778, -291.1744180273909137 ) ) ;
#2865 = CARTESIAN_POINT ( 'NONE',  ( -103.4281870388300462, -279.4665099721584625, -239.0882953529059591 ) ) ;
#2866 = CARTESIAN_POINT ( 'NONE',  ( 8.624982094127268795, -291.4608993500235670, -209.0162564729106123 ) ) ;
#2867 = CARTESIAN_POINT ( 'NONE',  ( 37.21765845827852814, -288.1220925132266188, -251.7853039135123367 ) ) ;
#2868 = CARTESIAN_POINT ( 'NONE',  ( 1.485204760623171083, -287.0488303815515678, -203.9229172603655513 ) ) ;
#2869 = CARTESIAN_POINT ( 'NONE',  ( -61.53272083558573513, -283.5419036321370072, -339.2895632518391835 ) ) ;
#2870 = VERTEX_POINT ( 'NONE', #43934 ) ;
#2871 = FACE_OUTER_BOUND ( 'NONE', #72138, .T. ) ;
#2872 = CARTESIAN_POINT ( 'NONE',  ( -5.150820151708191297, -294.3317621872541281, -201.7750207701828344 ) ) ;
#2873 = CARTESIAN_POINT ( 'NONE',  ( 38.74476234958408583, -292.3439164272979269, -278.8568525136179801 ) ) ;
#2874 = CARTESIAN_POINT ( 'NONE',  ( 15.76026168670163408, -275.3356033178822599, -320.7951352683645041 ) ) ;
#2875 = CARTESIAN_POINT ( 'NONE',  ( -95.48856867577825369, -296.5821054423128658, -219.9601463135191750 ) ) ;
#2876 = CARTESIAN_POINT ( 'NONE',  ( 11.40379034033410299, -291.2220414918509164, -215.0247091504053571 ) ) ;
#2877 = CARTESIAN_POINT ( 'NONE',  ( -107.6626292927897737, -295.0961193701960497, -247.1132791505773412 ) ) ;
#2878 = CARTESIAN_POINT ( 'NONE',  ( -62.95358841780969783, -292.9161529783538640, -201.5776775115582211 ) ) ;
#2879 = CARTESIAN_POINT ( 'NONE',  ( -4.707777516483687918, -293.5720805570799143, -204.7022333330794197 ) ) ;
#2880 = CARTESIAN_POINT ( 'NONE',  ( 208.4207707293412852, 35.83328680606452821, 15.07795544555653855 ) ) ;
#2881 = CARTESIAN_POINT ( 'NONE',  ( -11.70697373698338950, -292.7191181847800863, -341.0767123416845266 ) ) ;
#2882 = CARTESIAN_POINT ( 'NONE',  ( -93.46545006823660628, -299.2444835154307725, -220.5913497278921795 ) ) ;
#2883 = CARTESIAN_POINT ( 'NONE',  ( 32.49436237846204989, -288.2015092053195531, -248.2662015151656192 ) ) ;
#2884 = CARTESIAN_POINT ( 'NONE',  ( -20.46931860436149009, -278.8165469422323213, -343.8566872408301265 ) ) ;
#2885 = CARTESIAN_POINT ( 'NONE',  ( -41.37894363133016640, -275.8968223335654670, -346.8707251310198103 ) ) ;
#2886 = CARTESIAN_POINT ( 'NONE',  ( -94.06446177829603528, -272.6080721097270043, -218.4201888353314018 ) ) ;
#2887 = CARTESIAN_POINT ( 'NONE',  ( -2.977954173149480077, -280.6743074147379957, -336.4090794574188976 ) ) ;
#2888 = CARTESIAN_POINT ( 'NONE',  ( -95.55139297034149592, -276.2824067017272682, -319.5551605005184683 ) ) ;
#2889 = EDGE_CURVE ( 'NONE', #67382, #91332, #11583, .T. ) ;
#2890 = CARTESIAN_POINT ( 'NONE',  ( -101.6379645964201188, -295.7202586623055822, -234.7628897645957409 ) ) ;
#2891 = DIRECTION ( 'NONE',  ( 0.000000000000000000, 0.000000000000000000, 1.000000000000000000 ) ) ;
#2892 = CARTESIAN_POINT ( 'NONE',  ( 51.90681045958935158, -300.0003654427256947, -197.1871290551031848 ) ) ;
#2893 = CARTESIAN_POINT ( 'NONE',  ( 76.08708295871279859, -296.0521521680024080, -430.6442049081568939 ) ) ;
#2895 = CARTESIAN_POINT ( 'NONE',  ( -62.02769912935531949, -273.5553623970110948, -201.6617623974533160 ) ) ;
#2894 = CARTESIAN_POINT ( 'NONE',  ( -83.24402990789482715, -289.4474636461882824, -210.5343208057203697 ) ) ;
#2896 = CARTESIAN_POINT ( 'NONE',  ( -3.060732189554848492, -288.6118421495224311, -339.3236633873809751 ) ) ;
#2897 = CARTESIAN_POINT ( 'NONE',  ( -94.64693616848038005, -275.2241708497983836, -221.6983236229328043 ) ) ;
#2898 = CARTESIAN_POINT ( 'NONE',  ( -93.19672922290135375, -295.2467577503680900, -220.5590682967963403 ) ) ;
#2899 = CARTESIAN_POINT ( 'NONE',  ( -81.47718342649301349, -282.8326430093590602, -333.3243269062834884 ) ) ;
#2900 = DIRECTION ( 'NONE',  ( 0.000000000000000000, 1.000000000000000000, 0.000000000000000000 ) ) ;
#2901 = CARTESIAN_POINT ( 'NONE',  ( 34.73986262293673377, -279.2832123456855697, -249.4613584316390700 ) ) ;
#2902 = CARTESIAN_POINT ( 'NONE',  ( 197.4375396935993479, 24.88665474053333071, 11.71825508031674445 ) ) ;
#2903 = CARTESIAN_POINT ( 'NONE',  ( -70.38581510824025145, -290.4013790358661140, -204.8232131397174385 ) ) ;
#2904 = CARTESIAN_POINT ( 'NONE',  ( -109.2962303322233026, -282.4547446666628616, -288.6206652414547875 ) ) ;
#2905 = DIRECTION ( 'NONE',  ( -0.000000000000000000, -1.000000000000000000, -9.656854691831248164E-17 ) ) ;
#2906 = CARTESIAN_POINT ( 'NONE',  ( -71.09870476466221589, -289.6064229077545065, -203.3875016063779526 ) ) ;
#2907 = CARTESIAN_POINT ( 'NONE',  ( -87.82220854867985338, -274.8516771856002379, -216.6030027083346852 ) ) ;
#2908 = CARTESIAN_POINT ( 'NONE',  ( 11.25262060570510947, -283.6014355524578150, -329.6463279634551782 ) ) ;
#2910 = CARTESIAN_POINT ( 'NONE',  ( -64.05537194972967541, -283.4105777766824303, -338.2977041332143244 ) ) ;
#2909 = CARTESIAN_POINT ( 'NONE',  ( -82.69584842527063984, -271.5179643175806063, -209.8612594424555198 ) ) ;
#2911 = CARTESIAN_POINT ( 'NONE',  ( 12.15735637397209068, -277.7729995579064735, -324.8840983225068726 ) ) ;
#2912 = CARTESIAN_POINT ( 'NONE',  ( -39.15153233043744052, -277.8782774392157648, -343.5002062653364305 ) ) ;
#2913 = CARTESIAN_POINT ( 'NONE',  ( -3.764762803192364782, -284.6093846415869280, -337.4394659220541257 ) ) ;
#2914 = EDGE_CURVE ( 'NONE', #37641, #1315, #66663, .T. ) ;
#2915 = ORIENTED_EDGE ( 'NONE', *, *, #28070, .F. ) ;
#2916 = DIRECTION ( 'NONE',  ( 0.000000000000000000, 0.000000000000000000, 1.000000000000000000 ) ) ;
#2917 = CARTESIAN_POINT ( 'NONE',  ( -22.09962252229478707, -294.6953883675424777, -345.8374657661136098 ) ) ;
#2918 = CARTESIAN_POINT ( 'NONE',  ( 17.15852877712842073, -288.8141928387911435, -219.3366568809630053 ) ) ;
#2919 = CARTESIAN_POINT ( 'NONE',  ( 196.7904975038847795, 24.97768796420434256, 13.23503237509909880 ) ) ;
#2920 = CARTESIAN_POINT ( 'NONE',  ( 44.71564893372296723, -285.0523547857347353, -270.3937649182068412 ) ) ;
#2921 = CARTESIAN_POINT ( 'NONE',  ( -64.61947273876879194, -278.6246938338379096, -198.6293515077563256 ) ) ;
#2922 = CARTESIAN_POINT ( 'NONE',  ( -108.7172567006733743, -289.2947493576018019, -243.5280846392117269 ) ) ;
#2923 = CARTESIAN_POINT ( 'NONE',  ( -95.51620273670941685, -286.7038534672208812, -225.1030815780964360 ) ) ;
#2924 = CARTESIAN_POINT ( 'NONE',  ( -106.2025032871872980, -279.9544073437096472, -297.4934566202261408 ) ) ;
#2925 = CARTESIAN_POINT ( 'NONE',  ( -106.1563940164742803, -286.4068372814649592, -237.1475033595592095 ) ) ;
#2926 = CARTESIAN_POINT ( 'NONE',  ( -15.52709920383375142, -284.7699772989835765, -342.1185136498224324 ) ) ;
#2927 = CARTESIAN_POINT ( 'NONE',  ( -31.44814834119044633, -277.1464904308163000, -347.1878648014589999 ) ) ;
#2928 = CARTESIAN_POINT ( 'NONE',  ( -89.21368040031019575, -277.5917971751738946, -327.2671604308478095 ) ) ;
#2929 = CARTESIAN_POINT ( 'NONE',  ( -96.44706004355793993, -299.0968105714748049, -225.0869355814819528 ) ) ;
#2930 = LINE ( 'NONE', #60708, #86796 ) ;
#2931 = EDGE_CURVE ( 'NONE', #4825, #86359, #52442, .T. ) ;
#2932 = CARTESIAN_POINT ( 'NONE',  ( -106.6379572354042296, -280.6233781216988064, -303.7686719486574702 ) ) ;
#2933 = CARTESIAN_POINT ( 'NONE',  ( 29.45481597813228802, -297.0194551764546418, -194.6172037023857513 ) ) ;
#2934 = DIRECTION ( 'NONE',  ( 0.7957555401921969640, 0.6056179655966498210, 0.000000000000000000 ) ) ;
#2935 = CARTESIAN_POINT ( 'NONE',  ( -37.81644747580428145, -276.5658722141536714, -343.4335775399458157 ) ) ;
#2936 = CARTESIAN_POINT ( 'NONE',  ( 24.15190359836281786, -276.1466954785532266, -224.6823984261923499 ) ) ;
#2937 = CARTESIAN_POINT ( 'NONE',  ( 35.38230468208542590, -280.9232887556263449, -295.1034455707778079 ) ) ;
#2938 = CARTESIAN_POINT ( 'NONE',  ( 14.81312134196681640, -290.0649169452819365, -322.8763406324623020 ) ) ;
#2939 = CARTESIAN_POINT ( 'NONE',  ( -95.96620879823493055, -297.4090596858279127, -319.2268452488467005 ) ) ;
#2940 = CARTESIAN_POINT ( 'NONE',  ( -113.5466448117420839, -297.6591900471490817, -278.1595231856105102 ) ) ;
#2941 = CARTESIAN_POINT ( 'NONE',  ( -11.65423065400196023, -294.3874482102523871, -200.0194642710369521 ) ) ;
#2942 = CARTESIAN_POINT ( 'NONE',  ( 30.64877523258950376, -279.1391369767742390, -238.9746644816205219 ) ) ;
#2943 = CARTESIAN_POINT ( 'NONE',  ( 29.05495563625945366, -283.0228044141385908, -236.5898266888796684 ) ) ;
#2944 = CARTESIAN_POINT ( 'NONE',  ( -44.68731909621574516, -296.0384519634630465, -196.2330519449467374 ) ) ;
#2945 = CARTESIAN_POINT ( 'NONE',  ( -111.5849307654610385, -286.3691074003725134, -253.2035213163013054 ) ) ;
#2946 = CARTESIAN_POINT ( 'NONE',  ( -2.025449827848527118, -285.4514203212203256, -206.0625150002080659 ) ) ;
#2947 = CARTESIAN_POINT ( 'NONE',  ( 21.89749367432979454, -280.2407708675747813, -221.3302021775997162 ) ) ;
#2948 = CARTESIAN_POINT ( 'NONE',  ( -93.70700619081699756, -240.9337940567206431, -341.5190362321769157 ) ) ;
#2949 = ORIENTED_EDGE ( 'NONE', *, *, #86598, .T. ) ;
#2950 = CARTESIAN_POINT ( 'NONE',  ( -69.12886551661786427, -288.0368317553940187, -339.8605567356493111 ) ) ;
#2951 = CARTESIAN_POINT ( 'NONE',  ( 24.97097506146832657, -286.6945253799232773, -232.2925220345383082 ) ) ;
#2952 = ORIENTED_EDGE ( 'NONE', *, *, #80976, .T. ) ;
#2953 = CARTESIAN_POINT ( 'NONE',  ( -113.2912712511572408, -285.4935443032257467, -281.3731746439570429 ) ) ;
#2954 = CARTESIAN_POINT ( 'NONE',  ( 33.26372301889318805, -276.1313242869352962, -288.9880261822770535 ) ) ;
#2955 = EDGE_CURVE ( 'NONE', #15079, #77887, #79661, .T. ) ;
#2956 = CARTESIAN_POINT ( 'NONE',  ( -19.44550728358895242, -291.1973302276585400, -195.7329335394500447 ) ) ;
#2957 = CARTESIAN_POINT ( 'NONE',  ( 28.22244103946771432, -282.7304047362337656, -310.6448302517616753 ) ) ;
#2958 = CARTESIAN_POINT ( 'NONE',  ( -101.3205667520087445, -280.6244515284915906, -228.6792664564569861 ) ) ;
#2959 = CARTESIAN_POINT ( 'NONE',  ( 21.95170591714795805, -281.2253059536230353, -221.2689975232774486 ) ) ;
#2960 = CARTESIAN_POINT ( 'NONE',  ( 30.91033621190086578, -290.8380690714489560, -254.8156830097664738 ) ) ;
#2961 = CARTESIAN_POINT ( 'NONE',  ( 6.325340719953564061, -58.69197721219502029, -354.8253570307668952 ) ) ;
#2962 = ORIENTED_EDGE ( 'NONE', *, *, #45806, .T. ) ;
#2963 = CARTESIAN_POINT ( 'NONE',  ( 16.94494931043544028, -278.2765412746037441, -321.8682836903628299 ) ) ;
#2964 = CARTESIAN_POINT ( 'NONE',  ( 201.1675596189675446, 293.6556537245446634, -83.10562796347613812 ) ) ;
#2965 = VECTOR ( 'NONE', #11518, 1000.000000000000000 ) ;
#2966 = CARTESIAN_POINT ( 'NONE',  ( 25.50188153274858394, -280.1183605235837035, -310.7367447317829487 ) ) ;
#2967 = CARTESIAN_POINT ( 'NONE',  ( -101.2997446411217908, -296.3839126046775050, -234.9596884921501214 ) ) ;
#2968 = CARTESIAN_POINT ( 'NONE',  ( 38.26592855160097884, -292.8814704008326544, -256.1128412858878960 ) ) ;
#2969 = DIRECTION ( 'NONE',  ( 0.000000000000000000, 0.000000000000000000, 1.000000000000000000 ) ) ;
#2971 = CARTESIAN_POINT ( 'NONE',  ( -73.95941970419592337, -287.9470323679709054, -334.4505129913720225 ) ) ;
#2970 = CARTESIAN_POINT ( 'NONE',  ( -67.92481853885293219, -296.2333603907616748, -200.2813436115579009 ) ) ;
#2972 = CARTESIAN_POINT ( 'NONE',  ( -25.99563728367191828, -296.7665640718874442, -343.7241354788083640 ) ) ;
#2973 = CARTESIAN_POINT ( 'NONE',  ( -41.36657001774556619, -287.3156292685786184, -196.9656769640162395 ) ) ;
#2974 = ORIENTED_EDGE ( 'NONE', *, *, #32590, .F. ) ;
#2975 = CARTESIAN_POINT ( 'NONE',  ( -3.436110940620233478, -293.4300646426044636, -201.4755056033205278 ) ) ;
#2976 = CARTESIAN_POINT ( 'NONE',  ( -106.2296571493007349, -284.7190558751621552, -294.8517802936671615 ) ) ;
#2977 = CARTESIAN_POINT ( 'NONE',  ( -97.02726496196710571, -295.9939609678064016, -222.3440161226215253 ) ) ;
#2978 = CARTESIAN_POINT ( 'NONE',  ( -77.09449430967256944, -292.3369076640341859, -204.5435781759580607 ) ) ;
#2979 = CARTESIAN_POINT ( 'NONE',  ( -5.917812314285831654, -292.9465971988785213, -200.1181710203466366 ) ) ;
#2980 = CARTESIAN_POINT ( 'NONE',  ( -34.57587542716795781, -289.1832534903532519, -343.3582849914051849 ) ) ;
#2981 = VERTEX_POINT ( 'NONE', #15532 ) ;
#2982 = CARTESIAN_POINT ( 'NONE',  ( 157.0521749816618069, 17.25638377771152676, 7.577257116167345430 ) ) ;
#2983 = CARTESIAN_POINT ( 'NONE',  ( -70.21488714162688893, -299.4839891301380135, -202.0994225688680785 ) ) ;
#2984 = CARTESIAN_POINT ( 'NONE',  ( -57.99970379579195878, -272.5861082653977405, -196.5411150402163685 ) ) ;
#2985 = CARTESIAN_POINT ( 'NONE',  ( 5.720802865667158343, -281.5109840627208655, -329.5981780326182502 ) ) ;
#2986 = ORIENTED_EDGE ( 'NONE', *, *, #75967, .T. ) ;
#2987 = CARTESIAN_POINT ( 'NONE',  ( 12.65986701365186384, -275.8839807285244206, -328.8364990110983399 ) ) ;
#2988 = CARTESIAN_POINT ( 'NONE',  ( -106.1548794823400925, -271.3061729983235750, -243.5521685186124330 ) ) ;
#2989 = CARTESIAN_POINT ( 'NONE',  ( -67.83496793265835834, -281.5080505367585033, -202.6640011536138957 ) ) ;
#2990 = CARTESIAN_POINT ( 'NONE',  ( 33.69153331797667761, -273.9730815556033008, -291.9723621250579413 ) ) ;
#2991 = CARTESIAN_POINT ( 'NONE',  ( -41.90829471547915830, -299.1984041650800350, -197.1062429286031090 ) ) ;
#2992 = CARTESIAN_POINT ( 'NONE',  ( -98.04492213693521308, -274.0620976265568061, -229.3007920494205791 ) ) ;
#2993 = CARTESIAN_POINT ( 'NONE',  ( -112.8122911223118194, -298.2863968740475684, -259.7484565993211731 ) ) ;
#2994 = CARTESIAN_POINT ( 'NONE',  ( 1.590278049532844351, -272.5900234431163653, -205.8420674816332507 ) ) ;
#2995 = CARTESIAN_POINT ( 'NONE',  ( 20.60907936929845974, -294.8300248985997314, -314.9416857134140741 ) ) ;
#2996 = CARTESIAN_POINT ( 'NONE',  ( -17.25446246306490750, -290.8911275413054227, -199.5134797963687276 ) ) ;
#2997 = CARTESIAN_POINT ( 'NONE',  ( -83.63170945779077670, -296.0521521680024080, -417.1172536214571096 ) ) ;
#2998 = CARTESIAN_POINT ( 'NONE',  ( 9.467932666813636544, -275.1689144392015578, -209.3006137211017688 ) ) ;
#2999 = CARTESIAN_POINT ( 'NONE',  ( -62.03169170696425994, -273.8886687302750147, -201.6631971964509376 ) ) ;
#3000 = CARTESIAN_POINT ( 'NONE',  ( -38.74043224664081464, -281.7541842362255124, -346.8551819548016510 ) ) ;
#3001 = CARTESIAN_POINT ( 'NONE',  ( -22.43559455235949684, -296.8618801444668520, -344.0349697897236183 ) ) ;
#3002 = FACE_OUTER_BOUND ( 'NONE', #70187, .T. ) ;
#3003 = CARTESIAN_POINT ( 'NONE',  ( -109.7706457989530122, -283.8852471624824148, -260.0339907911579189 ) ) ;
#3004 = CARTESIAN_POINT ( 'NONE',  ( -106.5493604861856340, -282.1680181430447192, -299.8257300144005058 ) ) ;
#3005 = ADVANCED_FACE ( 'NONE', ( #44406 ), #23254, .F. ) ;
#3006 = CARTESIAN_POINT ( 'NONE',  ( 36.23238107834401944, -274.1073329748978153, -268.8679702717868736 ) ) ;
#3007 = CARTESIAN_POINT ( 'NONE',  ( 10.88161637998043396, -282.7188842188192552, -212.8526851851519268 ) ) ;
#3008 = DIRECTION ( 'NONE',  ( 0.000000000000000000, 0.000000000000000000, -1.000000000000000000 ) ) ;
#3009 = DIRECTION ( 'NONE',  ( -1.000000000000000000, 0.000000000000000000, 0.000000000000000000 ) ) ;
#3010 = CARTESIAN_POINT ( 'NONE',  ( -27.08382758656488676, -272.5802125551643371, -194.8018419186716415 ) ) ;
#3011 = CARTESIAN_POINT ( 'NONE',  ( -64.41049912907440955, -279.4046283878169561, -340.5395785599721421 ) ) ;
#3012 = DIRECTION ( 'NONE',  ( -1.000000000000000000, 0.000000000000000000, 0.000000000000000000 ) ) ;
#3013 = CARTESIAN_POINT ( 'NONE',  ( -106.8919198422468355, -286.0877017183601652, -300.0258869104520727 ) ) ;
#3014 = DIRECTION ( 'NONE',  ( 0.000000000000000000, 0.000000000000000000, 1.000000000000000000 ) ) ;
#3015 = CARTESIAN_POINT ( 'NONE',  ( -112.3869558678607348, -288.5397485678157068, -271.3142857673570916 ) ) ;
#3016 = CARTESIAN_POINT ( 'NONE',  ( 208.0212563688061209, 27.56882951438707607, 12.00000000000000000 ) ) ;
#3017 = CARTESIAN_POINT ( 'NONE',  ( -109.6645173009884076, -295.5112285779792956, -257.8494985183143058 ) ) ;
#3018 = CARTESIAN_POINT ( 'NONE',  ( -69.31102360988489863, -287.6169388157089770, -337.3598331948587088 ) ) ;
#3019 = CARTESIAN_POINT ( 'NONE',  ( 22.29632774050155319, -23.10002859818378340, -338.8215327972035311 ) ) ;
#3020 = CARTESIAN_POINT ( 'NONE',  ( -98.04167817466826307, -293.9517282718423985, -314.4343059470606363 ) ) ;
#3021 = CARTESIAN_POINT ( 'NONE',  ( 24.15608193541861581, -285.4265580190075298, -225.1866721606569115 ) ) ;
#3022 = CARTESIAN_POINT ( 'NONE',  ( 30.05325989315680957, -283.5543187774048874, -300.5592469201921517 ) ) ;
#3023 = CARTESIAN_POINT ( 'NONE',  ( -78.62819165778435604, -281.8398905386174533, -334.1529640879004432 ) ) ;
#3024 = CARTESIAN_POINT ( 'NONE',  ( -63.82089453060896034, -289.4071338496478916, -338.4436225798462488 ) ) ;
#3025 = CARTESIAN_POINT ( 'NONE',  ( 18.95676949748348150, -283.6453954953609582, -317.7711614054133520 ) ) ;
#3026 = CARTESIAN_POINT ( 'NONE',  ( -36.18073762146470074, -283.8400618162410183, -343.5133831118960188 ) ) ;
#3027 = CARTESIAN_POINT ( 'NONE',  ( 37.71393172772059899, -289.4391299682946510, -263.0903383623077616 ) ) ;
#3028 = AXIS2_PLACEMENT_3D ( 'NONE', #31242, #65388, #22716 ) ;
#3029 = CARTESIAN_POINT ( 'NONE',  ( -26.21185907515926772, -298.3545741468140591, -193.3608124155709902 ) ) ;
#3030 = ORIENTED_EDGE ( 'NONE', *, *, #89041, .T. ) ;
#3031 = CARTESIAN_POINT ( 'NONE',  ( -96.02768843728122761, -273.2243337611700440, -220.4914962255848536 ) ) ;
#3033 = CARTESIAN_POINT ( 'NONE',  ( -44.48209383374271653, -293.9414057577958488, -196.0066536928164851 ) ) ;
#3032 = VECTOR ( 'NONE', #46391, 1000.000000000000000 ) ;
#3034 = DIRECTION ( 'NONE',  ( 0.000000000000000000, 0.000000000000000000, -1.000000000000000000 ) ) ;
#3035 = CARTESIAN_POINT ( 'NONE',  ( -54.49178911615187815, -282.3376638359844719, -195.3683826091709363 ) ) ;
#3036 = CARTESIAN_POINT ( 'NONE',  ( 37.55162405153379268, -273.6340407221134683, -276.7656802560686629 ) ) ;
#3037 = DIRECTION ( 'NONE',  ( 0.000000000000000000, 0.000000000000000000, -1.000000000000000000 ) ) ;
#3038 = CARTESIAN_POINT ( 'NONE',  ( -35.47558221234827158, -296.4750249970931009, -194.1616107217360252 ) ) ;
#3039 = CARTESIAN_POINT ( 'NONE',  ( -110.2057400926187825, -291.9983672487444437, -282.1567865367271111 ) ) ;
#3040 = CARTESIAN_POINT ( 'NONE',  ( -43.48242765931818354, -273.3212619719324721, -197.4667772659005891 ) ) ;
#3041 = CARTESIAN_POINT ( 'NONE',  ( -106.3668036116438458, -292.4150927758277589, -244.4045357148850997 ) ) ;
#3042 = CARTESIAN_POINT ( 'NONE',  ( -17.37993872388247141, -293.2572709366335744, -199.8460532097747091 ) ) ;
#3043 = CARTESIAN_POINT ( 'NONE',  ( -76.64652642244364245, -285.3457353450075402, -333.1361879564246919 ) ) ;
#3044 = CARTESIAN_POINT ( 'NONE',  ( -105.4869049485316168, -292.4271843175775416, -235.6779807014726771 ) ) ;
#3045 = CARTESIAN_POINT ( 'NONE',  ( -58.81640960301491106, -293.0951848331761198, -196.9299588974726589 ) ) ;
#3046 = CARTESIAN_POINT ( 'NONE',  ( -39.69116431654797594, -294.9157623180346377, -343.3357305434871591 ) ) ;
#3047 = CARTESIAN_POINT ( 'NONE',  ( 15.51034928217692510, -290.3048975154570144, -323.5744764621534273 ) ) ;
#3048 = CARTESIAN_POINT ( 'NONE',  ( 27.85022165064060218, -281.1811771619723572, -229.2854337535828222 ) ) ;
#3049 = CARTESIAN_POINT ( 'NONE',  ( -51.50623766145860571, -295.9523515955251014, -196.0873153619806430 ) ) ;
#3050 = CARTESIAN_POINT ( 'NONE',  ( -110.2253665077959823, -284.0725096859965220, -295.2000225387272394 ) ) ;
#3051 = CARTESIAN_POINT ( 'NONE',  ( -3.090780735409602187, -278.5771951035954999, -336.6839747249878769 ) ) ;
#3052 = CARTESIAN_POINT ( 'NONE',  ( -107.7772799113469091, -283.0749666145505330, -291.0448133529571351 ) ) ;
#3053 = CARTESIAN_POINT ( 'NONE',  ( -13.31955261483823527, -284.3639863407584016, -199.3122821290266415 ) ) ;
#3054 = CARTESIAN_POINT ( 'NONE',  ( -51.11174979524055573, -275.3659373070663037, -344.8640790656508557 ) ) ;
#3055 = CARTESIAN_POINT ( 'NONE',  ( 113.5000000000000568, -218.8335761803644743, -490.8867980474134356 ) ) ;
#3056 = CARTESIAN_POINT ( 'NONE',  ( -2.404747239855777430, -282.0843592358984324, -334.5423710278622025 ) ) ;
#3057 = CARTESIAN_POINT ( 'NONE',  ( -53.69077580166315045, -281.0520664835295293, -195.4688937955734502 ) ) ;
#3058 = CARTESIAN_POINT ( 'NONE',  ( 21.91620773548717693, -285.9532751934067392, -221.5623416704565045 ) ) ;
#3059 = CARTESIAN_POINT ( 'NONE',  ( 34.10064247204049082, -295.5648138790134567, -289.7475538954539047 ) ) ;
#3060 = CARTESIAN_POINT ( 'NONE',  ( 22.89826290227155781, -277.7821046158716172, -317.0469120987233396 ) ) ;
#3061 = CARTESIAN_POINT ( 'NONE',  ( 38.00350234478532485, -276.6992061323920780, -257.0048325610704865 ) ) ;
#3062 = CARTESIAN_POINT ( 'NONE',  ( -80.82108114090546280, -277.4944608506777399, -329.0002127165847128 ) ) ;
#3063 = CARTESIAN_POINT ( 'NONE',  ( -66.30523341228550294, -299.6722401642571185, -201.3600877877883022 ) ) ;
#3064 = CARTESIAN_POINT ( 'NONE',  ( -1.281123231060983469, -284.5310798975464195, -204.7311511825882349 ) ) ;
#3065 = CARTESIAN_POINT ( 'NONE',  ( -108.7315755454474697, -292.4944906565732481, -243.5662014241347038 ) ) ;
#3066 = CARTESIAN_POINT ( 'NONE',  ( 0.07860816415507965171, -291.4833429118256731, -207.3218714691700484 ) ) ;
#3067 = VERTEX_POINT ( 'NONE', #8877 ) ;
#3068 = CARTESIAN_POINT ( 'NONE',  ( -14.83585392158876459, -292.0186628350635942, -200.8947637292160948 ) ) ;
#3069 = VERTEX_POINT ( 'NONE', #87028 ) ;
#3070 = CARTESIAN_POINT ( 'NONE',  ( 14.40531861230846467, -289.4246479270315149, -327.0346702897856517 ) ) ;
#3071 = CARTESIAN_POINT ( 'NONE',  ( -57.14878627495813390, -280.4411715149433917, -199.9937107100818139 ) ) ;
#3072 = ADVANCED_FACE ( 'NONE', ( #81317 ), #16463, .T. ) ;
#3073 = CARTESIAN_POINT ( 'NONE',  ( -112.8324078728765301, -295.6421855100037419, -256.8464757572042458 ) ) ;
#3074 = CARTESIAN_POINT ( 'NONE',  ( 16.62034589414837171, -288.9607096590137303, -325.2203012307290919 ) ) ;
#3075 = CARTESIAN_POINT ( 'NONE',  ( 28.67822697776172447, -287.3678649460407541, -230.6715384530783695 ) ) ;
#3076 = CARTESIAN_POINT ( 'NONE',  ( -91.67794081615380719, -284.1872729663721771, -319.1616948540911949 ) ) ;
#3077 = CARTESIAN_POINT ( 'NONE',  ( 201.8898544361462939, 293.7279171300682492, -83.20153124629544550 ) ) ;
#3078 = CARTESIAN_POINT ( 'NONE',  ( -91.05905222517534980, -229.2228000228819553, -346.3972628765899913 ) ) ;
#3079 = CARTESIAN_POINT ( 'NONE',  ( 172.7241459038852724, 240.9461585357967977, -177.0720788202972642 ) ) ;
#3080 = CARTESIAN_POINT ( 'NONE',  ( -40.52299827980939284, -276.2903069137316834, -343.4658875544013199 ) ) ;
#3081 = CARTESIAN_POINT ( 'NONE',  ( -69.39895019544928800, -276.4044892244371567, -336.3034515216097589 ) ) ;
#3082 = CARTESIAN_POINT ( 'NONE',  ( -68.83153142094452903, -273.3161080052328202, -200.1033302448623488 ) ) ;
#3083 = CARTESIAN_POINT ( 'NONE',  ( 168.8266546690683469, 229.6582186635458811, -190.4167746751373045 ) ) ;
#3084 = CARTESIAN_POINT ( 'NONE',  ( -12.04514565589438391, -275.4146594927864271, -342.6204389095458964 ) ) ;
#3085 = ORIENTED_EDGE ( 'NONE', *, *, #11508, .F. ) ;
#3086 = CARTESIAN_POINT ( 'NONE',  ( -45.36298306592939866, -289.6488715600345927, -342.9810013592488076 ) ) ;
#3087 = CARTESIAN_POINT ( 'NONE',  ( -97.22694137413476767, -298.0015441995196852, -222.2163705817446555 ) ) ;
#3088 = CARTESIAN_POINT ( 'NONE',  ( -110.7392032743995856, -296.7538416112298023, -293.4775556820247857 ) ) ;
#3089 = CARTESIAN_POINT ( 'NONE',  ( -77.94797901830229137, -295.7810334968511938, -331.0862488517759630 ) ) ;
#3090 = EDGE_LOOP ( 'NONE', ( #20220, #50138, #1554, #40636 ) ) ;
#3091 = CARTESIAN_POINT ( 'NONE',  ( -98.47012575264064083, -279.8715112114314252, -314.7974066838259546 ) ) ;
#3092 = AXIS2_PLACEMENT_3D ( 'NONE', #65272, #1767, #36359 ) ;
#3093 = CARTESIAN_POINT ( 'NONE',  ( 2.057236658432576526, -282.0471212020546545, -336.4462954681184215 ) ) ;
#3094 = CARTESIAN_POINT ( 'NONE',  ( -95.86679617888430016, -280.2495778382210005, -226.1923521755928448 ) ) ;
#3095 = CARTESIAN_POINT ( 'NONE',  ( 18.17832909697120769, -278.0292572741548724, -322.2407899997566005 ) ) ;
#3096 = AXIS2_PLACEMENT_3D ( 'NONE', #75932, #24340, #53215 ) ;
#3097 = CARTESIAN_POINT ( 'NONE',  ( -75.50078601134499934, -296.1074769172285528, -207.3794021907888805 ) ) ;
#3098 = LINE ( 'NONE', #67517, #66901 ) ;
#3099 = CARTESIAN_POINT ( 'NONE',  ( -92.20984144269753813, -279.4062738393386098, -222.1914310669604049 ) ) ;
#3100 = CARTESIAN_POINT ( 'NONE',  ( -58.08786774099759498, -274.5936933841057339, -196.3209753106200992 ) ) ;
#3101 = CARTESIAN_POINT ( 'NONE',  ( 29.92109096748625419, -286.7128903450975486, -306.9275318989845118 ) ) ;
#3102 = CARTESIAN_POINT ( 'NONE',  ( -97.96586353315110784, -275.1549477435995072, -226.1194276546539186 ) ) ;
#3103 = CARTESIAN_POINT ( 'NONE',  ( 33.63017435991903170, -274.4904678438071528, -298.8162146314662095 ) ) ;
#3104 = CARTESIAN_POINT ( 'NONE',  ( 165.2424497756046549, 275.5000000000000568, 22.91843887563435800 ) ) ;
#3105 = CARTESIAN_POINT ( 'NONE',  ( -80.51101045638458231, -288.8511520479362389, -329.4920280820580842 ) ) ;
#3106 = CARTESIAN_POINT ( 'NONE',  ( -112.4273608584512658, -283.6929006306159522, -286.9579953948043567 ) ) ;
#3107 = CARTESIAN_POINT ( 'NONE',  ( -5.618676244901598338, -280.8690342811481173, -337.2452585550860249 ) ) ;
#3109 = CARTESIAN_POINT ( 'NONE',  ( -57.76646952932928514, -283.8663224293867415, -198.7243532075731309 ) ) ;
#3108 = CARTESIAN_POINT ( 'NONE',  ( 36.15349400680588587, -280.1755402659749734, -274.0801709193741544 ) ) ;
#3110 = CARTESIAN_POINT ( 'NONE',  ( -70.07719201519769570, -291.4834696180043920, -337.8539023633189800 ) ) ;
#3111 = CARTESIAN_POINT ( 'NONE',  ( -99.81372407934746604, -280.2867524017653409, -231.7365177741657192 ) ) ;
#3112 = CARTESIAN_POINT ( 'NONE',  ( -103.8239762884536503, -271.0130733266666994, -235.5342847911063302 ) ) ;
#3113 = CARTESIAN_POINT ( 'NONE',  ( -27.49587067370445581, -281.3290688088525258, -345.9751576346699267 ) ) ;
#3114 = CARTESIAN_POINT ( 'NONE',  ( 36.09817803515041135, -295.3561070683542766, -255.0803593480729319 ) ) ;
#3115 = CARTESIAN_POINT ( 'NONE',  ( -31.13389149590402738, -278.3692832688519729, -194.5764519779699526 ) ) ;
#3116 = CARTESIAN_POINT ( 'NONE',  ( -108.5837353612852354, -278.9869936502050223, -286.8014701598497140 ) ) ;
#3117 = CARTESIAN_POINT ( 'NONE',  ( -24.81345774986261787, -284.8929889093944894, -344.5292069607254462 ) ) ;
#3118 = EDGE_CURVE ( 'NONE', #10505, #31408, #2105, .T. ) ;
#3119 = EDGE_CURVE ( 'NONE', #68047, #25647, #2730, .T. ) ;
#3120 = PLANE ( 'NONE',  #65582 ) ;
#3121 = CARTESIAN_POINT ( 'NONE',  ( -63.90589228720160264, -293.6287176404612751, -199.5694485526131814 ) ) ;
#3122 = CARTESIAN_POINT ( 'NONE',  ( 36.67689324420568653, -273.7112893889893144, -282.7676018470114627 ) ) ;
#3123 = CARTESIAN_POINT ( 'NONE',  ( 39.47883557998053305, -286.7284846699095624, -268.6985556441270546 ) ) ;
#3124 = CARTESIAN_POINT ( 'NONE',  ( -55.18628355259232166, -290.2186476542224227, -198.7509842342544744 ) ) ;
#3125 = CARTESIAN_POINT ( 'NONE',  ( -48.18343439339133027, -272.4879030626730696, -437.5575391234876861 ) ) ;
#3126 = CARTESIAN_POINT ( 'NONE',  ( 32.56211506881474804, -274.5359562479713986, -293.0481208463745020 ) ) ;
#3127 = CARTESIAN_POINT ( 'NONE',  ( -61.43610201560318274, -293.5078943124126454, -340.6318805672689791 ) ) ;
#3128 = DIRECTION ( 'NONE',  ( 0.9951408606192333473, 0.000000000000000000, -0.09846150276129089773 ) ) ;
#3129 = PLANE ( 'NONE',  #2019 ) ;
#3130 = CARTESIAN_POINT ( 'NONE',  ( 38.80879532418298794, -292.1032865527982381, -276.0073016608375838 ) ) ;
#3131 = CARTESIAN_POINT ( 'NONE',  ( -35.93846714110579654, -287.6701726972185611, -196.5744568950748317 ) ) ;
#3132 = CARTESIAN_POINT ( 'NONE',  ( -12.57546657330419393, -286.9744693794624482, -342.2536172055258135 ) ) ;
#3133 = CARTESIAN_POINT ( 'NONE',  ( 13.53391193484293353, -288.2064127064416539, -217.1208506087276646 ) ) ;
#3134 = CARTESIAN_POINT ( 'NONE',  ( 189.4188515237862589, 293.9636489450775798, -9.103929867429222611 ) ) ;
#3135 = CARTESIAN_POINT ( 'NONE',  ( 34.44458160300596461, -288.5416754317006962, -284.5444050319245548 ) ) ;
#3136 = CARTESIAN_POINT ( 'NONE',  ( 31.80490320440512875, -295.1420089349788327, -240.4085880801197845 ) ) ;
#3137 = DIRECTION ( 'NONE',  ( 0.000000000000000000, 1.000000000000000000, 0.000000000000000000 ) ) ;
#3138 = CARTESIAN_POINT ( 'NONE',  ( 39.18007486906842018, -288.7002209067438230, -265.8265251596110943 ) ) ;
#3139 = CARTESIAN_POINT ( 'NONE',  ( -53.84108145133048851, -275.3420229753857598, -344.1513293236438926 ) ) ;
#3140 = CARTESIAN_POINT ( 'NONE',  ( -102.0769076686427894, -278.3376488508054081, -312.1128748316036194 ) ) ;
#3141 = CARTESIAN_POINT ( 'NONE',  ( 20.11573350605875277, -280.5239699987596396, -219.1125193097255703 ) ) ;
#3142 = CARTESIAN_POINT ( 'NONE',  ( -58.39224187424481016, -299.7585883280645476, -198.7460253527467842 ) ) ;
#3143 = CARTESIAN_POINT ( 'NONE',  ( -43.32092956878232570, -270.7650335506043007, -505.4258654641533326 ) ) ;
#3144 = CARTESIAN_POINT ( 'NONE',  ( -44.18210449760081104, -283.9654691773182549, -195.6737059470788722 ) ) ;
#3145 = DIRECTION ( 'NONE',  ( 0.000000000000000000, 1.000000000000000000, 0.000000000000000000 ) ) ;
#3146 = CARTESIAN_POINT ( 'NONE',  ( -101.6647520232515660, -276.1908534411145411, -307.5239685529722351 ) ) ;
#3147 = CARTESIAN_POINT ( 'NONE',  ( 37.64219235886115200, -279.5109957541901622, -267.1685931404740018 ) ) ;
#3148 = CARTESIAN_POINT ( 'NONE',  ( 194.7510731661265595, -164.3527196417747405, 22.50000000000000000 ) ) ;
#3149 = CARTESIAN_POINT ( 'NONE',  ( -38.55353751901358805, -275.5469734511579531, -346.6581638315258260 ) ) ;
#3150 = CARTESIAN_POINT ( 'NONE',  ( -106.6325460656534574, -297.7394181985087016, -295.6006231813223053 ) ) ;
#3151 = CARTESIAN_POINT ( 'NONE',  ( -4.309480011362734508, -281.5472517469743821, -339.5880098019582078 ) ) ;
#3152 = CARTESIAN_POINT ( 'NONE',  ( -103.9375315631847059, -297.9044591093028771, -239.7692950969522485 ) ) ;
#3153 = CARTESIAN_POINT ( 'NONE',  ( -87.15395982469463831, -298.6905374437307614, -212.2220226413342061 ) ) ;
#3154 = CARTESIAN_POINT ( 'NONE',  ( 19.87471900312880990, -274.5784544573400581, -224.9718588033083506 ) ) ;
#3155 = CARTESIAN_POINT ( 'NONE',  ( 36.81942298719200579, -295.7002883529291353, -281.8857563062040867 ) ) ;
#3156 = CARTESIAN_POINT ( 'NONE',  ( 37.71915334566357103, -287.5034156985354343, -253.1308786954831191 ) ) ;
#3157 = CARTESIAN_POINT ( 'NONE',  ( -98.25228059568989636, -277.2374212787451597, -225.6267039745527256 ) ) ;
#3158 = CARTESIAN_POINT ( 'NONE',  ( -112.5657980065144983, -290.1798448089752469, -286.8029884026397553 ) ) ;
#3159 = CARTESIAN_POINT ( 'NONE',  ( 17.96171838373200558, -285.9286965936914271, -222.3513236743515620 ) ) ;
#3160 = CARTESIAN_POINT ( 'NONE',  ( -6.680634681508814232, -290.4544925771463681, -201.9008708072903744 ) ) ;
#3161 = ORIENTED_EDGE ( 'NONE', *, *, #12809, .F. ) ;
#3162 = CARTESIAN_POINT ( 'NONE',  ( 23.55732936118107901, -287.6197140082176134, -310.7485135007678991 ) ) ;
#3163 = DIRECTION ( 'NONE',  ( 0.5335274993777934238, -0.8457827187922903889, 0.000000000000000000 ) ) ;
#3164 = CARTESIAN_POINT ( 'NONE',  ( -99.16190811959243945, -286.1008385486072143, -224.7644959229374990 ) ) ;
#3165 = CARTESIAN_POINT ( 'NONE',  ( -2.152982846972653075, -291.5651546628753863, -202.1219432100804170 ) ) ;
#3166 = CARTESIAN_POINT ( 'NONE',  ( 27.16316385631357022, -282.6143944792402749, -229.6967351381213405 ) ) ;
#3167 = CARTESIAN_POINT ( 'NONE',  ( -17.13843939398215710, -281.6228536193876266, -196.5700173861686721 ) ) ;
#3168 = AXIS2_PLACEMENT_3D ( 'NONE', #78776, #38339, #60149 ) ;
#3169 = CARTESIAN_POINT ( 'NONE',  ( -67.78630364169399058, -283.2965420665266834, -336.7096380974146541 ) ) ;
#3170 = CARTESIAN_POINT ( 'NONE',  ( -113.6526282743976708, -296.4187247969506416, -281.0298623535917955 ) ) ;
#3171 = CARTESIAN_POINT ( 'NONE',  ( -85.64682327319778210, -274.6826751743233785, -214.9050234370071450 ) ) ;
#3172 = CARTESIAN_POINT ( 'NONE',  ( 34.90641323735309243, -291.3300079090541317, -251.5979380625179544 ) ) ;
#3173 = CARTESIAN_POINT ( 'NONE',  ( -21.83525760534138627, -273.0502545481738821, -198.6207475910898097 ) ) ;
#3174 = ORIENTED_EDGE ( 'NONE', *, *, #53671, .T. ) ;
#3175 = CARTESIAN_POINT ( 'NONE',  ( 222.8344101925596306, 36.73669859915801794, 7.000000000000000000 ) ) ;
#3176 = CARTESIAN_POINT ( 'NONE',  ( -74.49469757111489798, -285.4701770953417395, -334.9254219910689017 ) ) ;
#3177 = CARTESIAN_POINT ( 'NONE',  ( -22.14529752142060204, -295.9415392033025114, -345.5313371967322951 ) ) ;
#3178 = CARTESIAN_POINT ( 'NONE',  ( -97.61169086423342378, -284.6274329276824346, -311.8186506267267077 ) ) ;
#3179 = CARTESIAN_POINT ( 'NONE',  ( -7.985738926497114143, -275.7356267870846978, -341.3052370359391148 ) ) ;
#3180 = CARTESIAN_POINT ( 'NONE',  ( 39.55375964649560672, -294.1668854424063966, -267.4321988208715197 ) ) ;
#3181 = CARTESIAN_POINT ( 'NONE',  ( 24.54999461602020006, -285.1037932265534209, -226.6383561968136462 ) ) ;
#3182 = CARTESIAN_POINT ( 'NONE',  ( 24.79487604314860860, -293.2819738738166393, -224.9211554682974565 ) ) ;
#3183 = CARTESIAN_POINT ( 'NONE',  ( -98.85729388595689215, -290.3413811284460735, -309.7047224357694972 ) ) ;
#3184 = CARTESIAN_POINT ( 'NONE',  ( 175.2296996224750103, 214.5000000000000568, 0.000000000000000000 ) ) ;
#3185 = DIRECTION ( 'NONE',  ( 0.000000000000000000, 0.000000000000000000, -1.000000000000000000 ) ) ;
#3186 = CARTESIAN_POINT ( 'NONE',  ( 84.93309205534008299, 81.36957093815985331, -298.8374046425330448 ) ) ;
#3187 = CARTESIAN_POINT ( 'NONE',  ( -103.8035332550911392, -285.5801295624835916, -307.9585234203994446 ) ) ;
#3188 = CARTESIAN_POINT ( 'NONE',  ( 25.22466315766302358, -278.4094976428775681, -220.5068182859052968 ) ) ;
#3189 = ORIENTED_EDGE ( 'NONE', *, *, #89909, .F. ) ;
#3190 = CARTESIAN_POINT ( 'NONE',  ( -38.90540172793681251, -281.9925159454898562, -343.6660957841280037 ) ) ;
#3191 = CARTESIAN_POINT ( 'NONE',  ( -77.80739894272457491, -277.2462581844129090, -335.9079588489759658 ) ) ;
#3192 = CARTESIAN_POINT ( 'NONE',  ( -4.783303107571053481, -282.4821269198680511, -202.9817501106678321 ) ) ;
#3193 = CARTESIAN_POINT ( 'NONE',  ( 86.54078617439742516, 81.51664523006699881, -300.9066486022009599 ) ) ;
#3194 = CARTESIAN_POINT ( 'NONE',  ( 8.838160785872977598, -281.0073569661338411, -331.2382626041874687 ) ) ;
#3195 = CARTESIAN_POINT ( 'NONE',  ( 37.29967594461567870, -285.5814833268626671, -271.0765042700479057 ) ) ;
#3196 = CARTESIAN_POINT ( 'NONE',  ( -32.02081407409072256, -299.8780319020539196, -194.3728757402488441 ) ) ;
#3197 = CARTESIAN_POINT ( 'NONE',  ( -75.68501931998575571, -296.0709155532713908, -332.6115627939650494 ) ) ;
#3198 = ORIENTED_EDGE ( 'NONE', *, *, #88532, .F. ) ;
#3199 = CARTESIAN_POINT ( 'NONE',  ( 23.76049941203009652, -291.6736650922729837, -229.5228431721685922 ) ) ;
#3200 = CARTESIAN_POINT ( 'NONE',  ( -112.3042237070368969, -279.4182610784516783, -253.2166481482915970 ) ) ;
#3201 = CARTESIAN_POINT ( 'NONE',  ( 9.485080266334289689, -274.7168091038886928, -214.2926665229085756 ) ) ;
#3202 = CARTESIAN_POINT ( 'NONE',  ( 29.68409321610350560, -273.9862011148551915, -232.9821150870422457 ) ) ;
#3203 = DIRECTION ( 'NONE',  ( -1.000000000000000000, -0.000000000000000000, -0.000000000000000000 ) ) ;
#3204 = CARTESIAN_POINT ( 'NONE',  ( 11.87504125697724611, -272.7353163065756121, -213.7007498005672232 ) ) ;
#3205 = CARTESIAN_POINT ( 'NONE',  ( 21.84186392373628749, -295.6313442226972938, -318.7129388050902890 ) ) ;
#3206 = DIRECTION ( 'NONE',  ( 1.000000000000000000, 0.000000000000000000, 0.000000000000000000 ) ) ;
#3207 = CARTESIAN_POINT ( 'NONE',  ( -43.32098233076673921, -270.7600516457314939, -505.4240078839325179 ) ) ;
#3208 = CARTESIAN_POINT ( 'NONE',  ( -109.9201869115441781, -285.7674474160023692, -260.0369071200122448 ) ) ;
#3209 = CARTESIAN_POINT ( 'NONE',  ( 35.20154015585742968, -283.0243865427275409, -247.7458067330712197 ) ) ;
#3210 = CARTESIAN_POINT ( 'NONE',  ( -76.18830825081796831, -282.9345695676315700, -332.3470213345502202 ) ) ;
#3211 = CARTESIAN_POINT ( 'NONE',  ( -51.45359808223236797, -275.6354948520724406, -342.7993313043730836 ) ) ;
#3212 = CARTESIAN_POINT ( 'NONE',  ( 31.48851192887348205, -283.7787441181668555, -298.1688037236652917 ) ) ;
#3213 = CARTESIAN_POINT ( 'NONE',  ( -36.47728199580403441, -275.5210373603086964, -344.0619698814880962 ) ) ;
#3214 = CARTESIAN_POINT ( 'NONE',  ( 13.70207272223562178, -275.8679550096711637, -217.7421164110424172 ) ) ;
#3215 = DIRECTION ( 'NONE',  ( 0.000000000000000000, 1.000000000000000000, 0.000000000000000000 ) ) ;
#3216 = EDGE_CURVE ( 'NONE', #6956, #36970, #44399, .T. ) ;
#3217 = CARTESIAN_POINT ( 'NONE',  ( -31.09709954890292494, -280.9318436103359886, -193.7241804183869931 ) ) ;
#3218 = CARTESIAN_POINT ( 'NONE',  ( 20.07857662489317008, -281.3494650320590722, -219.1315579260468382 ) ) ;
#3219 = ORIENTED_EDGE ( 'NONE', *, *, #24991, .F. ) ;
#3220 = CARTESIAN_POINT ( 'NONE',  ( -35.09237171215954731, -122.5496321078137356, 22.50000000000000000 ) ) ;
#3221 = CARTESIAN_POINT ( 'NONE',  ( -15.78790135731870947, -288.1883546324197596, -197.6723359921274437 ) ) ;
#3222 = CARTESIAN_POINT ( 'NONE',  ( -37.00505171732093856, -294.2449637719207658, -343.5342719649205492 ) ) ;
#3223 = CARTESIAN_POINT ( 'NONE',  ( -113.2607411498891281, -289.7475656991182973, -282.5927162835344006 ) ) ;
#3224 = CARTESIAN_POINT ( 'NONE',  ( 34.37596487510375454, -285.5532896977239261, -252.0191782791793003 ) ) ;
#3226 = CARTESIAN_POINT ( 'NONE',  ( -57.91541754910730333, -290.0227392740632126, -199.2111255646440213 ) ) ;
#3225 = CARTESIAN_POINT ( 'NONE',  ( 36.21814932527016850, -286.1719439005656795, -273.8053620493907943 ) ) ;
#3227 = CARTESIAN_POINT ( 'NONE',  ( -22.39388310276886429, -287.4527762011890104, -198.4501148162585196 ) ) ;
#3228 = CARTESIAN_POINT ( 'NONE',  ( -83.65198204334981824, -275.6869242687699284, -329.4216884099090521 ) ) ;
#3229 = CARTESIAN_POINT ( 'NONE',  ( 32.12710830490041758, -286.3562172689345289, -301.6744548911016182 ) ) ;
#3230 = CARTESIAN_POINT ( 'NONE',  ( -18.70430708143557652, -288.2921875845780733, -197.6600272521977786 ) ) ;
#3231 = CARTESIAN_POINT ( 'NONE',  ( 37.74772135464480272, -285.4955006648787617, -265.9519459777102384 ) ) ;
#3232 = CARTESIAN_POINT ( 'NONE',  ( 35.37489605523790459, -282.6132585092693716, -279.4756645447856727 ) ) ;
#3233 = CARTESIAN_POINT ( 'NONE',  ( -0.1647487453744717611, -290.5593828577046907, -335.7491328647454907 ) ) ;
#3234 = CARTESIAN_POINT ( 'NONE',  ( 189.9243309297870610, 215.0000000000000568, 25.22542485937348644 ) ) ;
#3235 = EDGE_CURVE ( 'NONE', #62642, #12065, #46260, .T. ) ;
#3236 = CARTESIAN_POINT ( 'NONE',  ( 155.0193286407019002, 19.71512530817393127, -13.29403319965122066 ) ) ;
#3237 = CARTESIAN_POINT ( 'NONE',  ( -112.9250856760444748, -298.4456253468944169, -272.4547568002766411 ) ) ;
#3238 = CARTESIAN_POINT ( 'NONE',  ( 33.88377705627229375, -279.2465434819816323, -246.7040258299916218 ) ) ;
#3239 = CARTESIAN_POINT ( 'NONE',  ( -47.71145770650421269, -291.1208084651235026, -194.1718542637828762 ) ) ;
#3240 = CARTESIAN_POINT ( 'NONE',  ( -92.80522687419166061, -294.2646205408400419, -319.0462041717752300 ) ) ;
#3241 = CARTESIAN_POINT ( 'NONE',  ( 11.64691924035343717, -279.4341169229158481, -215.5764609222925685 ) ) ;
#3242 = CARTESIAN_POINT ( 'NONE',  ( -67.62128913285192766, -271.7316188445224157, -202.3437700395113268 ) ) ;
#3243 = CARTESIAN_POINT ( 'NONE',  ( -68.71273156986022457, -296.7884836583860988, -336.8362218243789812 ) ) ;
#3244 = CARTESIAN_POINT ( 'NONE',  ( -95.56682381678963623, -271.7992918970323899, -220.8592517632580723 ) ) ;
#3245 = CARTESIAN_POINT ( 'NONE',  ( 8.279646956727130913, -292.6772831150340721, -331.1284340458325346 ) ) ;
#3246 = CARTESIAN_POINT ( 'NONE',  ( -0.9812017884011294822, -293.9701704699788252, -206.3677102599160946 ) ) ;
#3247 = DIRECTION ( 'NONE',  ( 1.000000000000000000, 0.000000000000000000, 0.000000000000000000 ) ) ;
#3248 = CARTESIAN_POINT ( 'NONE',  ( 32.78091438322449136, -294.0773592550401645, -249.3198927158008473 ) ) ;
#3249 = EDGE_CURVE ( 'NONE', #71226, #4269, #76566, .T. ) ;
#3250 = FACE_BOUND ( 'NONE', #1362, .T. ) ;
#3252 = CARTESIAN_POINT ( 'NONE',  ( -41.03921944085710294, -295.0999438261267755, -343.2799837038897977 ) ) ;
#3251 = CARTESIAN_POINT ( 'NONE',  ( -94.11255491464412160, -281.8875079250580029, -319.9138863375851543 ) ) ;
#3253 = CARTESIAN_POINT ( 'NONE',  ( 22.52326512964628336, -282.2017200253790747, -318.8090409811625818 ) ) ;
#3254 = CARTESIAN_POINT ( 'NONE',  ( -22.86645706011551127, -282.1559836653042908, -196.1473679702848187 ) ) ;
#3255 = CARTESIAN_POINT ( 'NONE',  ( -7.347449989516855240, -286.1014655196306649, -199.4095594324957688 ) ) ;
#3256 = CARTESIAN_POINT ( 'NONE',  ( -111.6121051130163693, -288.4340928879395847, -279.5227427972042733 ) ) ;
#3257 = CARTESIAN_POINT ( 'NONE',  ( -30.29833455534296860, -281.4444596772003138, -346.3420284385918535 ) ) ;
#3258 = CARTESIAN_POINT ( 'NONE',  ( 5.373708009634825089, -287.4089358795773705, -334.0548101093624496 ) ) ;
#3259 = CARTESIAN_POINT ( 'NONE',  ( 139.1539576904058606, 250.0000000000000568, 10.50000000000000000 ) ) ;
#3260 = CARTESIAN_POINT ( 'NONE',  ( -89.04797160909069476, -297.3936470175174236, -323.0912663003654757 ) ) ;
#3261 = CARTESIAN_POINT ( 'NONE',  ( 37.02265668121343367, -277.1994463476847841, -287.9830897149314524 ) ) ;
#3263 = CARTESIAN_POINT ( 'NONE',  ( -107.6375145660343691, -278.4805832761761621, -250.5515366300710127 ) ) ;
#3262 = CARTESIAN_POINT ( 'NONE',  ( 37.59847648380248586, -291.6793053756771883, -278.7376271320996466 ) ) ;
#3264 = CARTESIAN_POINT ( 'NONE',  ( 38.32484388043344126, -293.5403911187398762, -256.0931776150931682 ) ) ;
#3265 = CARTESIAN_POINT ( 'NONE',  ( -75.36061662161361596, -283.6296659964604601, -205.0025134999579564 ) ) ;
#3266 = CARTESIAN_POINT ( 'NONE',  ( -56.39080640651074106, -279.2976468192235870, -342.9552907756294644 ) ) ;
#3267 = CARTESIAN_POINT ( 'NONE',  ( -1.129938079112184912, -291.6040282042743002, -206.6903560878875226 ) ) ;
#3268 = CARTESIAN_POINT ( 'NONE',  ( -99.67364875471277230, -271.1200460979784452, -228.2594931903377073 ) ) ;
#3269 = ORIENTED_EDGE ( 'NONE', *, *, #11007, .T. ) ;
#3270 = DIRECTION ( 'NONE',  ( -0.000000000000000000, -0.000000000000000000, -1.000000000000000000 ) ) ;
#3271 = CARTESIAN_POINT ( 'NONE',  ( 33.36934294880997243, -292.8173123691423143, -251.9780597820586650 ) ) ;
#3272 = DIRECTION ( 'NONE',  ( 1.000000000000000000, 0.000000000000000000, 0.000000000000000000 ) ) ;
#3273 = CARTESIAN_POINT ( 'NONE',  ( -6.998514795304330072, -286.1237833571631768, -333.4427485647536855 ) ) ;
#3274 = CARTESIAN_POINT ( 'NONE',  ( -33.33765991442466259, -297.1598859787685569, -193.5970321323677865 ) ) ;
#3275 = CARTESIAN_POINT ( 'NONE',  ( -35.17906740486936457, -287.3939084084247497, -193.8717792726471600 ) ) ;
#3276 = CARTESIAN_POINT ( 'NONE',  ( 30.48439716770303676, -287.7482690112159958, -297.4904141672690230 ) ) ;
#3277 = CARTESIAN_POINT ( 'NONE',  ( -103.7474611906482949, -279.6426332942239128, -302.4319490299551489 ) ) ;
#3278 = CARTESIAN_POINT ( 'NONE',  ( -84.74074546509368133, -299.1489603889610294, -213.4496210277129933 ) ) ;
#3279 = CARTESIAN_POINT ( 'NONE',  ( -39.69869221830266781, -278.8168503100827138, -196.9893103965865748 ) ) ;
#3280 = EDGE_LOOP ( 'NONE', ( #62154, #23611, #77651, #73879 ) ) ;
#3281 = CARTESIAN_POINT ( 'NONE',  ( -9.115682335510763679, -298.0632170819999374, -193.3838024440057382 ) ) ;
#3282 = CARTESIAN_POINT ( 'NONE',  ( -0.5661350211931107657, -294.4649723526099478, -205.6248638718004145 ) ) ;
#3283 = CARTESIAN_POINT ( 'NONE',  ( 32.58212755522404080, -294.7623062535610643, -240.0774798978839613 ) ) ;
#3284 = DIRECTION ( 'NONE',  ( -0.000000000000000000, -1.000000000000000000, -0.000000000000000000 ) ) ;
#3285 = CARTESIAN_POINT ( 'NONE',  ( -98.92317465171700519, -290.6594618712950933, -309.7516582634343081 ) ) ;
#3286 = DIRECTION ( 'NONE',  ( 0.000000000000000000, 0.000000000000000000, 1.000000000000000000 ) ) ;
#3287 = CARTESIAN_POINT ( 'NONE',  ( 28.41554031329198082, -291.1948374564298661, -232.7274786695991793 ) ) ;
#3289 = CARTESIAN_POINT ( 'NONE',  ( -72.85345360504487644, -297.2344932337986734, -206.5567070707547828 ) ) ;
#3288 = AXIS2_PLACEMENT_3D ( 'NONE', #82985, #37672, #54112 ) ;
#3290 = CARTESIAN_POINT ( 'NONE',  ( 165.0427047786672290, 275.5000000000000568, 23.37680765314704701 ) ) ;
#3291 = FACE_BOUND ( 'NONE', #79678, .T. ) ;
#3292 = CARTESIAN_POINT ( 'NONE',  ( -110.8686674365253282, -291.8142579168338671, -290.7692740041106845 ) ) ;
#3293 = CARTESIAN_POINT ( 'NONE',  ( 36.60358173371528068, -290.4805209788416391, -305.9350535429201159 ) ) ;
#3294 = CARTESIAN_POINT ( 'NONE',  ( -37.30491739858693734, -288.0527346028062539, -195.5150379833580416 ) ) ;
#3295 = CARTESIAN_POINT ( 'NONE',  ( -13.45676503978470251, -272.3628528579907311, -199.4418801069632252 ) ) ;
#3296 = CARTESIAN_POINT ( 'NONE',  ( 1.340272797033512653, -276.4934163097516375, -206.7606528268024135 ) ) ;
#3298 = CARTESIAN_POINT ( 'NONE',  ( 22.15926449107730534, -291.0160333956610543, -225.6291449652785275 ) ) ;
#3297 = AXIS2_PLACEMENT_3D ( 'NONE', #86504, #22132, #85589 ) ;
#3299 = CARTESIAN_POINT ( 'NONE',  ( -77.14549112972787270, -279.4396016717453790, -334.8888388176876560 ) ) ;
#3300 = EDGE_LOOP ( 'NONE', ( #76937, #7294, #62037 ) ) ;
#3301 = CARTESIAN_POINT ( 'NONE',  ( -69.06088858312446632, -282.8292890359639955, -336.2368098477783178 ) ) ;
#3302 = CARTESIAN_POINT ( 'NONE',  ( -94.96939602140655268, -278.9442615027691659, -320.9629082307384920 ) ) ;
#3303 = EDGE_CURVE ( 'NONE', #24040, #7041, #77458, .T. ) ;
#3304 = CARTESIAN_POINT ( 'NONE',  ( 37.86777583068692365, -280.1642391187898511, -255.8165847958368033 ) ) ;
#3305 = CARTESIAN_POINT ( 'NONE',  ( -64.37108594678602458, -181.9596566217732914, -359.3138851375881586 ) ) ;
#3306 = CARTESIAN_POINT ( 'NONE',  ( 39.38880183194059725, -276.5393117308727824, -274.0207565710887820 ) ) ;
#3307 = APPLICATION_PROTOCOL_DEFINITION ( 'draft international standard', 'automotive_design', 1998, #17230 ) ;
#3308 = CARTESIAN_POINT ( 'NONE',  ( -4.145390490588479082, -276.0020011739800907, -201.6392988562928679 ) ) ;
#3309 = CARTESIAN_POINT ( 'NONE',  ( -69.85430415644619018, -297.9805209788416391, -337.9475929042657754 ) ) ;
#3310 = ORIENTED_EDGE ( 'NONE', *, *, #24948, .F. ) ;
#3311 = EDGE_LOOP ( 'NONE', ( #33346, #66788, #7493 ) ) ;
#3312 = CARTESIAN_POINT ( 'NONE',  ( 194.3144103428324172, 215.0000000000000568, 16.91223866672520515 ) ) ;
#3313 = CARTESIAN_POINT ( 'NONE',  ( -70.09826347096063159, -290.5738688192431596, -335.9588250696023124 ) ) ;
#3314 = CARTESIAN_POINT ( 'NONE',  ( -41.68000079072222519, -290.8662038289725160, -346.2368919982716307 ) ) ;
#3315 = CARTESIAN_POINT ( 'NONE',  ( -109.3757603311664184, -290.0685400739879469, -257.6229172631110487 ) ) ;
#3316 = CARTESIAN_POINT ( 'NONE',  ( 9.778015517621573949, -286.1891212163698128, -209.5395814965136196 ) ) ;
#3317 = DIRECTION ( 'NONE',  ( 0.000000000000000000, 0.000000000000000000, 1.000000000000000000 ) ) ;
#3318 = CARTESIAN_POINT ( 'NONE',  ( 30.03661558084898786, -280.3545769650451689, -300.5963633306288898 ) ) ;
#3319 = CARTESIAN_POINT ( 'NONE',  ( 24.55222554496365106, -289.9720976208146794, -311.3722411185597139 ) ) ;
#3320 = CARTESIAN_POINT ( 'NONE',  ( -45.73750329682886218, -281.6402312371427001, -343.6261088063008629 ) ) ;
#3321 = CARTESIAN_POINT ( 'NONE',  ( 34.71750494821791477, -283.0574604377915762, -284.8714733654586553 ) ) ;
#3322 = CARTESIAN_POINT ( 'NONE',  ( 39.46722419409472593, -288.5081374216714494, -271.5356888175278982 ) ) ;
#3323 = CARTESIAN_POINT ( 'NONE',  ( -108.3509578115677812, -279.2711797265430391, -253.1659510713735131 ) ) ;
#3324 = CARTESIAN_POINT ( 'NONE',  ( -98.02425376813560831, -289.9744038353175597, -223.5891087115241191 ) ) ;
#3325 = CARTESIAN_POINT ( 'NONE',  ( -57.72296622173877267, -286.5984343889253978, -196.2196953537114723 ) ) ;
#3326 = CARTESIAN_POINT ( 'NONE',  ( 24.64996416893101738, -287.4387019231546105, -224.7918250204139099 ) ) ;
#3327 = CARTESIAN_POINT ( 'NONE',  ( -104.1124439977133562, -284.3217342683776110, -299.8681979394119708 ) ) ;
#3328 = ORIENTED_EDGE ( 'NONE', *, *, #46568, .F. ) ;
#3329 = CARTESIAN_POINT ( 'NONE',  ( 222.4306832106270804, 15.36528803885690664, 21.50000000000000000 ) ) ;
#3330 = CARTESIAN_POINT ( 'NONE',  ( -3.888440784880806689, -294.3490796603538797, -202.3675184288472053 ) ) ;
#3331 = CARTESIAN_POINT ( 'NONE',  ( 36.94713547685543631, -292.0067257337372553, -252.0726741169643788 ) ) ;
#3332 = CARTESIAN_POINT ( 'NONE',  ( 31.47876952186530630, -274.9452595870853884, -295.5514066198417140 ) ) ;
#3333 = ADVANCED_FACE ( 'NONE', ( #83643 ), #32309, .T. ) ;
#3334 = CARTESIAN_POINT ( 'NONE',  ( -24.93244843925003806, -294.2465778989452474, -346.3053164935913060 ) ) ;
#3335 = CARTESIAN_POINT ( 'NONE',  ( -109.0981875987010739, -289.2520776972204999, -253.5218018858991798 ) ) ;
#3336 = CARTESIAN_POINT ( 'NONE',  ( 18.72559985069543842, -292.4709175641842194, -318.6963935335374458 ) ) ;
#3337 = CARTESIAN_POINT ( 'NONE',  ( -91.06020840915365966, -292.4726279651912932, -220.3280093818309240 ) ) ;
#3338 = DIRECTION ( 'NONE',  ( 0.000000000000000000, 0.000000000000000000, 1.000000000000000000 ) ) ;
#3339 = CARTESIAN_POINT ( 'NONE',  ( 23.34960531646590098, -290.9489093174582877, -226.0148230720368474 ) ) ;
#3340 = CARTESIAN_POINT ( 'NONE',  ( 7.105927811645549319, -296.4473943804986789, -330.8352197173951481 ) ) ;
#3341 = CARTESIAN_POINT ( 'NONE',  ( -15.77094140479450068, -289.7075302732210389, -340.4006211466099217 ) ) ;
#3342 = CARTESIAN_POINT ( 'NONE',  ( 23.06459478745229319, -278.1443693137554192, -315.4109386283270169 ) ) ;
#3343 = CARTESIAN_POINT ( 'NONE',  ( -37.14348105266689970, -275.8446178746968940, -346.9767815062695604 ) ) ;
#3344 = CARTESIAN_POINT ( 'NONE',  ( -67.48802892612940241, -273.0155328330564544, -199.6185448967968625 ) ) ;
#3345 = CARTESIAN_POINT ( 'NONE',  ( -49.35059724476386833, -277.9777276013978735, -196.8961563645111426 ) ) ;
#3346 = CARTESIAN_POINT ( 'NONE',  ( -23.10852334831740862, -275.2730393374979485, -345.2736523688169541 ) ) ;
#3347 = EDGE_CURVE ( 'NONE', #29030, #26503, #47183, .T. ) ;
#3348 = CARTESIAN_POINT ( 'NONE',  ( -108.0820080083184394, -294.9753395334382731, -290.2872897124192946 ) ) ;
#3349 = CARTESIAN_POINT ( 'NONE',  ( 144.7857639756989272, -299.5541904835127980, -195.3611179825600175 ) ) ;
#3350 = CARTESIAN_POINT ( 'NONE',  ( -62.07197012466863839, -274.3733237499686197, -201.5693567460409668 ) ) ;
#3351 = FACE_OUTER_BOUND ( 'NONE', #71825, .T. ) ;
#3352 = VECTOR ( 'NONE', #12074, 1000.000000000000000 ) ;
#3354 = CARTESIAN_POINT ( 'NONE',  ( -24.59434719683853743, -274.0525546230624059, -198.4311249685764267 ) ) ;
#3353 = CARTESIAN_POINT ( 'NONE',  ( -15.45460456147322859, -286.7904845927549218, -342.5222730165527310 ) ) ;
#3355 = AXIS2_PLACEMENT_3D ( 'NONE', #38183, #74661, #10239 ) ;
#3356 = CARTESIAN_POINT ( 'NONE',  ( 30.36269043639126508, -288.0278526685917768, -307.1484451448854429 ) ) ;
#3357 = CARTESIAN_POINT ( 'NONE',  ( -9.884553245675764543, -300.3741332763799505, -194.9966984203866218 ) ) ;
#3358 = CARTESIAN_POINT ( 'NONE',  ( -97.90682274181324374, -293.9517282735380377, -314.3363195487081043 ) ) ;
#3359 = CIRCLE ( 'NONE', #409, 4.999999999999986677 ) ;
#3360 = CARTESIAN_POINT ( 'NONE',  ( -66.52441117905529211, -282.6219065637503718, -341.4564131871359791 ) ) ;
#3361 = CARTESIAN_POINT ( 'NONE',  ( 200.6103193995254230, 275.0000000000000568, -2.464576988612312114 ) ) ;
#3362 = VECTOR ( 'NONE', #69642, 1000.000000000000000 ) ;
#3363 = CARTESIAN_POINT ( 'NONE',  ( -112.2859399133422329, -276.5005673606524965, -274.3658439002661567 ) ) ;
#3364 = LINE ( 'NONE', #90445, #82186 ) ;
#3365 = CARTESIAN_POINT ( 'NONE',  ( -107.3759221028292785, -289.6370752132515918, -248.3566074674033644 ) ) ;
#3366 = LINE ( 'NONE', #1507, #39639 ) ;
#3367 = ADVANCED_FACE ( 'NONE', ( #32552 ), #90725, .F. ) ;
#3368 = DIRECTION ( 'NONE',  ( -0.000000000000000000, 1.000000000000000000, -0.000000000000000000 ) ) ;
#3369 = CARTESIAN_POINT ( 'NONE',  ( -67.34130092343009721, -289.6585701269480637, -201.6223035945419042 ) ) ;
#3370 = CARTESIAN_POINT ( 'NONE',  ( -49.00406835077139789, -275.4211536965879645, -197.5447889531275791 ) ) ;
#3371 = CARTESIAN_POINT ( 'NONE',  ( 29.25731011628556999, -283.4683831290116700, -307.9280178847054117 ) ) ;
#3373 = CARTESIAN_POINT ( 'NONE',  ( -104.1132998724246619, -284.1550810543499779, -299.8662610525607874 ) ) ;
#3372 = CARTESIAN_POINT ( 'NONE',  ( -77.30828217564319971, -295.5390933722094360, -206.4777937018711782 ) ) ;
#3374 = CARTESIAN_POINT ( 'NONE',  ( -38.10654969369583256, -275.4676571440381849, -196.7758618226220619 ) ) ;
#3375 = CARTESIAN_POINT ( 'NONE',  ( 31.26620542559711069, -276.0169261289804581, -244.9533037860313129 ) ) ;
#3376 = CARTESIAN_POINT ( 'NONE',  ( -8.776404072727224559, -284.6787398149948558, -339.7633288188958431 ) ) ;
#3377 = ORIENTED_EDGE ( 'NONE', *, *, #93547, .F. ) ;
#3378 = CARTESIAN_POINT ( 'NONE',  ( 60.83289261295102079, -250.0118895884541530, -21.50000000000000000 ) ) ;
#3379 = CARTESIAN_POINT ( 'NONE',  ( 0.5386532627527429451, -294.3950790960922745, -337.4141883416912719 ) ) ;
#3380 = CARTESIAN_POINT ( 'NONE',  ( -111.5039782348854089, -286.4169941999679168, -279.2793477202540657 ) ) ;
#3381 = CARTESIAN_POINT ( 'NONE',  ( 156.4851178187871312, 3.000000000000000000, -7.000000000000000888 ) ) ;
#3382 = CARTESIAN_POINT ( 'NONE',  ( 36.60358173371529489, -284.6237833571632905, -234.7871824221999191 ) ) ;
#3383 = CARTESIAN_POINT ( 'NONE',  ( -54.10599870879289597, -276.4591646791535595, -345.4030915490043867 ) ) ;
#3384 = CARTESIAN_POINT ( 'NONE',  ( -91.04928535344082263, -288.1990336665144241, -324.4902966406356768 ) ) ;
#3385 = CARTESIAN_POINT ( 'NONE',  ( -70.30981510752965846, -287.1296922317927738, -204.4394443781715722 ) ) ;
#3386 = CARTESIAN_POINT ( 'NONE',  ( 3.714587149990489667, -278.2513697288731578, -331.9432199836292057 ) ) ;
#3387 = CARTESIAN_POINT ( 'NONE',  ( -68.27895474457298519, -287.0789885570061415, -200.4791708890046777 ) ) ;
#3388 = CARTESIAN_POINT ( 'NONE',  ( 13.28499688721336724, -284.3442213100884146, -325.6959008563357543 ) ) ;
#3389 = CARTESIAN_POINT ( 'NONE',  ( -20.12403930961524168, -277.0036265471377988, -345.4661680429287571 ) ) ;
#3390 = CARTESIAN_POINT ( 'NONE',  ( -106.3463232545784791, -277.9450047232013503, -304.6477661944054489 ) ) ;
#3391 = CARTESIAN_POINT ( 'NONE',  ( -111.8245872750670031, -298.4574600745342536, -271.5092575864684932 ) ) ;
#3392 = CARTESIAN_POINT ( 'NONE',  ( 140.6539576904058606, 131.0000000000000568, -11.50000000000000000 ) ) ;
#3393 = DIRECTION ( 'NONE',  ( 0.000000000000000000, 0.000000000000000000, 1.000000000000000000 ) ) ;
#3394 = CARTESIAN_POINT ( 'NONE',  ( -37.23121733014565393, -296.1931139969674973, -194.5955937437999523 ) ) ;
#3395 = CARTESIAN_POINT ( 'NONE',  ( 202.9738562182569694, 293.9636489450776367, -54.00000000000000000 ) ) ;
#3396 = CARTESIAN_POINT ( 'NONE',  ( -91.01731910912383228, -277.3478396063592868, -320.0020066101476459 ) ) ;
#3397 = CARTESIAN_POINT ( 'NONE',  ( -68.69565184611099085, -274.8542161595667608, -200.4544609531145340 ) ) ;
#3398 = CARTESIAN_POINT ( 'NONE',  ( 38.19189227883794047, -280.7835932419579876, -284.1270094048365422 ) ) ;
#3399 = CARTESIAN_POINT ( 'NONE',  ( 35.56163497104553528, -289.1423880664242461, -257.3023228312590618 ) ) ;
#3400 = CARTESIAN_POINT ( 'NONE',  ( -61.35485033385133846, -296.8784525281200786, -342.8461524688852933 ) ) ;
#3401 = CARTESIAN_POINT ( 'NONE',  ( -47.56332316031804197, -296.3844183213226415, -346.2790153482373512 ) ) ;
#3402 = CARTESIAN_POINT ( 'NONE',  ( 16.16908601960792780, -294.8132240842397778, -217.9741721522336206 ) ) ;
#3403 = CARTESIAN_POINT ( 'NONE',  ( -8.518242664795220520, -278.4301388005070521, -201.3014573404978478 ) ) ;
#3404 = CARTESIAN_POINT ( 'NONE',  ( 21.64223775218759371, -282.8452870759924167, -224.9288560693948398 ) ) ;
#3405 = CARTESIAN_POINT ( 'NONE',  ( -35.06874290883403233, -296.1606666266059733, -195.9218606051179563 ) ) ;
#3406 = CARTESIAN_POINT ( 'NONE',  ( -76.33086043225696926, -285.1640202527632368, -335.8920178884321217 ) ) ;
#3407 = CARTESIAN_POINT ( 'NONE',  ( 29.70220634126613746, -286.8713741452664863, -300.1406900055482652 ) ) ;
#3408 = CARTESIAN_POINT ( 'NONE',  ( -37.81643920958603644, -140.6726492126896346, -364.1437749989735835 ) ) ;
#3409 = EDGE_LOOP ( 'NONE', ( #92381, #68975, #16468, #27296, #33854 ) ) ;
#3410 = CARTESIAN_POINT ( 'NONE',  ( 34.77943607890461664, -287.3706479215621812, -281.8700862883184755 ) ) ;
#3411 = ORIENTED_EDGE ( 'NONE', *, *, #84671, .F. ) ;
#3412 = CARTESIAN_POINT ( 'NONE',  ( -111.5722864269859116, -285.3890799960030904, -289.6826170217073013 ) ) ;
#3413 = CARTESIAN_POINT ( 'NONE',  ( 31.28308989514621530, -276.2195874349703786, -295.4625486652283826 ) ) ;
#3414 = CARTESIAN_POINT ( 'NONE',  ( 9.579703076757906999, -285.4765073871970458, -209.8103901689671318 ) ) ;
#3415 = CARTESIAN_POINT ( 'NONE',  ( -97.21358883384220917, -290.1170594236804732, -222.4356607155498011 ) ) ;
#3416 = CARTESIAN_POINT ( 'NONE',  ( 37.44553721366549581, -282.2755764260394926, -252.9918664540992097 ) ) ;
#3417 =( NAMED_UNIT ( * ) PLANE_ANGLE_UNIT ( ) SI_UNIT ( $, .RADIAN. ) );
#3418 = CARTESIAN_POINT ( 'NONE',  ( -56.40234970307031404, -281.3311188052444436, -196.4188603925978498 ) ) ;
#3419 = CARTESIAN_POINT ( 'NONE',  ( 39.50835230792633723, -281.9516607562512149, -275.6552146410106729 ) ) ;
#3420 = CARTESIAN_POINT ( 'NONE',  ( 17.40634833298269157, -278.4094976428775681, -226.7417163044926838 ) ) ;
#3421 = ORIENTED_EDGE ( 'NONE', *, *, #30621, .F. ) ;
#3422 = AXIS2_PLACEMENT_3D ( 'NONE', #9639, #81603, #51330 ) ;
#3423 = CARTESIAN_POINT ( 'NONE',  ( 37.18202074190754303, -277.6398253042544297, -277.1613718337236492 ) ) ;
#3424 = CARTESIAN_POINT ( 'NONE',  ( -113.0202178868561447, -270.5102741164896543, -296.2292133334984783 ) ) ;
#3425 = AXIS2_PLACEMENT_3D ( 'NONE', #85327, #79169, #22323 ) ;
#3426 = CARTESIAN_POINT ( 'NONE',  ( 20.11802656611209628, -278.9112657782015958, -222.6943762391129553 ) ) ;
#3427 = CARTESIAN_POINT ( 'NONE',  ( -69.29461257921681749, -296.9688094375072751, -204.6123229025582759 ) ) ;
#3428 = CARTESIAN_POINT ( 'NONE',  ( -95.61020414936773193, -290.7389932783574977, -220.0984873618251640 ) ) ;
#3429 = CARTESIAN_POINT ( 'NONE',  ( -97.39219751932952818, -246.9239084015011656, -331.4851807666400987 ) ) ;
#3430 = AXIS2_PLACEMENT_3D ( 'NONE', #16645, #15259, #81046 ) ;
#3432 = CARTESIAN_POINT ( 'NONE',  ( 16.57268045031483794, -285.2347499314938091, -219.9472256863061546 ) ) ;
#3431 = CARTESIAN_POINT ( 'NONE',  ( -31.94293825058073466, -296.6932287952452612, -193.9516209903190997 ) ) ;
#3433 = CARTESIAN_POINT ( 'NONE',  ( 34.64963357485707718, -295.6476501391692864, -288.4750174734703592 ) ) ;
#3434 = CARTESIAN_POINT ( 'NONE',  ( -5.600728758618639169, -287.7937102271188223, -204.0618423320328816 ) ) ;
#3435 = ORIENTED_EDGE ( 'NONE', *, *, #9771, .T. ) ;
#3436 = CARTESIAN_POINT ( 'NONE',  ( 27.84619259727910290, -293.9603291448657956, -229.7223394935316492 ) ) ;
#3437 = VECTOR ( 'NONE', #19295, 1000.000000000000000 ) ;
#3438 = CARTESIAN_POINT ( 'NONE',  ( -98.16176580261897300, -285.6060052778029785, -229.8776886191627682 ) ) ;
#3439 = CARTESIAN_POINT ( 'NONE',  ( -47.59369798343985281, -293.9746551386352849, -346.2749194801295971 ) ) ;
#3440 = CARTESIAN_POINT ( 'NONE',  ( -98.02577560872533979, -290.7241780541166349, -317.4949890764902989 ) ) ;
#3441 = CARTESIAN_POINT ( 'NONE',  ( -33.54867469438197958, -292.5910424320822472, -193.5162101395644640 ) ) ;
#3442 = CARTESIAN_POINT ( 'NONE',  ( -72.35699666442870637, -289.6959892840354200, -334.4152280223494813 ) ) ;
#3443 = VERTEX_POINT ( 'NONE', #18807 ) ;
#3444 = DIRECTION ( 'NONE',  ( 0.000000000000000000, 0.000000000000000000, 1.000000000000000000 ) ) ;
#3445 = CARTESIAN_POINT ( 'NONE',  ( 96.44228902283924754, -301.5705273522572156, -194.5544052147834577 ) ) ;
#3446 = CARTESIAN_POINT ( 'NONE',  ( -87.76341052564968948, -272.1612075169296077, -212.6220725324359933 ) ) ;
#3447 = CARTESIAN_POINT ( 'NONE',  ( 34.29786879288168677, -280.4102106372642993, -255.0966938950409144 ) ) ;
#3448 = ORIENTED_EDGE ( 'NONE', *, *, #92749, .T. ) ;
#3449 = ORIENTED_EDGE ( 'NONE', *, *, #50173, .T. ) ;
#3450 = EDGE_CURVE ( 'NONE', #61449, #47327, #29358, .T. ) ;
#3451 = CARTESIAN_POINT ( 'NONE',  ( -1.324746964779585534, -274.0245518955879334, -202.3735750925492027 ) ) ;
#3452 = CARTESIAN_POINT ( 'NONE',  ( -110.0501149628585438, -294.8751095925890127, -282.3692054820198223 ) ) ;
#3453 = CARTESIAN_POINT ( 'NONE',  ( -91.85913063617145724, -279.7002230644374094, -320.8215270186369708 ) ) ;
#3454 = CARTESIAN_POINT ( 'NONE',  ( 27.73049027741052086, -273.2105888176850499, -234.5261222635036518 ) ) ;
#3455 = CARTESIAN_POINT ( 'NONE',  ( -108.2231049134757939, -298.0080769763791864, -251.2612192934299173 ) ) ;
#3456 = CARTESIAN_POINT ( 'NONE',  ( -110.1095834582196602, -297.5096961944851728, -279.6586303020674222 ) ) ;
#3457 = CARTESIAN_POINT ( 'NONE',  ( -112.9831370309887717, -298.2686637528121310, -261.1516968279346997 ) ) ;
#3458 = CARTESIAN_POINT ( 'NONE',  ( 28.52243080689648380, -273.0861252370503962, -233.6433321265610630 ) ) ;
#3459 = CARTESIAN_POINT ( 'NONE',  ( 35.30919848983042897, -294.3162414422748725, -278.9142396800737629 ) ) ;
#3460 = CARTESIAN_POINT ( 'NONE',  ( -36.17875722034020214, -290.6417042956522891, -196.7684997398745566 ) ) ;
#3461 = FACE_OUTER_BOUND ( 'NONE', #37309, .T. ) ;
#3462 = CARTESIAN_POINT ( 'NONE',  ( 37.22403684347696640, -275.8070578647080424, -251.4012188966840995 ) ) ;
#3463 = CARTESIAN_POINT ( 'NONE',  ( -68.28450880347773477, -273.8007633457644943, -204.2297779361963990 ) ) ;
#3464 = CARTESIAN_POINT ( 'NONE',  ( 33.06000806390615310, -283.8796350802811617, -297.2312926088651466 ) ) ;
#3465 =( BOUNDED_CURVE ( )  B_SPLINE_CURVE ( 3, ( #12358, #18522, #40276, #48327 ),
 .UNSPECIFIED., .F., .F. ) 
 B_SPLINE_CURVE_WITH_KNOTS ( ( 4, 4 ),
 ( 1.570796326794896780, 3.141592653589793116 ),
 .UNSPECIFIED. ) 
 CURVE ( )  GEOMETRIC_REPRESENTATION_ITEM ( )  RATIONAL_B_SPLINE_CURVE ( ( 1.000000000000000000, 0.8047378541243650485, 0.8047378541243650485, 1.000000000000000000 ) ) 
 REPRESENTATION_ITEM ( '' )  );
#3466 = CARTESIAN_POINT ( 'NONE',  ( -37.33124170232879635, -281.7368201097845031, -346.8809497115246359 ) ) ;
#3467 = VECTOR ( 'NONE', #39809, 1000.000000000000114 ) ;
#3468 = CYLINDRICAL_SURFACE ( 'NONE', #29402, 25.00000000000000355 ) ;
#3469 =( BOUNDED_SURFACE ( )  B_SPLINE_SURFACE ( 3, 2, ( 
 ( #14695, #57777, #86622 ),
 ( #63964, #43550, #87097 ),
 ( #72446, #22247, #51117 ),
 ( #7565, #36450, #65365 ) ),
 .UNSPECIFIED., .F., .F., .F. ) 
 B_SPLINE_SURFACE_WITH_KNOTS ( ( 4, 4 ),
 ( 3, 3 ),
 ( 4.278565243615663150, 4.712388980384689674 ),
 ( 0.000000000000000000, 1.000000000000000000 ),
 .UNSPECIFIED. ) 
 GEOMETRIC_REPRESENTATION_ITEM ( )  RATIONAL_B_SPLINE_SURFACE ( (
 ( 1.000000000000000000, 0.8168508380123955526, 1.000000000000000000),
 ( 1.000000000000000000, 0.7849082635113585615, 1.000000000000000000),
 ( 1.000000000000000000, 0.7478056585118741939, 1.000000000000000000),
 ( 1.000000000000000000, 0.7071067811865482389, 1.000000000000000000) ) ) 
 REPRESENTATION_ITEM ( '' )  SURFACE ( )  );
#3470 = CARTESIAN_POINT ( 'NONE',  ( -104.2651214110867102, -283.3523776848874149, -299.9221972969260719 ) ) ;
#3471 = CARTESIAN_POINT ( 'NONE',  ( -70.94262198748015180, -281.4943253504089284, -337.5995480718307249 ) ) ;
#3472 = EDGE_CURVE ( 'NONE', #2187, #79053, #42928, .T. ) ;
#3473 = CARTESIAN_POINT ( 'NONE',  ( 33.07497690071242857, -274.4081549606615908, -291.7791999513033261 ) ) ;
#3474 = CARTESIAN_POINT ( 'NONE',  ( -23.79561910030680849, -282.2252611632882804, -196.5423384039622192 ) ) ;
#3475 = LINE ( 'NONE', #40825, #76092 ) ;
#3476 = CARTESIAN_POINT ( 'NONE',  ( 194.7453183674696220, 20.99999999999999645, 15.62500000000048850 ) ) ;
#3477 = CARTESIAN_POINT ( 'NONE',  ( -87.49435193961841151, -271.7662184468114219, -212.9224195425988171 ) ) ;
#3478 = CARTESIAN_POINT ( 'NONE',  ( -110.6897125428610025, -280.3417573901916739, -286.7957614591096558 ) ) ;
#3479 = CARTESIAN_POINT ( 'NONE',  ( 208.4306832106271088, 0.000000000000000000, 7.500000000000012434 ) ) ;
#3480 = CARTESIAN_POINT ( 'NONE',  ( -106.6158994474202757, -286.8657778370662186, -240.0573691442952793 ) ) ;
#3481 = FACE_OUTER_BOUND ( 'NONE', #83950, .T. ) ;
#3482 = CARTESIAN_POINT ( 'NONE',  ( -110.7266578267132502, -288.7515249627732601, -254.8199309094176783 ) ) ;
#3483 = LINE ( 'NONE', #60333, #78480 ) ;
#3484 = CARTESIAN_POINT ( 'NONE',  ( -98.77153666896752782, -295.9018593688907686, -230.1007066985058316 ) ) ;
#3485 = CARTESIAN_POINT ( 'NONE',  ( -71.76624294165712570, -287.6516547220033999, -336.1464198544258579 ) ) ;
#3486 = CARTESIAN_POINT ( 'NONE',  ( 121.1498776811041438, 150.0802918209077177, -263.8330885344481658 ) ) ;
#3487 = CARTESIAN_POINT ( 'NONE',  ( -107.6726829452816219, -294.8918204399934098, -244.1623968445080095 ) ) ;
#3488 = CARTESIAN_POINT ( 'NONE',  ( 1.188457573889697860, -285.0366859289206900, -204.4813979563307385 ) ) ;
#3489 = CARTESIAN_POINT ( 'NONE',  ( 35.27625943179678103, -283.3248736587961503, -283.5877328220953473 ) ) ;
#3490 = CARTESIAN_POINT ( 'NONE',  ( 3.975652429553107048, -280.7441613301439247, -334.1951580907712582 ) ) ;
#3491 = CARTESIAN_POINT ( 'NONE',  ( -37.26801856798356027, -289.0512044463033021, -343.3610807978087678 ) ) ;
#3492 = AXIS2_PLACEMENT_3D ( 'NONE', #26890, #3717, #69980 ) ;
#3493 = CARTESIAN_POINT ( 'NONE',  ( 19.82113896954361465, -283.6280743775568567, -316.7251846059284617 ) ) ;
#3494 = CARTESIAN_POINT ( 'NONE',  ( 19.79572939634006090, -281.7108435265626554, -224.6673998703409154 ) ) ;
#3495 = CARTESIAN_POINT ( 'NONE',  ( 37.96200453370386896, -289.5825242995225040, -274.3110319910481962 ) ) ;
#3496 = CONICAL_SURFACE ( 'NONE', #53370, 4.000000000000003553, 1.029744258676654534 ) ;
#3497 = CARTESIAN_POINT ( 'NONE',  ( -82.97228390446436208, -297.6139512576797301, -208.2718905325717174 ) ) ;
#3498 = VERTEX_POINT ( 'NONE', #10746 ) ;
#3499 = CIRCLE ( 'NONE', #56446, 24.00000000000000355 ) ;
#3500 = CARTESIAN_POINT ( 'NONE',  ( -81.25038677240452500, -273.4736917697527474, -207.0428328662378306 ) ) ;
#3501 = CARTESIAN_POINT ( 'NONE',  ( -4.123262171867538406, -294.4721556704471368, -203.5009228801643530 ) ) ;
#3502 = CARTESIAN_POINT ( 'NONE',  ( 159.4851178187871312, 69.18068689461284748, -7.000000000000000888 ) ) ;
#3503 = CARTESIAN_POINT ( 'NONE',  ( -95.95921662488163406, -286.4090924074130839, -317.1477375740089997 ) ) ;
#3504 = ORIENTED_EDGE ( 'NONE', *, *, #8722, .F. ) ;
#3505 = CARTESIAN_POINT ( 'NONE',  ( 37.79886013720064142, -273.5266078969362411, -268.3800509541516703 ) ) ;
#3506 = CARTESIAN_POINT ( 'NONE',  ( 139.6925840978351516, -0.9999999999999991118, 22.50000000000000000 ) ) ;
#3507 = CARTESIAN_POINT ( 'NONE',  ( -112.8626095561200771, -294.8188545096006692, -280.8988274138584416 ) ) ;
#3508 = CARTESIAN_POINT ( 'NONE',  ( -62.05636646272959922, -273.0707073773173192, -201.5637493112703282 ) ) ;
#3509 = AXIS2_PLACEMENT_3D ( 'NONE', #17354, #44350, #80806 ) ;
#3510 = CARTESIAN_POINT ( 'NONE',  ( -91.27973232351980926, -292.7876233583033354, -220.1289463421949790 ) ) ;
#3511 = CARTESIAN_POINT ( 'NONE',  ( -59.22667057881314179, -285.0993336956092890, -341.1187548907683436 ) ) ;
#3512 = CARTESIAN_POINT ( 'NONE',  ( -112.2864870736867289, -291.7888547884392665, -285.3231724539863876 ) ) ;
#3513 = CARTESIAN_POINT ( 'NONE',  ( -104.1872876013020885, -292.3528703765999808, -233.1459905883267822 ) ) ;
#3514 = CARTESIAN_POINT ( 'NONE',  ( 28.39362824236933491, -293.8165028841322624, -302.2246007315227416 ) ) ;
#3515 = CARTESIAN_POINT ( 'NONE',  ( 7.048319744136891885, -290.4483194718962409, -330.8785390666133139 ) ) ;
#3516 = CARTESIAN_POINT ( 'NONE',  ( 22.87398460134540557, -281.0760973511481211, -222.3498315182758631 ) ) ;
#3517 = CARTESIAN_POINT ( 'NONE',  ( -112.3424223613341724, -294.7489488954487911, -261.1847427880285295 ) ) ;
#3518 = CARTESIAN_POINT ( 'NONE',  ( -27.37420368595265430, -282.7622862379806179, -346.7666173154133276 ) ) ;
#3519 = AXIS2_PLACEMENT_3D ( 'NONE', #17433, #18349, #3206 ) ;
#3520 = CARTESIAN_POINT ( 'NONE',  ( 28.22328208483245149, -278.0096016008662900, -306.1494825789188212 ) ) ;
#3521 = CARTESIAN_POINT ( 'NONE',  ( -9.685128554203979334, -274.8342426744605973, -340.8977717842163315 ) ) ;
#3522 = CARTESIAN_POINT ( 'NONE',  ( 175.2296996224750103, 250.5000000000000568, 0.000000000000000000 ) ) ;
#3523 = CARTESIAN_POINT ( 'NONE',  ( -92.60978701811066571, -283.3793437537340765, -318.1653762170193431 ) ) ;
#3524 = AXIS2_PLACEMENT_3D ( 'NONE', #39095, #830, #45739 ) ;
#3525 = CARTESIAN_POINT ( 'NONE',  ( -48.07838628637967560, -281.1236714209066463, -194.4607814239770107 ) ) ;
#3526 = CARTESIAN_POINT ( 'NONE',  ( 1.413272689442203855, -285.6154625031711021, -204.0821678239133803 ) ) ;
#3527 = CARTESIAN_POINT ( 'NONE',  ( 9.472692893479200293, -294.4657847708367058, -212.9676436195597091 ) ) ;
#3528 = CARTESIAN_POINT ( 'NONE',  ( 38.82475190748067462, -277.1980820771216258, -273.9853798329471601 ) ) ;
#3529 = CARTESIAN_POINT ( 'NONE',  ( 27.24158974425489887, -277.4094432712955722, -311.4754408556286194 ) ) ;
#3530 = CARTESIAN_POINT ( 'NONE',  ( -110.1685116794591721, -278.3100721470262329, -276.0767695804867117 ) ) ;
#3531 = CARTESIAN_POINT ( 'NONE',  ( -109.5372873558532802, -274.7792576125245319, -251.1983830590123148 ) ) ;
#3532 = CARTESIAN_POINT ( 'NONE',  ( -10.05841032550461733, -284.4089916781757097, -200.6647522803869492 ) ) ;
#3533 = CARTESIAN_POINT ( 'NONE',  ( 32.20909583356594652, -293.6431795383152803, -303.4767414905147689 ) ) ;
#3534 = CARTESIAN_POINT ( 'NONE',  ( -86.84904272021957183, -291.3273215102551035, -328.3567692955385837 ) ) ;
#3535 = VECTOR ( 'NONE', #44027, 1000.000000000000000 ) ;
#3536 = CARTESIAN_POINT ( 'NONE',  ( 29.02417964233303849, -292.0521722741974600, -239.0997151428993845 ) ) ;
#3537 = VERTEX_POINT ( 'NONE', #47665 ) ;
#3538 = CARTESIAN_POINT ( 'NONE',  ( -86.12280831207357323, -289.9660489227205744, -211.4790834090941303 ) ) ;
#3539 = CARTESIAN_POINT ( 'NONE',  ( 2.255529487390719012, -292.2650364333858874, -208.9485746055341622 ) ) ;
#3540 = VERTEX_POINT ( 'NONE', #91205 ) ;
#3541 = CARTESIAN_POINT ( 'NONE',  ( -95.21596241793501747, -290.9488912308358408, -320.6807192806642206 ) ) ;
#3542 = CARTESIAN_POINT ( 'NONE',  ( -110.0684122584599862, -279.3074120160384837, -262.4782581799385071 ) ) ;
#3543 = EDGE_CURVE ( 'NONE', #52528, #80622, #55017, .T. ) ;
#3544 = CARTESIAN_POINT ( 'NONE',  ( -98.83631042565870928, -296.0846984200247789, -224.5144804261545062 ) ) ;
#3545 = CARTESIAN_POINT ( 'NONE',  ( -52.16177603630362114, -286.5187603413301076, -194.8503335397373917 ) ) ;
#3546 = CARTESIAN_POINT ( 'NONE',  ( 27.11773386100906080, -287.3324524171187591, -228.2811267598260088 ) ) ;
#3547 = CARTESIAN_POINT ( 'NONE',  ( -97.37574256147604501, -285.4646735099198054, -228.7697798428477540 ) ) ;
#3548 = CARTESIAN_POINT ( 'NONE',  ( -31.54385115895311387, -124.1296239072845680, -364.1778657101864383 ) ) ;
#3549 = CARTESIAN_POINT ( 'NONE',  ( -110.5300065284289133, -264.7307192410654579, -306.1878980822340850 ) ) ;
#3550 = CARTESIAN_POINT ( 'NONE',  ( -31.03177537408224751, -124.7070154724701752, -360.4556306706562623 ) ) ;
#3551 = CARTESIAN_POINT ( 'NONE',  ( -94.58576116420519497, -277.1071319848362009, -315.9411938318368698 ) ) ;
#3552 = CARTESIAN_POINT ( 'NONE',  ( 21.07494522676942950, -275.0922978967715267, -314.6524446726106135 ) ) ;
#3553 = CARTESIAN_POINT ( 'NONE',  ( -60.12388022359375128, -297.2723495997484520, -196.8175532766127276 ) ) ;
#3554 = CARTESIAN_POINT ( 'NONE',  ( -97.02394130038283038, -247.4898175441587114, -331.8706397708260738 ) ) ;
#3555 = CARTESIAN_POINT ( 'NONE',  ( -84.57516265379381082, -276.3718005307977137, -330.6139778956907094 ) ) ;
#3556 = CARTESIAN_POINT ( 'NONE',  ( -38.11513081123835889, -275.8024718723389697, -196.3518224758765314 ) ) ;
#3557 = CARTESIAN_POINT ( 'NONE',  ( -105.1678373823866508, -290.6796861829718637, -297.6557278294694129 ) ) ;
#3558 = CARTESIAN_POINT ( 'NONE',  ( -111.4690222184587043, -297.6111311020603694, -249.9332731992617767 ) ) ;
#3559 = CARTESIAN_POINT ( 'NONE',  ( -89.57113311769904840, -297.8319755070070300, -213.7945775454860495 ) ) ;
#3560 = CARTESIAN_POINT ( 'NONE',  ( 17.97381884032833099, -294.3974273772245169, -318.0162292550816119 ) ) ;
#3561 = ORIENTED_EDGE ( 'NONE', *, *, #29697, .T. ) ;
#3562 = CONICAL_SURFACE ( 'NONE', #27780, 4.025000000000000355, 0.7853981633973095011 ) ;
#3563 = CARTESIAN_POINT ( 'NONE',  ( -56.53420651391186169, -279.2176532685523398, -343.4970207104573205 ) ) ;
#3564 = CARTESIAN_POINT ( 'NONE',  ( -30.22682948699986483, -282.4720686814482633, -346.9699002399244137 ) ) ;
#3565 = AXIS2_PLACEMENT_3D ( 'NONE', #71851, #6971, #36301 ) ;
#3566 = CARTESIAN_POINT ( 'NONE',  ( -40.50396707637281679, -278.0341096356804087, -343.5406132354212332 ) ) ;
#3567 = CARTESIAN_POINT ( 'NONE',  ( 36.26284111494198470, -277.5516729311813720, -289.2382344107984977 ) ) ;
#3568 = CARTESIAN_POINT ( 'NONE',  ( -60.68575216430463826, -296.3181406805940128, -200.5187549589553839 ) ) ;
#3569 = DIRECTION ( 'NONE',  ( 0.000000000000000000, 0.000000000000000000, 1.000000000000000000 ) ) ;
#3570 = CARTESIAN_POINT ( 'NONE',  ( -78.63025341943485103, -277.7918684300138352, -330.6244583185356873 ) ) ;
#3571 = AXIS2_PLACEMENT_3D ( 'NONE', #21542, #6412, #86869 ) ;
#3572 = CARTESIAN_POINT ( 'NONE',  ( -90.05952426016648360, -274.1329562602711007, -214.3868399119125456 ) ) ;
#3573 = CARTESIAN_POINT ( 'NONE',  ( 38.59892950167494519, -286.3592783143711245, -280.0772776289361445 ) ) ;
#3574 = CARTESIAN_POINT ( 'NONE',  ( -46.65846988999888367, -275.9340286228207333, -195.9420448328806401 ) ) ;
#3575 = CARTESIAN_POINT ( 'NONE',  ( 38.96705684354925125, -274.0655611780182994, -265.4955255711364543 ) ) ;
#3576 = CARTESIAN_POINT ( 'NONE',  ( 175.2296996224750103, 161.0000000000000853, 9.550761578869391144 ) ) ;
#3577 = AXIS2_PLACEMENT_3D ( 'NONE', #90895, #39781, #41669 ) ;
#3578 = CARTESIAN_POINT ( 'NONE',  ( -10.67475059123048631, -287.8925288928151076, -338.5438257208471100 ) ) ;
#3579 = AXIS2_PLACEMENT_3D ( 'NONE', #3184, #17412, #40540 ) ;
#3580 = CARTESIAN_POINT ( 'NONE',  ( -110.5909832594162765, -283.6055915651521104, -293.8108658896078964 ) ) ;
#3581 = CARTESIAN_POINT ( 'NONE',  ( 35.70002379452798635, -279.9475316401529312, -282.3143845139392170 ) ) ;
#3583 = CARTESIAN_POINT ( 'NONE',  ( -74.24874123376558543, -283.6373982981772883, -205.6997258425355426 ) ) ;
#3582 = CARTESIAN_POINT ( 'NONE',  ( 35.72256530037758893, -280.2471157571049503, -279.5496743247740028 ) ) ;
#3584 = CARTESIAN_POINT ( 'NONE',  ( 29.42458971303385340, -290.0054700535752659, -304.6389638658780541 ) ) ;
#3585 = CARTESIAN_POINT ( 'NONE',  ( -103.7355515119771781, -280.1791238356550480, -238.9528368796921995 ) ) ;
#3586 = DIRECTION ( 'NONE',  ( 0.000000000000000000, 1.000000000000000000, 0.000000000000000000 ) ) ;
#3587 = CARTESIAN_POINT ( 'NONE',  ( 27.18488080863017231, -279.4146534923528407, -229.7312065776307293 ) ) ;
#3588 = CARTESIAN_POINT ( 'NONE',  ( 5.336681734716932191, -294.6298804052118498, -208.6881387458344363 ) ) ;
#3590 = CARTESIAN_POINT ( 'NONE',  ( -90.33519128877667015, -277.5549640475629189, -215.8298763579868478 ) ) ;
#3589 = AXIS2_PLACEMENT_3D ( 'NONE', #35399, #72314, #92668 ) ;
#3591 = CARTESIAN_POINT ( 'NONE',  ( -43.20700921346766421, -277.7795873713844230, -343.2273709229162364 ) ) ;
#3592 = CARTESIAN_POINT ( 'NONE',  ( -41.44300898866784166, -285.1037115954483738, -345.4668974981497627 ) ) ;
#3593 = DIRECTION ( 'NONE',  ( 0.000000000000000000, -1.000000000000000000, 0.000000000000000000 ) ) ;
#3594 = CARTESIAN_POINT ( 'NONE',  ( -92.52410291393324826, -291.7542614080916223, -322.0525459733080993 ) ) ;
#3595 = AXIS2_PLACEMENT_3D ( 'NONE', #45296, #24471, #37283 ) ;
#3596 = EDGE_CURVE ( 'NONE', #45087, #74899, #45950, .T. ) ;
#3597 = CARTESIAN_POINT ( 'NONE',  ( -4.832952116147695598, -285.6666530723716733, -200.7382760127721895 ) ) ;
#3598 = CARTESIAN_POINT ( 'NONE',  ( -79.97644140347784969, -289.8648009274541550, -210.0596393592840911 ) ) ;
#3599 = CARTESIAN_POINT ( 'NONE',  ( -48.18343439339138001, -283.1093320178187582, -430.6442049081568371 ) ) ;
#3600 = CARTESIAN_POINT ( 'NONE',  ( 35.11465735488442874, -274.0748087476350179, -257.9850623104874217 ) ) ;
#3601 = CARTESIAN_POINT ( 'NONE',  ( -3.799391091954892552, -292.7444360309395393, -336.6005652980742866 ) ) ;
#3602 = LINE ( 'NONE', #11632, #79019 ) ;
#3603 = CARTESIAN_POINT ( 'NONE',  ( 140.6539576904058606, 250.5000000000000568, -12.50000000000000000 ) ) ;
#3604 = CARTESIAN_POINT ( 'NONE',  ( -14.05941338440898036, -290.8285501941077200, -197.6376102078408792 ) ) ;
#3605 = CARTESIAN_POINT ( 'NONE',  ( -110.8914037317769896, -286.0730426712937060, -276.4341331833798563 ) ) ;
#3606 = CARTESIAN_POINT ( 'NONE',  ( -75.17880751458058342, -287.7890861640981939, -336.2574556549772637 ) ) ;
#3607 = CARTESIAN_POINT ( 'NONE',  ( -38.65346954131330648, -287.4606941471247410, -196.7709972478338329 ) ) ;
#3608 = ADVANCED_FACE ( 'NONE', ( #11689 ), #80700, .F. ) ;
#3609 = DIRECTION ( 'NONE',  ( -0.000000000000000000, 1.000000000000000000, -0.000000000000000000 ) ) ;
#3610 = CARTESIAN_POINT ( 'NONE',  ( 22.09884203058636132, -288.9499373939734710, -313.0158208316170203 ) ) ;
#3611 = CARTESIAN_POINT ( 'NONE',  ( 34.70681222247446129, -295.2487667415485930, -248.2835576237800126 ) ) ;
#3612 = CARTESIAN_POINT ( 'NONE',  ( -100.8992325856211068, -276.0845769087823101, -311.3192643314317252 ) ) ;
#3613 = CARTESIAN_POINT ( 'NONE',  ( -67.69636223418849852, -277.7730056753987924, -341.1024692560662857 ) ) ;
#3614 = CARTESIAN_POINT ( 'NONE',  ( 26.84233109548847906, -291.0993841984039818, -230.3908562936944122 ) ) ;
#3615 = CARTESIAN_POINT ( 'NONE',  ( -113.7662432301547710, -278.4293597551597941, -280.1794997208239124 ) ) ;
#3616 = CARTESIAN_POINT ( 'NONE',  ( -96.61009421258725638, -299.1565390367795771, -224.9629286694865016 ) ) ;
#3617 = CARTESIAN_POINT ( 'NONE',  ( -48.18343439339133027, -264.4312075782656279, -496.1714326515607922 ) ) ;
#3618 = CARTESIAN_POINT ( 'NONE',  ( -110.3786324335668922, -282.3324557148184795, -287.4645182672546753 ) ) ;
#3619 = CARTESIAN_POINT ( 'NONE',  ( -48.18343439339134449, -254.0547856900766703, -480.4587914081814688 ) ) ;
#3620 = CARTESIAN_POINT ( 'NONE',  ( -109.6954169800915366, -276.4755713682384908, -287.0249116973764671 ) ) ;
#3621 = CARTESIAN_POINT ( 'NONE',  ( 36.88807596914821829, -279.6896477438029933, -281.0821715460117503 ) ) ;
#3622 = FACE_OUTER_BOUND ( 'NONE', #33584, .T. ) ;
#3623 = CARTESIAN_POINT ( 'NONE',  ( 19.34901374047956324, -274.7318770703203654, -321.4577720552351821 ) ) ;
#3624 = CARTESIAN_POINT ( 'NONE',  ( -110.4264030661165066, -298.2008373491525504, -260.5231914145043675 ) ) ;
#3625 = CARTESIAN_POINT ( 'NONE',  ( -76.61147981202276469, -282.4846526728620688, -336.2966422407261575 ) ) ;
#3626 = CARTESIAN_POINT ( 'NONE',  ( -70.58503270139516417, -298.5438992151777029, -205.0915916167130320 ) ) ;
#3627 = CARTESIAN_POINT ( 'NONE',  ( -110.3476246162948797, -298.1586358163755222, -247.3067130482227185 ) ) ;
#3628 = CARTESIAN_POINT ( 'NONE',  ( 5.192506653319919785, -274.3117287078989079, -210.9443556489674165 ) ) ;
#3629 = CARTESIAN_POINT ( 'NONE',  ( 3.303550686920755375, -294.5981021510733058, -207.2681548189215448 ) ) ;
#3630 = CARTESIAN_POINT ( 'NONE',  ( 27.13659901274048281, -287.1658781473803970, -228.2713455383054679 ) ) ;
#3631 = CARTESIAN_POINT ( 'NONE',  ( -3.301641916264301813, -274.7471367666977926, -338.0629276371942069 ) ) ;
#3632 = CARTESIAN_POINT ( 'NONE',  ( 25.85049158197741548, -287.9679283919724639, -314.4497864515938090 ) ) ;
#3633 = CARTESIAN_POINT ( 'NONE',  ( 23.73690771995800119, -286.0509875304440470, -229.8612124768762328 ) ) ;
#3634 = CARTESIAN_POINT ( 'NONE',  ( -108.5244133883725652, -288.8591520860207993, -246.5762767011976564 ) ) ;
#3635 = EDGE_LOOP ( 'NONE', ( #75934, #12803, #4384, #93641 ) ) ;
#3636 = CARTESIAN_POINT ( 'NONE',  ( 206.6943913402143096, 294.1769577359763161, -83.83314285352493300 ) ) ;
#3637 = AXIS2_PLACEMENT_3D ( 'NONE', #49476, #63245, #84503 ) ;
#3638 = CARTESIAN_POINT ( 'NONE',  ( -3.343318345540888803, -288.0984722136330447, -335.0862926492917495 ) ) ;
#3639 = CARTESIAN_POINT ( 'NONE',  ( 165.0427047786672290, 249.5000000000000568, 23.37680765314704701 ) ) ;
#3640 = CARTESIAN_POINT ( 'NONE',  ( -97.85153049825210303, -284.8602827561805384, -317.5986098996201008 ) ) ;
#3641 = CARTESIAN_POINT ( 'NONE',  ( 10.98000521840325838, -291.7606223035207904, -210.6451465341437483 ) ) ;
#3642 = CARTESIAN_POINT ( 'NONE',  ( 35.40583081042965574, -282.8643995261323312, -247.6843201971592805 ) ) ;
#3643 = CARTESIAN_POINT ( 'NONE',  ( -3.888463415681657320, -281.7993682370669717, -201.5413225496155576 ) ) ;
#3644 = CARTESIAN_POINT ( 'NONE',  ( -92.56052022569977566, -283.7049582715205815, -318.1282502806257071 ) ) ;
#3645 = CARTESIAN_POINT ( 'NONE',  ( 18.02432890966275636, -278.2588308072120640, -320.9728043955709040 ) ) ;
#3646 = CARTESIAN_POINT ( 'NONE',  ( -54.59516618233048746, -297.8363351003297339, -195.3190104087792918 ) ) ;
#3647 = TOROIDAL_SURFACE ( 'NONE', #65662, 24.50000000000000000, 0.5000000000000000000 ) ;
#3648 = CARTESIAN_POINT ( 'NONE',  ( -81.37981066230648253, -274.7545378001894960, -211.4594357926004307 ) ) ;
#3649 = CARTESIAN_POINT ( 'NONE',  ( 0.7700471852684900309, -290.5832673472678493, -206.1790214181901320 ) ) ;
#3650 = CARTESIAN_POINT ( 'NONE',  ( -37.81075464249324369, -296.9664671818636066, -197.0535054000108346 ) ) ;
#3651 = ORIENTED_EDGE ( 'NONE', *, *, #46092, .F. ) ;
#3652 = DIRECTION ( 'NONE',  ( 0.5729786897769825194, 1.137382224641321619E-14, 0.8195702660915978877 ) ) ;
#3653 = CARTESIAN_POINT ( 'NONE',  ( -108.7668310379991397, -286.1996917792465638, -291.3771489139386404 ) ) ;
#3654 = AXIS2_PLACEMENT_3D ( 'NONE', #5607, #71407, #86506 ) ;
#3655 = CARTESIAN_POINT ( 'NONE',  ( -32.02017785781833936, -296.0661944938649413, -346.8803577203190684 ) ) ;
#3656 = CIRCLE ( 'NONE', #39922, 8.500000000000007105 ) ;
#3657 = CARTESIAN_POINT ( 'NONE',  ( -109.0779264960525126, -285.0182938389965557, -284.4254876788514252 ) ) ;
#3658 = CARTESIAN_POINT ( 'NONE',  ( 27.44379568282640136, -275.1533809843029417, -311.6382920504752292 ) ) ;
#3659 = CARTESIAN_POINT ( 'NONE',  ( 20.29678017065466733, -293.5131461247013931, -219.4381975904448723 ) ) ;
#3660 = CARTESIAN_POINT ( 'NONE',  ( 30.32935644297891642, -285.2461718969747722, -236.2886425755122559 ) ) ;
#3661 = CARTESIAN_POINT ( 'NONE',  ( 4.126568248832680474, -292.9275303271610369, -205.4432764109110394 ) ) ;
#3662 = CARTESIAN_POINT ( 'NONE',  ( -96.57328127619301483, -290.2883733847293684, -313.0660039034881947 ) ) ;
#3663 = CARTESIAN_POINT ( 'NONE',  ( 169.9462594094670180, 250.5000000000000568, -23.92352941176469727 ) ) ;
#3664 = CIRCLE ( 'NONE', #23325, 2.500000000000000444 ) ;
#3665 = CARTESIAN_POINT ( 'NONE',  ( 222.4201966301864672, -44.14345022962302068, 22.50000000000000000 ) ) ;
#3666 = CARTESIAN_POINT ( 'NONE',  ( -62.22388460320987491, -183.0710032457758984, -358.7722912303554494 ) ) ;
#3667 = CARTESIAN_POINT ( 'NONE',  ( -57.59075369304125758, -287.3156083290446077, -196.7353183839019550 ) ) ;
#3668 = CARTESIAN_POINT ( 'NONE',  ( -95.95921662488163406, -294.6952119285919025, -223.5744983911110353 ) ) ;
#3669 = VERTEX_POINT ( 'NONE', #40082 ) ;
#3670 = ADVANCED_FACE ( 'NONE', ( #26373 ), #69455, .F. ) ;
#3671 = CARTESIAN_POINT ( 'NONE',  ( 16.04156061211757489, -281.1934707343594937, -320.6782800191246565 ) ) ;
#3672 = CARTESIAN_POINT ( 'NONE',  ( -112.9746097129493592, -278.3990453635024096, -255.9586054810243922 ) ) ;
#3673 = CARTESIAN_POINT ( 'NONE',  ( -13.75458084390644231, -282.3590026451987569, -199.2874991544501313 ) ) ;
#3674 = CARTESIAN_POINT ( 'NONE',  ( -68.72028664152445288, -197.1574858626671300, -358.6428543488109426 ) ) ;
#3675 = ADVANCED_FACE ( 'NONE', ( #53851 ), #61445, .T. ) ;
#3676 = CARTESIAN_POINT ( 'NONE',  ( 22.92688668245770245, -280.7594868724583534, -317.3535635459220998 ) ) ;
#3677 = CARTESIAN_POINT ( 'NONE',  ( 14.29518050955971908, -284.8017966785216117, -216.3872835249163415 ) ) ;
#3678 = CARTESIAN_POINT ( 'NONE',  ( -108.9424241297686535, -274.7299519248360866, -245.5893234993298506 ) ) ;
#3679 = AXIS2_PLACEMENT_3D ( 'NONE', #24712, #10485, #68270 ) ;
#3680 = CARTESIAN_POINT ( 'NONE',  ( -6.733421242427103159, -295.1314706440206805, -336.7020684243057076 ) ) ;
#3681 = ORIENTED_EDGE ( 'NONE', *, *, #203, .T. ) ;
#3682 = CARTESIAN_POINT ( 'NONE',  ( 0.1750993051216313823, -291.2478782896370717, -207.1651272999152980 ) ) ;
#3683 = CARTESIAN_POINT ( 'NONE',  ( 22.56681797367697584, -276.8507392544338472, -318.5927596699377773 ) ) ;
#3684 = CARTESIAN_POINT ( 'NONE',  ( -54.21153688493372869, -273.8293901800537924, -199.3371177587120542 ) ) ;
#3685 = CARTESIAN_POINT ( 'NONE',  ( 39.01095305913688804, -274.3753454015922557, -262.6252497561658288 ) ) ;
#3686 = CARTESIAN_POINT ( 'NONE',  ( 207.4345711710209343, 35.56792554197559042, 11.99999999999999822 ) ) ;
#3687 = CARTESIAN_POINT ( 'NONE',  ( -82.69117329601709798, -271.4326210128701291, -210.5603382261614058 ) ) ;
#3688 = CARTESIAN_POINT ( 'NONE',  ( -64.04315138647687888, -296.8190070920826429, -341.9546846855083118 ) ) ;
#3689 = CARTESIAN_POINT ( 'NONE',  ( 209.2568086740244837, 34.98978593258890868, 12.09245862095592727 ) ) ;
#3690 = CARTESIAN_POINT ( 'NONE',  ( 199.2296996224750103, 68.12454877777268791, 0.000000000000000000 ) ) ;
#3691 = CARTESIAN_POINT ( 'NONE',  ( -99.28489239726592075, -285.0911461414118548, -309.6641206029707405 ) ) ;
#3692 = CARTESIAN_POINT ( 'NONE',  ( 36.88063014320469080, -283.5193611751342360, -286.7007127241964213 ) ) ;
#3693 = CARTESIAN_POINT ( 'NONE',  ( -109.5204537167712289, -284.0543398857845432, -258.7008559994420125 ) ) ;
#3694 = CARTESIAN_POINT ( 'NONE',  ( -35.11367763140418674, -275.4235795490523060, -344.1274811344654267 ) ) ;
#3695 = CARTESIAN_POINT ( 'NONE',  ( -15.75100204404952109, -284.6302552625655835, -341.3872204692429477 ) ) ;
#3696 = CARTESIAN_POINT ( 'NONE',  ( -110.5954289105286250, -276.9210866731372107, -278.8506460073057838 ) ) ;
#3697 = CARTESIAN_POINT ( 'NONE',  ( 34.67459842992152375, -276.4517726080438820, -256.6542286077366271 ) ) ;
#3698 = CARTESIAN_POINT ( 'NONE',  ( 196.8803347170859865, 73.40565171261609123, -12.49999999999998579 ) ) ;
#3699 = CARTESIAN_POINT ( 'NONE',  ( -28.25426863066250505, -280.9673716393867835, -194.0083440244762301 ) ) ;
#3700 = ORIENTED_EDGE ( 'NONE', *, *, #46910, .T. ) ;
#3701 = ORIENTED_EDGE ( 'NONE', *, *, #20481, .F. ) ;
#3702 = CARTESIAN_POINT ( 'NONE',  ( 197.7570118961457695, 17.87787486654938363, 10.88803913700007975 ) ) ;
#3703 = CARTESIAN_POINT ( 'NONE',  ( -102.9823526865151138, -286.9136298341684324, -232.4201070035155396 ) ) ;
#3704 = CARTESIAN_POINT ( 'NONE',  ( -73.39085345530745030, -294.7406820238770138, -334.0247675129881486 ) ) ;
#3705 = CARTESIAN_POINT ( 'NONE',  ( -112.2161213889790474, -290.1202169613839601, -252.8358839466416441 ) ) ;
#3706 = CARTESIAN_POINT ( 'NONE',  ( 29.12812112663493025, -286.2269449983073173, -302.9147179869371485 ) ) ;
#3708 = CARTESIAN_POINT ( 'NONE',  ( -75.48285505297796760, -289.7761964459410251, -206.8723858681778438 ) ) ;
#3707 = CARTESIAN_POINT ( 'NONE',  ( 15.46485560699442985, -285.3918276152409135, -219.1083854862778821 ) ) ;
#3709 = CARTESIAN_POINT ( 'NONE',  ( -109.3661999113004981, -285.5718668317051652, -284.4891729368653728 ) ) ;
#3710 = CARTESIAN_POINT ( 'NONE',  ( 27.35743948046766505, -274.0589582028262612, -308.2955611787468229 ) ) ;
#3711 = CARTESIAN_POINT ( 'NONE',  ( 22.64493826663130349, -286.5869506597848044, -317.3719459951165049 ) ) ;
#3712 = CARTESIAN_POINT ( 'NONE',  ( -54.53160599625301330, -287.8314300863208359, -197.3576401074107025 ) ) ;
#3713 = CARTESIAN_POINT ( 'NONE',  ( 25.88847412566088479, -286.0993400144516272, -311.1015168225341085 ) ) ;
#3714 = CARTESIAN_POINT ( 'NONE',  ( 18.68207087875009620, -283.1614534672724517, -317.5477972199113310 ) ) ;
#3715 = CARTESIAN_POINT ( 'NONE',  ( 17.32929186436410163, -290.2739087983973718, -321.9470759671938254 ) ) ;
#3716 = SPHERICAL_SURFACE ( 'NONE', #83670, 1.000000000000000000 ) ;
#3717 = DIRECTION ( 'NONE',  ( -0.000000000000000000, -0.000000000000000000, -1.000000000000000000 ) ) ;
#3718 = CARTESIAN_POINT ( 'NONE',  ( -87.62850582987663017, -297.6675395369700823, -326.8276375493790624 ) ) ;
#3719 = CARTESIAN_POINT ( 'NONE',  ( -19.02203114442400178, -278.2876494383350519, -197.5791950613629240 ) ) ;
#3720 = CARTESIAN_POINT ( 'NONE',  ( -22.21554921374996283, -291.4381808060925891, -194.9719300890212708 ) ) ;
#3721 = CARTESIAN_POINT ( 'NONE',  ( -110.0607041098306240, -295.1162397386514158, -257.7759331969653545 ) ) ;
#3722 = CARTESIAN_POINT ( 'NONE',  ( 21.73531356265890579, -279.6279216616588315, -226.6232302346700749 ) ) ;
#3723 = CARTESIAN_POINT ( 'NONE',  ( 0.2006842507856418378, -272.6359761036351301, -206.0665076447548643 ) ) ;
#3724 = CARTESIAN_POINT ( 'NONE',  ( -75.90264450403937246, -296.8936097310100308, -332.9847849940167634 ) ) ;
#3725 = LINE ( 'NONE', #38757, #89716 ) ;
#3726 = CARTESIAN_POINT ( 'NONE',  ( -99.08015730504273222, -271.7300684382305462, -225.2515336869703049 ) ) ;
#3727 = CARTESIAN_POINT ( 'NONE',  ( 37.60307598746469893, -291.9519350583364599, -282.9799375716426084 ) ) ;
#3728 = VECTOR ( 'NONE', #17944, 999.9999999999998863 ) ;
#3729 = CARTESIAN_POINT ( 'NONE',  ( -30.77230205459084900, -293.5620974422297422, -197.0657025320491016 ) ) ;
#3730 = CARTESIAN_POINT ( 'NONE',  ( 201.2104617360081704, 60.19600395700749829, 7.000000000000000000 ) ) ;
#3731 = CARTESIAN_POINT ( 'NONE',  ( 14.98386275671792589, -293.6160892113402952, -219.1550446047386060 ) ) ;
#3732 = FACE_OUTER_BOUND ( 'NONE', #62620, .T. ) ;
#3734 = CARTESIAN_POINT ( 'NONE',  ( 20.52320543901548433, -294.1787170949178858, -314.8861090188129879 ) ) ;
#3733 = CARTESIAN_POINT ( 'NONE',  ( -27.61004275948390685, -280.9493661771480220, -345.1375085902362798 ) ) ;
#3735 = CARTESIAN_POINT ( 'NONE',  ( 32.39238987560119654, -281.9716586663358271, -303.1387913265050429 ) ) ;
#3736 = CARTESIAN_POINT ( 'NONE',  ( -106.9883179038249779, -283.7987696096448644, -303.1497276486421697 ) ) ;
#3737 = CARTESIAN_POINT ( 'NONE',  ( -99.81640266325914013, -289.1104353168295233, -229.0731080423128105 ) ) ;
#3738 = DIRECTION ( 'NONE',  ( -0.3024135303179394940, -0.9531768234072001134, 0.000000000000000000 ) ) ;
#3739 = CARTESIAN_POINT ( 'NONE',  ( 22.84401450027144875, -280.6646525542469135, -317.2905150132684753 ) ) ;
#3740 = CIRCLE ( 'NONE', #6802, 2.939656322713313230 ) ;
#3741 = EDGE_CURVE ( 'NONE', #25512, #71850, #23283, .T. ) ;
#3742 = CARTESIAN_POINT ( 'NONE',  ( -7.054705697281143273, -287.5843340915924955, -340.8323111664559519 ) ) ;
#3743 = CARTESIAN_POINT ( 'NONE',  ( -43.18343439339132317, -296.0521521680024080, -430.6442049081568939 ) ) ;
#3744 = CARTESIAN_POINT ( 'NONE',  ( -76.06061488172476004, -297.1785181648194225, -333.2481186419474852 ) ) ;
#3745 = CARTESIAN_POINT ( 'NONE',  ( 21.29025772054045973, -277.6418650265628685, -319.3600956610622461 ) ) ;
#3746 = CARTESIAN_POINT ( 'NONE',  ( -51.82740420475825260, -279.5285163502910564, -198.7394640599044067 ) ) ;
#3747 = CARTESIAN_POINT ( 'NONE',  ( 23.97394127447170931, -293.0979133398607246, -223.7626877676976846 ) ) ;
#3748 = CARTESIAN_POINT ( 'NONE',  ( -105.7132288800199262, -282.2121521082460163, -302.5270666125585990 ) ) ;
#3749 = CARTESIAN_POINT ( 'NONE',  ( -68.16940249262060547, -279.4571092204822094, -338.7465830200557093 ) ) ;
#3750 = CARTESIAN_POINT ( 'NONE',  ( 32.85805851504282771, -292.3335562041454523, -249.3199720749372261 ) ) ;
#3751 = CARTESIAN_POINT ( 'NONE',  ( -77.11957347515530614, -295.5188283455943292, -206.7787191624978504 ) ) ;
#3752 = VERTEX_POINT ( 'NONE', #70871 ) ;
#3753 = FACE_OUTER_BOUND ( 'NONE', #58377, .T. ) ;
#3754 = CARTESIAN_POINT ( 'NONE',  ( -23.51332835650195108, -294.3783842667656927, -342.1537197203543315 ) ) ;
#3755 = DIRECTION ( 'NONE',  ( -0.000000000000000000, -1.000000000000000000, -0.000000000000000000 ) ) ;
#3756 = CARTESIAN_POINT ( 'NONE',  ( -82.08285599513421005, -288.9094976428775681, -214.2051214447836571 ) ) ;
#3757 = CARTESIAN_POINT ( 'NONE',  ( -37.59482026529267529, -297.1078084665533652, -193.5968284698001298 ) ) ;
#3758 = CARTESIAN_POINT ( 'NONE',  ( -69.60026389723520879, -286.9515539124382713, -200.9733374609629379 ) ) ;
#3759 = CARTESIAN_POINT ( 'NONE',  ( -61.25701600895228438, -289.2048696744967060, -339.3325444634945711 ) ) ;
#3760 = CARTESIAN_POINT ( 'NONE',  ( -110.3111115768619470, -280.2115630193436004, -259.7023745579906517 ) ) ;
#3761 = CARTESIAN_POINT ( 'NONE',  ( -58.21168634846085865, -299.5388727493933061, -199.3511349760614735 ) ) ;
#3762 = CARTESIAN_POINT ( 'NONE',  ( -54.05920378112192992, -276.0663880267032937, -341.8814087185648987 ) ) ;
#3763 = ORIENTED_EDGE ( 'NONE', *, *, #45526, .T. ) ;
#3764 = CARTESIAN_POINT ( 'NONE',  ( -23.36033430842553571, -297.8894392957309947, -193.3830261749414774 ) ) ;
#3765 = CARTESIAN_POINT ( 'NONE',  ( -87.68560857433259059, -291.6815103985820201, -325.2653652623214384 ) ) ;
#3766 = CARTESIAN_POINT ( 'NONE',  ( 38.44370002599556102, -295.2587489999416448, -278.7859613990530647 ) ) ;
#3767 = CARTESIAN_POINT ( 'NONE',  ( -112.5627052039163516, -274.5519900738179331, -270.3865807095182276 ) ) ;
#3768 = CARTESIAN_POINT ( 'NONE',  ( -95.02588653217055992, -290.5715431880959159, -315.2859854738908325 ) ) ;
#3769 = CARTESIAN_POINT ( 'NONE',  ( -43.53109889459130954, -249.2085213603784268, -456.5866734977748251 ) ) ;
#3770 = CARTESIAN_POINT ( 'NONE',  ( 19.46847308635654983, -291.0017227332807579, -220.2125791070446894 ) ) ;
#3771 = CARTESIAN_POINT ( 'NONE',  ( -9.124202496769562742, -298.7296733842057392, -193.3807113113939522 ) ) ;
#3772 = CARTESIAN_POINT ( 'NONE',  ( -79.73687535343847799, -297.1277458130988975, -210.9074670912553984 ) ) ;
#3773 = DIRECTION ( 'NONE',  ( 0.000000000000000000, 0.000000000000000000, -1.000000000000000000 ) ) ;
#3774 = CARTESIAN_POINT ( 'NONE',  ( 195.0811277904325038, 27.48493576247232539, 15.19607843137263892 ) ) ;
#3775 = CARTESIAN_POINT ( 'NONE',  ( -112.4925842252274890, -292.2392415583480556, -257.1303820601103212 ) ) ;
#3776 = CARTESIAN_POINT ( 'NONE',  ( -99.86837403722181250, -292.4090924074130839, -320.2651865833026363 ) ) ;
#3777 = EDGE_CURVE ( 'NONE', #73850, #20929, #71819, .T. ) ;
#3778 = CARTESIAN_POINT ( 'NONE',  ( -109.5229372111426045, -286.2972642340722018, -290.1552565137893680 ) ) ;
#3779 = ADVANCED_FACE ( 'NONE', ( #26838 ), #85054, .T. ) ;
#3780 = CARTESIAN_POINT ( 'NONE',  ( -40.83566927194004847, -272.0080689501005509, -195.5584416224066615 ) ) ;
#3781 = CARTESIAN_POINT ( 'NONE',  ( -86.27480106415140426, -275.2875578507015462, -214.1954637909017549 ) ) ;
#3782 = CARTESIAN_POINT ( 'NONE',  ( 31.19085896907123612, -291.2478215303064530, -241.1670925712065809 ) ) ;
#3783 = CARTESIAN_POINT ( 'NONE',  ( -111.8465745835718366, -280.2367701674981504, -284.1919722268178816 ) ) ;
#3784 = VERTEX_POINT ( 'NONE', #64271 ) ;
#3785 = CARTESIAN_POINT ( 'NONE',  ( -48.35221062882412468, -282.5445874753498856, -342.6291007028255535 ) ) ;
#3786 = CARTESIAN_POINT ( 'NONE',  ( -111.0440035944138231, -279.8986946984858264, -249.1605761525999299 ) ) ;
#3787 = CARTESIAN_POINT ( 'NONE',  ( 23.44165430925463767, -279.7217804362036873, -223.7200259240646574 ) ) ;
#3788 = CIRCLE ( 'NONE', #23462, 0.5000000000000128786 ) ;
#3789 = CARTESIAN_POINT ( 'NONE',  ( 83.10068444444905822, 82.68374727650824241, -299.4140318971746524 ) ) ;
#3790 = CARTESIAN_POINT ( 'NONE',  ( 26.72756007566194825, -275.9356431648753869, -228.0769588946166380 ) ) ;
#3791 = APPLICATION_PROTOCOL_DEFINITION ( 'draft international standard', 'automotive_design', 1998, #57215 ) ;
#3792 = CARTESIAN_POINT ( 'NONE',  ( -49.62686765597128868, -275.4184753970764632, -194.9965585817814713 ) ) ;
#3793 = CARTESIAN_POINT ( 'NONE',  ( 7.450504543161046378, -278.9090924074131408, -326.4764044574609443 ) ) ;
#3794 = ORIENTED_EDGE ( 'NONE', *, *, #21048, .T. ) ;
#3795 = EDGE_LOOP ( 'NONE', ( #20981, #915 ) ) ;
#3796 = B_SPLINE_CURVE_WITH_KNOTS ( 'NONE', 3,
 ( #44129, #45509, #60232, #80131, #23763, #53094, #38882, #73034, #8163, #67791 ),
 .UNSPECIFIED., .F., .F.,
 ( 4, 2, 2, 2, 4 ),
 ( 0.5000000000000000000, 0.5447723136181439330, 0.5895446272362879769, 0.6343169408544320209, 0.6790892544725759539 ),
 .UNSPECIFIED. ) ;
#3797 = FACE_OUTER_BOUND ( 'NONE', #60628, .T. ) ;
#3798 = CARTESIAN_POINT ( 'NONE',  ( -88.86860724608207818, -290.8767907922493237, -322.5071045599775061 ) ) ;
#3799 = CARTESIAN_POINT ( 'NONE',  ( 21.29374681377383638, -288.6542313100443948, -222.0303991915291419 ) ) ;
#3800 = CARTESIAN_POINT ( 'NONE',  ( -105.2107677708636544, -289.5361099034072936, -297.6573221304121262 ) ) ;
#3801 = CARTESIAN_POINT ( 'NONE',  ( 24.65740365723694794, -286.4541666774916280, -224.8019473008992293 ) ) ;
#3802 = DIRECTION ( 'NONE',  ( 1.000000000000000000, -1.124465274301078034E-16, -0.000000000000000000 ) ) ;
#3803 = CARTESIAN_POINT ( 'NONE',  ( 19.96044163558106277, -280.6031639379269791, -316.8880732669632607 ) ) ;
#3804 = CARTESIAN_POINT ( 'NONE',  ( 33.00363917865989549, -289.1027651777063170, -246.6461708482359541 ) ) ;
#3805 = CARTESIAN_POINT ( 'NONE',  ( -18.57760694158791992, -281.2860604328961927, -341.6784285630788531 ) ) ;
#3806 = CARTESIAN_POINT ( 'NONE',  ( -104.9019450405615430, -280.2533242400683662, -241.4326409383732823 ) ) ;
#3807 = CARTESIAN_POINT ( 'NONE',  ( 34.62945368840601645, -288.1547741847199404, -243.6595593979861292 ) ) ;
#3808 = CARTESIAN_POINT ( 'NONE',  ( -92.76923378251689201, -278.3673619375146586, -317.9612960788221585 ) ) ;
#3809 = CARTESIAN_POINT ( 'NONE',  ( -112.5322414616984901, -289.5320085612436856, -255.6507507476649721 ) ) ;
#3810 = AXIS2_PLACEMENT_3D ( 'NONE', #50602, #62965, #14630 ) ;
#3811 = CARTESIAN_POINT ( 'NONE',  ( -113.4379889354556070, -285.2167501435198460, -281.3908560555238410 ) ) ;
#3812 = CARTESIAN_POINT ( 'NONE',  ( -1.004161295595429104, -287.0137118053792733, -202.5443783457734810 ) ) ;
#3813 = CARTESIAN_POINT ( 'NONE',  ( -33.49410224138745207, -283.1690883240081007, -343.2722227151212451 ) ) ;
#3814 = ORIENTED_EDGE ( 'NONE', *, *, #88682, .F. ) ;
#3815 = CARTESIAN_POINT ( 'NONE',  ( -97.38415354343349861, -293.0393986255323284, -224.1317913308921845 ) ) ;
#3816 = CARTESIAN_POINT ( 'NONE',  ( 26.09345564753667190, -291.6687573174892236, -227.4978217854600757 ) ) ;
#3817 = CARTESIAN_POINT ( 'NONE',  ( -36.72207634974510881, -273.1188707359617638, -197.1159888817449257 ) ) ;
#3818 = CARTESIAN_POINT ( 'NONE',  ( -111.4959257250324924, -295.6453885704456752, -290.7194974103967411 ) ) ;
#3819 = CARTESIAN_POINT ( 'NONE',  ( -92.17623646728226561, -289.7302232938142197, -221.1093197897206721 ) ) ;
#3820 = CARTESIAN_POINT ( 'NONE',  ( -8.861382141778378241, -292.9142792264262880, -338.6892246676347327 ) ) ;
#3821 = CARTESIAN_POINT ( 'NONE',  ( -86.98672413512964852, -290.9665472029911939, -324.4902227632713334 ) ) ;
#3822 = DIRECTION ( 'NONE',  ( 0.000000000000000000, 0.000000000000000000, 1.000000000000000000 ) ) ;
#3823 = CARTESIAN_POINT ( 'NONE',  ( 35.67293339134257479, -291.7814474073047109, -288.2724381629643631 ) ) ;
#3824 = CARTESIAN_POINT ( 'NONE',  ( 24.33859369159023345, -296.1311152283219030, -313.0511580319457039 ) ) ;
#3825 = CARTESIAN_POINT ( 'NONE',  ( 12.32414570359500061, -289.2817760311842221, -324.2511521285316576 ) ) ;
#3826 = CARTESIAN_POINT ( 'NONE',  ( 4.969041158637687694, -278.4632856510345391, -332.7166147122437678 ) ) ;
#3827 = CARTESIAN_POINT ( 'NONE',  ( -72.67127316535380999, -276.3043180960522136, -338.3450783578011283 ) ) ;
#3828 = CARTESIAN_POINT ( 'NONE',  ( -35.46651847218083731, -297.2722413285309813, -193.5228410401993244 ) ) ;
#3829 = CARTESIAN_POINT ( 'NONE',  ( 17.26383780331741846, -274.4991361181947696, -320.3420922601056304 ) ) ;
#3830 = CARTESIAN_POINT ( 'NONE',  ( -3.674848277866018087, -278.5797528103818195, -203.9552551387219239 ) ) ;
#3831 = CARTESIAN_POINT ( 'NONE',  ( 21.79203441000850461, -276.1513377228506556, -226.8831701784761776 ) ) ;
#3832 = CARTESIAN_POINT ( 'NONE',  ( -71.23353334215805432, -275.8919994566852552, -338.6090780963942848 ) ) ;
#3833 = CARTESIAN_POINT ( 'NONE',  ( 200.1126601882107252, 249.5000000000000568, -2.416251949619908856 ) ) ;
#3834 = CARTESIAN_POINT ( 'NONE',  ( -102.1246206068893940, -273.6651385091302018, -236.3830957407453184 ) ) ;
#3835 = LINE ( 'NONE', #27483, #38313 ) ;
#3837 = CARTESIAN_POINT ( 'NONE',  ( 33.83423658172637261, -275.1708802348304630, -254.0883783344873166 ) ) ;
#3836 = CARTESIAN_POINT ( 'NONE',  ( -62.24440673204787089, -287.3944031294223009, -341.5377645544289180 ) ) ;
#3838 = CARTESIAN_POINT ( 'NONE',  ( -12.22372873399449311, -288.7343269669929100, -343.2049522237026622 ) ) ;
#3839 = CARTESIAN_POINT ( 'NONE',  ( -30.69179918307676047, -300.1148906191218089, -195.0036787439324826 ) ) ;
#3840 = CARTESIAN_POINT ( 'NONE',  ( -108.4408398538581366, -294.8561388163880110, -246.8530472998392327 ) ) ;
#3841 = CARTESIAN_POINT ( 'NONE',  ( 31.88044968381650790, -280.3191656451151630, -236.8852224378985341 ) ) ;
#3842 = CARTESIAN_POINT ( 'NONE',  ( 221.8344101925596306, 0.000000000000000000, 10.00000000000000000 ) ) ;
#3843 = CARTESIAN_POINT ( 'NONE',  ( -4.125849016030076477, -278.4899119336675426, -203.1034748114884678 ) ) ;
#3844 = CARTESIAN_POINT ( 'NONE',  ( -48.18343439339133027, -253.0206516614774728, -465.6442049081569508 ) ) ;
#3845 = CARTESIAN_POINT ( 'NONE',  ( -108.4896135967199342, -289.5843662271626613, -252.2793800626216694 ) ) ;
#3846 = DIRECTION ( 'NONE',  ( -0.000000000000000000, -1.000000000000000000, -0.000000000000000000 ) ) ;
#3847 = LINE ( 'NONE', #47845, #14071 ) ;
#3848 = CARTESIAN_POINT ( 'NONE',  ( -104.1806912062201889, -289.0031135144143377, -236.2234462952982312 ) ) ;
#3849 = CARTESIAN_POINT ( 'NONE',  ( -54.39054924004955183, -275.3492675188937824, -198.6670143585344022 ) ) ;
#3850 = CARTESIAN_POINT ( 'NONE',  ( 27.81215116149938282, -283.5041391352590381, -310.3811201814481819 ) ) ;
#3852 = CARTESIAN_POINT ( 'NONE',  ( -93.42207030925594324, -283.8890286302528239, -317.0943190321610814 ) ) ;
#3851 = CARTESIAN_POINT ( 'NONE',  ( -111.6475788109127762, -270.8102793284238032, -256.3727456962960218 ) ) ;
#3853 = CARTESIAN_POINT ( 'NONE',  ( -46.26810626372915891, -275.3619658972887123, -197.3152817565799069 ) ) ;
#3854 = CARTESIAN_POINT ( 'NONE',  ( 9.580829515692020237, -275.5195125063872297, -214.1621018541664228 ) ) ;
#3855 = CARTESIAN_POINT ( 'NONE',  ( 22.67050588876224637, -284.1669401021530348, -315.3448459382437363 ) ) ;
#3856 = CARTESIAN_POINT ( 'NONE',  ( -76.71872781989530665, -272.4316568420984481, -208.5252403431800019 ) ) ;
#3857 = ORIENTED_EDGE ( 'NONE', *, *, #61840, .F. ) ;
#3858 = CARTESIAN_POINT ( 'NONE',  ( -186.9122233887894140, -89.54582641780471874, 21.50000000000000000 ) ) ;
#3859 = CARTESIAN_POINT ( 'NONE',  ( 19.52824766555975344, -294.0919391089947794, -322.3503284480491970 ) ) ;
#3860 = CARTESIAN_POINT ( 'NONE',  ( -107.7161797551716518, -286.2063611641913212, -295.4002116545882473 ) ) ;
#3861 = CARTESIAN_POINT ( 'NONE',  ( 175.2296996224750103, 276.0000000000000568, 0.000000000000000000 ) ) ;
#3862 = CARTESIAN_POINT ( 'NONE',  ( 15.93645355044460921, -281.4702648963637444, -320.5744003001203737 ) ) ;
#3863 = CARTESIAN_POINT ( 'NONE',  ( -119.3990491898856732, -282.0523547857346784, -270.3284710469131937 ) ) ;
#3864 = CARTESIAN_POINT ( 'NONE',  ( -106.2052141782906318, -277.3089545510403013, -304.5686183027536913 ) ) ;
#3865 = CARTESIAN_POINT ( 'NONE',  ( -111.5336455799082813, -289.1716553820066338, -252.9830959788331199 ) ) ;
#3866 = CARTESIAN_POINT ( 'NONE',  ( -2.080041497264457195, -284.0965032753784385, -335.0850740678901047 ) ) ;
#3867 = AXIS2_PLACEMENT_3D ( 'NONE', #30577, #37217, #59003 ) ;
#3868 = CARTESIAN_POINT ( 'NONE',  ( -87.76980426881645769, -279.5286494010926504, -324.5365766746646727 ) ) ;
#3869 = CARTESIAN_POINT ( 'NONE',  ( -29.54127319221524317, -287.5743836886140912, -194.3495423381301350 ) ) ;
#3870 = CARTESIAN_POINT ( 'NONE',  ( -49.49028958735146944, -281.8974109375523085, -196.3515752167647577 ) ) ;
#3871 = CARTESIAN_POINT ( 'NONE',  ( 1.193582804254908591, -274.7185470624626191, -203.6822600330811781 ) ) ;
#3872 = CARTESIAN_POINT ( 'NONE',  ( -107.5769756848989545, -277.9809490391822351, -302.0504314144416185 ) ) ;
#3873 = CARTESIAN_POINT ( 'NONE',  ( -101.3932908513521056, -297.9599835026583037, -308.3928622960517600 ) ) ;
#3874 = CARTESIAN_POINT ( 'NONE',  ( 156.8934089303672295, 249.5000000000000568, 16.24901362097164537 ) ) ;
#3875 = EDGE_CURVE ( 'NONE', #87519, #52231, #11143, .T. ) ;
#3876 = FACE_OUTER_BOUND ( 'NONE', #88544, .T. ) ;
#3877 = CARTESIAN_POINT ( 'NONE',  ( -110.0607289645893587, -271.0744741343257829, -248.1379112651184755 ) ) ;
#3878 = CARTESIAN_POINT ( 'NONE',  ( -96.93952468164245317, -277.4699290209426863, -312.6449797877878609 ) ) ;
#3879 = CARTESIAN_POINT ( 'NONE',  ( -46.84701685229932622, -275.1390719887108958, -194.3502130286888701 ) ) ;
#3880 = CARTESIAN_POINT ( 'NONE',  ( 7.523633233885763438, -288.4334962818484200, -211.4314836240222917 ) ) ;
#3881 = CARTESIAN_POINT ( 'NONE',  ( -111.6263444986069828, -297.8513360954940481, -287.8674849973318146 ) ) ;
#3882 = CARTESIAN_POINT ( 'NONE',  ( -97.08804772726796273, -297.1113003231642438, -318.3233230924677741 ) ) ;
#3883 = ADVANCED_FACE ( 'NONE', ( #48596 ), #13578, .F. ) ;
#3884 = CARTESIAN_POINT ( 'NONE',  ( -102.7379058268482623, -293.0387598460442860, -233.8765426218124617 ) ) ;
#3885 = CARTESIAN_POINT ( 'NONE',  ( -80.08159532274385128, -277.4719795939890901, -208.9336828837877249 ) ) ;
#3886 = CARTESIAN_POINT ( 'NONE',  ( -8.715753501634367240, -282.3498201072318921, -201.6452582478680711 ) ) ;
#3887 = CARTESIAN_POINT ( 'NONE',  ( -111.8282507846819698, -270.6444425313729312, -264.7655964034407248 ) ) ;
#3888 = CARTESIAN_POINT ( 'NONE',  ( -41.47762777424248526, -284.9639896214721944, -346.0644372150130152 ) ) ;
#3889 = CARTESIAN_POINT ( 'NONE',  ( -11.90187720279179651, -285.3115920806744725, -201.6076345574216191 ) ) ;
#3890 = CARTESIAN_POINT ( 'NONE',  ( 181.7315844963778204, 252.7314447161878661, -166.3319146787848410 ) ) ;
#3891 = ORIENTED_EDGE ( 'NONE', *, *, #55197, .F. ) ;
#3892 = CARTESIAN_POINT ( 'NONE',  ( 19.53433387065772564, -286.5713760049341090, -224.5460630323287887 ) ) ;
#3893 = VERTEX_POINT ( 'NONE', #34414 ) ;
#3894 = CARTESIAN_POINT ( 'NONE',  ( -78.98031843224808313, -284.6792455678940996, -334.7638972312655596 ) ) ;
#3895 = CARTESIAN_POINT ( 'NONE',  ( -109.1512911691190055, -273.0636955951828213, -256.8440481922058893 ) ) ;
#3896 = CARTESIAN_POINT ( 'NONE',  ( 38.16807301947188336, -286.1840028699430150, -257.3887898171809070 ) ) ;
#3897 = CARTESIAN_POINT ( 'NONE',  ( 37.10013944839366928, -282.2581906540859791, -251.6199137984777678 ) ) ;
#3898 = CYLINDRICAL_SURFACE ( 'NONE', #21924, 4.999999999999990230 ) ;
#3899 = CARTESIAN_POINT ( 'NONE',  ( -86.37415712152908043, -280.9062222552844901, -211.8240706576670789 ) ) ;
#3900 = CARTESIAN_POINT ( 'NONE',  ( 35.59041867844874929, -282.1976164632449127, -295.1570721854247950 ) ) ;
#3901 = CARTESIAN_POINT ( 'NONE',  ( 27.36219212280433055, -284.6237833571632905, -239.2376011013261916 ) ) ;
#3902 = CARTESIAN_POINT ( 'NONE',  ( 6.097804300016943735, -58.55705473465773281, -354.8591203811397463 ) ) ;
#3903 = ORIENTED_EDGE ( 'NONE', *, *, #12254, .T. ) ;
#3904 = CARTESIAN_POINT ( 'NONE',  ( 37.43522874238411902, -277.6041177106234272, -274.3864749951786166 ) ) ;
#3905 = CARTESIAN_POINT ( 'NONE',  ( 189.1269273087761746, 271.5004129489445859, -139.4852769914478756 ) ) ;
#3906 = CARTESIAN_POINT ( 'NONE',  ( 23.46775487827690654, -278.9808892367470889, -227.0707381497046811 ) ) ;
#3907 = CARTESIAN_POINT ( 'NONE',  ( 23.98321471386222470, -294.7086033295246352, -225.4920993278231549 ) ) ;
#3908 = CARTESIAN_POINT ( 'NONE',  ( -70.98508551709741710, -294.8569315755531193, -335.2751632507477666 ) ) ;
#3909 = CARTESIAN_POINT ( 'NONE',  ( -72.13882231151022495, -291.1120482898492696, -201.7266562873833777 ) ) ;
#3910 = CARTESIAN_POINT ( 'NONE',  ( 123.4306832106270946, -178.2391364535880882, 0.000000000000000000 ) ) ;
#3912 = CARTESIAN_POINT ( 'NONE',  ( 35.54615633446665157, -286.1040052329445871, -282.0087430885778303 ) ) ;
#3911 = CARTESIAN_POINT ( 'NONE',  ( -104.0970417118808768, -294.6399437678667255, -307.6490353800345474 ) ) ;
#3913 = CARTESIAN_POINT ( 'NONE',  ( 28.57260044242703145, -294.9558767396604253, -236.2118799550954407 ) ) ;
#3914 = CARTESIAN_POINT ( 'NONE',  ( -107.8327192305908824, -286.1426761573477506, -249.3936192887715606 ) ) ;
#3915 = VERTEX_POINT ( 'NONE', #33948 ) ;
#3916 = CARTESIAN_POINT ( 'NONE',  ( 36.85207186405477842, -294.2454271874594269, -250.6100683830450180 ) ) ;
#3917 = CARTESIAN_POINT ( 'NONE',  ( -107.8188564907485443, -284.7896946007451788, -289.6686294985610175 ) ) ;
#3918 = CARTESIAN_POINT ( 'NONE',  ( -112.7455393479568500, -295.5168014389322479, -256.8603865158926283 ) ) ;
#3919 = CARTESIAN_POINT ( 'NONE',  ( -112.7684182332622100, -291.5395922517828353, -255.6307074632259173 ) ) ;
#3920 = CARTESIAN_POINT ( 'NONE',  ( -84.23381177032861444, -291.9193052115301157, -209.2967807060013570 ) ) ;
#3921 = CARTESIAN_POINT ( 'NONE',  ( -21.12727545794537320, -289.0049481451823112, -341.5376059339846506 ) ) ;
#3922 = ORIENTED_EDGE ( 'NONE', *, *, #92370, .F. ) ;
#3923 = DIRECTION ( 'NONE',  ( 1.000000000000000000, 0.000000000000000000, 0.000000000000000000 ) ) ;
#3924 = CARTESIAN_POINT ( 'NONE',  ( -99.74693943026251475, -298.9892499639144603, -227.3744683607866079 ) ) ;
#3925 = CARTESIAN_POINT ( 'NONE',  ( -111.4302628277299334, -271.5943354071937392, -250.6930690799671879 ) ) ;
#3926 = CARTESIAN_POINT ( 'NONE',  ( 0.5318640914145956744, -279.6287387840284282, -207.6206613115326434 ) ) ;
#3927 = ORIENTED_EDGE ( 'NONE', *, *, #91947, .F. ) ;
#3928 = ORIENTED_EDGE ( 'NONE', *, *, #77906, .F. ) ;
#3929 = CARTESIAN_POINT ( 'NONE',  ( 38.67395804321970587, -275.2126909379657604, -282.5758344602695615 ) ) ;
#3930 = CARTESIAN_POINT ( 'NONE',  ( -70.76486760227054162, -296.0829234350040906, -204.6690761318453724 ) ) ;
#3931 = CARTESIAN_POINT ( 'NONE',  ( -3.279958271336609332, -278.4577381665240523, -336.3206754745209537 ) ) ;
#3932 = CARTESIAN_POINT ( 'NONE',  ( 16.35638309704997084, -272.9640199228561528, -219.0286924979402556 ) ) ;
#3933 = CARTESIAN_POINT ( 'NONE',  ( -93.05577821529237781, -298.4338955351863660, -222.5602783544774752 ) ) ;
#3934 = CARTESIAN_POINT ( 'NONE',  ( -86.31696427394523141, -298.4327590036571678, -215.8116030930952718 ) ) ;
#3935 = FACE_OUTER_BOUND ( 'NONE', #80868, .T. ) ;
#3936 = CARTESIAN_POINT ( 'NONE',  ( -113.5110041914985430, -298.1973691151788444, -266.7932724350081344 ) ) ;
#3937 = CARTESIAN_POINT ( 'NONE',  ( -109.4555446166864954, -270.8547586346160756, -248.3197336285120116 ) ) ;
#3938 = CARTESIAN_POINT ( 'NONE',  ( 3.880696444029271053, -295.1319988853880432, -330.7316959887211851 ) ) ;
#3939 = CARTESIAN_POINT ( 'NONE',  ( -44.33830144156664943, -290.5367903350182814, -197.0540205050876637 ) ) ;
#3940 = CARTESIAN_POINT ( 'NONE',  ( 209.8616357346614905, 36.89613957940296274, 10.50000000000000000 ) ) ;
#3941 = ADVANCED_FACE ( 'NONE', ( #41958 ), #17245, .T. ) ;
#3942 = CARTESIAN_POINT ( 'NONE',  ( 38.86236064766877263, -275.9117602386304497, -259.7560237114771553 ) ) ;
#3943 = CARTESIAN_POINT ( 'NONE',  ( -63.09089416710570930, -298.0407648374106202, -201.9770537296492705 ) ) ;
#3944 = CARTESIAN_POINT ( 'NONE',  ( 32.78430889520149805, -283.1730981371846951, -242.6371301171608650 ) ) ;
#3945 = TOROIDAL_SURFACE ( 'NONE', #55384, 24.00000000000000355, 1.000000000000000000 ) ;
#3946 = CARTESIAN_POINT ( 'NONE',  ( -44.39056898841063514, -281.8242437299555831, -346.5955736806773189 ) ) ;
#3947 = CARTESIAN_POINT ( 'NONE',  ( 0.9890151541174989624, -275.9035728178853333, -337.0853642246066784 ) ) ;
#3948 = CARTESIAN_POINT ( 'NONE',  ( 2.197429475817664013, -229.5268262511776527, 22.50000000000000000 ) ) ;
#3949 = CARTESIAN_POINT ( 'NONE',  ( -103.6274440919934534, -284.1679605102631285, -239.2765322247979043 ) ) ;
#3950 = CARTESIAN_POINT ( 'NONE',  ( -6.237961062326914607, -280.6442960687672326, -338.7905403553558585 ) ) ;
#3951 = CARTESIAN_POINT ( 'NONE',  ( 36.28808916097170822, -274.1432537918842627, -271.6129572846691644 ) ) ;
#3952 = CARTESIAN_POINT ( 'NONE',  ( -110.2397754343363090, -280.3252676258772453, -288.0462152943991896 ) ) ;
#3953 = CARTESIAN_POINT ( 'NONE',  ( -48.18343439339133027, -293.9810843561368756, -505.5731370962914752 ) ) ;
#3954 = CARTESIAN_POINT ( 'NONE',  ( 195.4113456599614551, 19.73462695515988230, 13.33559673734781015 ) ) ;
#3955 = CARTESIAN_POINT ( 'NONE',  ( -57.88612961976851068, -272.1911191981950537, -196.9280281509629447 ) ) ;
#3956 = CARTESIAN_POINT ( 'NONE',  ( -97.32466134903762622, -279.9340385015618153, -315.6820441345582822 ) ) ;
#3957 = DIRECTION ( 'NONE',  ( 0.000000000000000000, 0.000000000000000000, 1.000000000000000000 ) ) ;
#3958 = CARTESIAN_POINT ( 'NONE',  ( -105.3930203544997397, -286.9016394110923898, -237.5231519892752203 ) ) ;
#3959 = CARTESIAN_POINT ( 'NONE',  ( 156.4851178187871312, 15.24064981607392255, -6.999999999998999023 ) ) ;
#3960 = CARTESIAN_POINT ( 'NONE',  ( -32.59055472263807474, -286.9922305065118167, -345.2609619176300271 ) ) ;
#3961 = CARTESIAN_POINT ( 'NONE',  ( 155.8658096505380684, 20.95954935106544426, 14.18771993490441830 ) ) ;
#3962 = CARTESIAN_POINT ( 'NONE',  ( -107.2521678640016063, -295.0502972760867237, -292.8787700620900409 ) ) ;
#3963 = CARTESIAN_POINT ( 'NONE',  ( -15.51064158014850491, -286.9063134480295503, -341.3674231275247166 ) ) ;
#3964 = CARTESIAN_POINT ( 'NONE',  ( 156.8097460172999149, 17.78059845260639804, -7.900495735315244517 ) ) ;
#3965 = CARTESIAN_POINT ( 'NONE',  ( -109.5346917680343779, -294.2904637160274888, -290.6877657296118969 ) ) ;
#3966 = CARTESIAN_POINT ( 'NONE',  ( -66.90243596928769421, -284.1515985747753348, -200.0129079831128536 ) ) ;
#3967 = CARTESIAN_POINT ( 'NONE',  ( -2.792420425637325287, -282.1169338827938304, -205.1333854750963610 ) ) ;
#3968 = CARTESIAN_POINT ( 'NONE',  ( -83.28854091667598425, -281.9113829519091041, -330.9488113130627198 ) ) ;
#3969 = CARTESIAN_POINT ( 'NONE',  ( -74.71590172187745793, -289.5645964093313296, -333.0828143797020289 ) ) ;
#3970 = CARTESIAN_POINT ( 'NONE',  ( -109.7148629322869766, -280.1517723286212345, -257.0381969833500193 ) ) ;
#3971 = CARTESIAN_POINT ( 'NONE',  ( 20.63764013512398421, -281.7281467063703531, -225.7201619882444845 ) ) ;
#3972 = CARTESIAN_POINT ( 'NONE',  ( 37.99509383334434887, -289.5107615713391738, -268.6955023555037201 ) ) ;
#3973 = ORIENTED_EDGE ( 'NONE', *, *, #92308, .T. ) ;
#3974 = CARTESIAN_POINT ( 'NONE',  ( -78.84155419291386124, -273.5092632704380549, -205.5015611493715255 ) ) ;
#3975 = CARTESIAN_POINT ( 'NONE',  ( -111.9490725445499493, -292.4849238040270052, -274.0140372659323020 ) ) ;
#3976 = CARTESIAN_POINT ( 'NONE',  ( 157.4851178187871596, 1.000000000000001554, -8.171572875253810153 ) ) ;
#3977 = CARTESIAN_POINT ( 'NONE',  ( 40.65961533371913106, -296.2662352645559167, -288.1317622949166548 ) ) ;
#3978 = ORIENTED_EDGE ( 'NONE', *, *, #89850, .T. ) ;
#3979 = CARTESIAN_POINT ( 'NONE',  ( 36.15822021795626284, -273.3495455904300115, -254.5588239821648529 ) ) ;
#3980 = DIRECTION ( 'NONE',  ( 0.000000000000000000, 0.000000000000000000, -1.000000000000000000 ) ) ;
#3981 = CARTESIAN_POINT ( 'NONE',  ( -99.36929568534276314, -294.3585989404804195, -314.7108157338814749 ) ) ;
#3982 = CARTESIAN_POINT ( 'NONE',  ( -87.39706624112145050, -272.6804916913363854, -217.0156240571391777 ) ) ;
#3983 = CARTESIAN_POINT ( 'NONE',  ( 8.425533636345621247, -289.9324263097764742, -328.1198235085651618 ) ) ;
#3984 = CARTESIAN_POINT ( 'NONE',  ( -38.88402848578563464, -284.8318691571317345, -344.3710476100683309 ) ) ;
#3985 = CARTESIAN_POINT ( 'NONE',  ( -71.92196545920795359, -293.0293575898770086, -202.2084493069208122 ) ) ;
#3986 = CARTESIAN_POINT ( 'NONE',  ( -79.33780129512977908, -292.8135564267675477, -206.3475995486332693 ) ) ;
#3987 = CARTESIAN_POINT ( 'NONE',  ( 21.80595542779304452, -292.7866763501625655, -227.5548767595264223 ) ) ;
#3988 = CARTESIAN_POINT ( 'NONE',  ( -99.78598614260957333, -287.1135753174981460, -228.8194305723173443 ) ) ;
#3989 = CARTESIAN_POINT ( 'NONE',  ( -75.00978690769282764, -279.7313267816818438, -203.2037264096550189 ) ) ;
#3990 = CARTESIAN_POINT ( 'NONE',  ( -68.94827795070665388, -293.5443281292814959, -339.0071891260435564 ) ) ;
#3991 = CARTESIAN_POINT ( 'NONE',  ( -93.43299178725850140, -283.6652946230617545, -323.1323868274789106 ) ) ;
#3992 = CARTESIAN_POINT ( 'NONE',  ( 21.33061767708065304, -278.1688001777686168, -316.5271972907961526 ) ) ;
#3993 = EDGE_CURVE ( 'NONE', #34997, #58159, #35812, .T. ) ;
#3994 = CARTESIAN_POINT ( 'NONE',  ( 30.91033621190086578, -296.2662352645559167, -285.9065529553535612 ) ) ;
#3995 = CARTESIAN_POINT ( 'NONE',  ( -67.24328213961942424, -275.5796630498039690, -339.9757779007239265 ) ) ;
#3996 = DIRECTION ( 'NONE',  ( 0.000000000000000000, 1.000000000000000000, 0.000000000000000000 ) ) ;
#3997 = CARTESIAN_POINT ( 'NONE',  ( -1.227036590058407928, -282.0667193128870167, -333.8726879463029604 ) ) ;
#3998 = CARTESIAN_POINT ( 'NONE',  ( -64.61537948573912615, -280.9090724401610828, -198.7219689535120040 ) ) ;
#3999 = CARTESIAN_POINT ( 'NONE',  ( 32.64543012981248893, -287.0149876187390419, -301.8987432983395252 ) ) ;
#4000 = CARTESIAN_POINT ( 'NONE',  ( -33.47764100108386032, -293.8615673356368347, -196.4360509522435336 ) ) ;
#4001 = CARTESIAN_POINT ( 'NONE',  ( 32.29699949344013277, -277.5512180778191009, -301.2947878019139694 ) ) ;
#4002 = CARTESIAN_POINT ( 'NONE',  ( 37.73158758126069756, -276.6817748453760260, -255.6200275691118975 ) ) ;
#4003 = CARTESIAN_POINT ( 'NONE',  ( -35.11976253066777787, -276.8567960983031639, -343.3272950637256713 ) ) ;
#4004 = CARTESIAN_POINT ( 'NONE',  ( -61.12203803105138888, -299.7430216211606648, -199.3519198207216334 ) ) ;
#4005 = CARTESIAN_POINT ( 'NONE',  ( -112.1410887091962394, -282.5809905160034532, -268.1072565408044284 ) ) ;
#4006 = CARTESIAN_POINT ( 'NONE',  ( 23.96096623889392774, -292.5980329817888901, -223.7805658431922495 ) ) ;
#4007 = CARTESIAN_POINT ( 'NONE',  ( 21.79729763385790520, -289.8038797943099780, -318.4339171177215917 ) ) ;
#4008 = CARTESIAN_POINT ( 'NONE',  ( 35.51251759422262921, -292.5854358490628329, -278.9603921538848113 ) ) ;
#4009 = ORIENTED_EDGE ( 'NONE', *, *, #24867, .F. ) ;
#4010 = CARTESIAN_POINT ( 'NONE',  ( -50.44731205546880659, -290.4626793910574065, -195.0826401322508161 ) ) ;
#4011 = CARTESIAN_POINT ( 'NONE',  ( -32.15154794809505745, -291.7861051528240068, -197.5120346829365019 ) ) ;
#4012 = ORIENTED_EDGE ( 'NONE', *, *, #33617, .F. ) ;
#4013 = CARTESIAN_POINT ( 'NONE',  ( -65.32138313132958274, -290.4889601323397414, -341.8219205522011634 ) ) ;
#4014 = CARTESIAN_POINT ( 'NONE',  ( -109.2338518354734731, -279.3780383111872538, -257.1168289755672163 ) ) ;
#4015 = EDGE_CURVE ( 'NONE', #20911, #3498, #27308, .T. ) ;
#4016 = CARTESIAN_POINT ( 'NONE',  ( -112.0080249597404531, -295.2519638753410618, -287.9231737092022172 ) ) ;
#4017 = CARTESIAN_POINT ( 'NONE',  ( -29.48161483590419607, -286.8006493789483784, -193.8658119456694351 ) ) ;
#4018 = CARTESIAN_POINT ( 'NONE',  ( -18.19139214208549049, -286.6255765077052047, -195.7472626910281690 ) ) ;
#4019 = CARTESIAN_POINT ( 'NONE',  ( -100.4172623272052931, -284.3806398051031010, -307.1518904666638718 ) ) ;
#4020 = CARTESIAN_POINT ( 'NONE',  ( -84.28609762920955006, -219.3914707876369050, -352.4634555978751678 ) ) ;
#4021 = CARTESIAN_POINT ( 'NONE',  ( 159.5856148316313750, 220.3251242856082968, -204.2681947999263912 ) ) ;
#4022 = CARTESIAN_POINT ( 'NONE',  ( 152.6535939263449109, 205.0357462877106798, -214.3309654381289420 ) ) ;
#4023 = EDGE_CURVE ( 'NONE', #83547, #2308, #67130, .T. ) ;
#4024 = AXIS2_PLACEMENT_3D ( 'NONE', #80863, #24026, #15073 ) ;
#4025 = CARTESIAN_POINT ( 'NONE',  ( 19.13000027186423324, -274.0915920411455318, -223.8471546873101090 ) ) ;
#4026 = CARTESIAN_POINT ( 'NONE',  ( -13.69865890452786061, -275.6583918228139964, -339.8063541832243004 ) ) ;
#4027 = CARTESIAN_POINT ( 'NONE',  ( -40.43150215130466307, -297.5220758740396718, -193.4326384129933842 ) ) ;
#4028 = CARTESIAN_POINT ( 'NONE',  ( 161.8949478297373048, 217.5625359936354926, -202.7765268075980316 ) ) ;
#4029 = CARTESIAN_POINT ( 'NONE',  ( 37.69540036843609698, -274.4248344230874181, -285.2853205819436084 ) ) ;
#4030 = CARTESIAN_POINT ( 'NONE',  ( -90.94576330318855639, -275.0383167652792054, -219.3074990926179169 ) ) ;
#4031 = ORIENTED_EDGE ( 'NONE', *, *, #31052, .T. ) ;
#4032 = CARTESIAN_POINT ( 'NONE',  ( -100.9598543248765878, -274.1993811033202064, -227.4387219108742784 ) ) ;
#4033 =( BOUNDED_SURFACE ( )  B_SPLINE_SURFACE ( 3, 2, ( 
 ( #63343, #28274, #49106 ),
 ( #50023, #91708, #78916 ),
 ( #14064, #55748, #71839 ),
 ( #57616, #86459, #48618 ),
 ( #28732, #77518, #12670 ),
 ( #41513, #82972, #1586 ),
 ( #89597, #24286, #53161 ),
 ( #2982, #37557, #31409 ),
 ( #68320, #46061, #60298 ),
 ( #16720, #66469, #67403 ),
 ( #38498, #2060, #52691 ),
 ( #30468, #89135, #45115 ),
 ( #82043, #54100, #30950 ),
 ( #10079, #88216, #38011 ) ),
 .UNSPECIFIED., .F., .F., .F. ) 
 B_SPLINE_SURFACE_WITH_KNOTS ( ( 4, 2, 2, 2, 2, 2, 4 ),
 ( 3, 3 ),
 ( 5.128070023563283009, 5.416848844467358148, 5.705627665371434176, 5.850017075823472190, 5.994406486275510204, 6.138795896727548218, 6.283185307179586232 ),
 ( 0.000000000000000000, 1.000000000000000000 ),
 .UNSPECIFIED. ) 
 GEOMETRIC_REPRESENTATION_ITEM ( )  RATIONAL_B_SPLINE_SURFACE ( (
 ( 1.000000000000000000, 0.9583671019092238064, 1.000000000000000000),
 ( 1.000000000000000000, 0.9398658125638107430, 1.000000000000000000),
 ( 1.000000000000000000, 0.9157002655843566874, 1.000000000000000000),
 ( 1.000000000000000000, 0.8622678315323227816, 1.000000000000000000),
 ( 1.000000000000000000, 0.8329613673159231846, 1.000000000000000000),
 ( 1.000000000000000000, 0.7919708659745474666, 1.000000000000000000),
 ( 1.000000000000000000, 0.7788285231915077489, 1.000000000000000000),
 ( 1.000000000000000000, 0.7549177526733943377, 1.000000000000000000),
 ( 1.000000000000000000, 0.7441566529437989574, 1.000000000000000000),
 ( 1.000000000000000000, 0.7262859251462961963, 1.000000000000000000),
 ( 1.000000000000000000, 0.7191857644035900554, 1.000000000000000000),
 ( 1.000000000000000000, 0.7095926089624357003, 1.000000000000000000),
 ( 1.000000000000000000, 0.7070960980132859897, 1.000000000000000000),
 ( 1.000000000000000000, 0.7071067811865473507, 1.000000000000000000) ) ) 
 REPRESENTATION_ITEM ( '' )  SURFACE ( )  );
#4034 = CARTESIAN_POINT ( 'NONE',  ( -63.83736815365980988, -289.8994016073442594, -338.5032898712450447 ) ) ;
#4035 = CARTESIAN_POINT ( 'NONE',  ( -95.45266302553322646, -296.6744096911716042, -320.6331262177190524 ) ) ;
#4036 = CARTESIAN_POINT ( 'NONE',  ( -114.2764895211900580, -297.0539072336697473, -269.6093972280968956 ) ) ;
#4037 = CARTESIAN_POINT ( 'NONE',  ( -28.89387161511191238, -295.1088963941198813, -342.9216773273358285 ) ) ;
#4038 = VERTEX_POINT ( 'NONE', #78896 ) ;
#4039 = CARTESIAN_POINT ( 'NONE',  ( -92.27005585177633407, -279.7495852344541163, -322.3224873393675125 ) ) ;
#4040 = ORIENTED_EDGE ( 'NONE', *, *, #67853, .F. ) ;
#4041 = CARTESIAN_POINT ( 'NONE',  ( 35.27169297381365709, -280.7369771262673908, -244.7692610333076857 ) ) ;
#4042 = UNCERTAINTY_MEASURE_WITH_UNIT (LENGTH_MEASURE( 1.000000000000000082E-05 ), #53027, 'distance_accuracy_value', 'NONE');
#4043 = CARTESIAN_POINT ( 'NONE',  ( -11.15876004124781495, -277.6435906317606168, -338.7560161592641066 ) ) ;
#4044 = CARTESIAN_POINT ( 'NONE',  ( 36.92019660882584731, -277.5170706682662285, -286.5199641268273467 ) ) ;
#4045 = CARTESIAN_POINT ( 'NONE',  ( -112.4030575602510424, -276.6644657056460801, -263.1457901575126925 ) ) ;
#4046 = CARTESIAN_POINT ( 'NONE',  ( -43.49355164788299533, -274.4648378832227422, -197.5082821846793024 ) ) ;
#4047 = CARTESIAN_POINT ( 'NONE',  ( -98.40696098134409908, -271.6011207919544290, -229.0179435390359117 ) ) ;
#4048 = DIRECTION ( 'NONE',  ( 0.000000000000000000, 0.000000000000000000, 1.000000000000000000 ) ) ;
#4049 = CARTESIAN_POINT ( 'NONE',  ( -109.1324868316131642, -278.8933834816829744, -257.1292266207890975 ) ) ;
#4050 = CARTESIAN_POINT ( 'NONE',  ( 21.10140636523384217, -286.9064663761558336, -319.7342035411035681 ) ) ;
#4051 = CARTESIAN_POINT ( 'NONE',  ( 20.29705258445983773, -276.8896176567656653, -222.3738817825212948 ) ) ;
#4052 = DIRECTION ( 'NONE',  ( -0.000000000000000000, -1.000000000000000000, -0.000000000000000000 ) ) ;
#4053 = CARTESIAN_POINT ( 'NONE',  ( -50.79115954333742877, -288.4254054342342215, -342.3275407985929064 ) ) ;
#4054 = CARTESIAN_POINT ( 'NONE',  ( -108.1365484681044649, -283.5165483416020038, -300.5207354781006757 ) ) ;
#4055 = CARTESIAN_POINT ( 'NONE',  ( 35.56914304497294665, -279.6264126878859884, -257.6338652318328286 ) ) ;
#4057 = CARTESIAN_POINT ( 'NONE',  ( -100.8248340219891475, -283.1584755640865865, -231.3887262345100169 ) ) ;
#4056 = CARTESIAN_POINT ( 'NONE',  ( 20.14761920898719083, -279.4830995175145745, -224.4225385385279026 ) ) ;
#4058 = CARTESIAN_POINT ( 'NONE',  ( 36.50029055872439443, -289.7245242943254198, -283.7734164794053981 ) ) ;
#4059 = CARTESIAN_POINT ( 'NONE',  ( -109.1500874426143781, -279.5579548379943162, -285.5494693523274350 ) ) ;
#4060 = CARTESIAN_POINT ( 'NONE',  ( 153.2628468892384603, 20.37991841447901820, 11.93555113919330424 ) ) ;
#4061 = CARTESIAN_POINT ( 'NONE',  ( -76.15658909139186505, -293.5340424949073395, -206.1264115607340273 ) ) ;
#4062 = CARTESIAN_POINT ( 'NONE',  ( -66.94671055470398358, -277.9093002762613196, -200.3788532812752692 ) ) ;
#4063 = CARTESIAN_POINT ( 'NONE',  ( -70.49162088761256939, -278.1527132285085600, -335.5145938848217497 ) ) ;
#4064 = CARTESIAN_POINT ( 'NONE',  ( -75.79751954597993802, -285.5639878300248142, -335.0061147293567387 ) ) ;
#4065 = CARTESIAN_POINT ( 'NONE',  ( 199.0350682890975236, 66.35678781651726865, 8.036454959886293992 ) ) ;
#4066 = CARTESIAN_POINT ( 'NONE',  ( -97.00718836604771411, -291.8413187080085436, -316.7221330200372904 ) ) ;
#4067 = CARTESIAN_POINT ( 'NONE',  ( -111.8656736841943911, -294.6660120775948144, -261.4807654072386640 ) ) ;
#4068 = CARTESIAN_POINT ( 'NONE',  ( 18.24177169860236347, -286.0216536380135608, -217.2312243296136955 ) ) ;
#4069 = CARTESIAN_POINT ( 'NONE',  ( -101.8127393148392059, -289.4390505371529230, -234.3406728086626742 ) ) ;
#4070 = CARTESIAN_POINT ( 'NONE',  ( 10.19742947581766224, -229.5268262511776527, 22.47499999999998721 ) ) ;
#4071 = CARTESIAN_POINT ( 'NONE',  ( -6.081977584088528843, -275.3173350994387079, -336.8886847156738895 ) ) ;
#4072 = CARTESIAN_POINT ( 'NONE',  ( 11.07958883707165221, -292.5128886719675734, -326.6305079970456404 ) ) ;
#4073 = CARTESIAN_POINT ( 'NONE',  ( 189.4188515237862589, 293.9636489450775798, -40.00000000000000711 ) ) ;
#4074 = CARTESIAN_POINT ( 'NONE',  ( -94.18180535206808202, -289.7289409008695316, -219.4503117475313729 ) ) ;
#4075 = CARTESIAN_POINT ( 'NONE',  ( -49.57397602170458129, -287.4938622409321169, -197.5298536357526302 ) ) ;
#4076 = CARTESIAN_POINT ( 'NONE',  ( -72.72219355050258116, -287.7539575484923944, -337.6229474402345545 ) ) ;
#4077 = EDGE_CURVE ( 'NONE', #11917, #53167, #12642, .T. ) ;
#4078 = CARTESIAN_POINT ( 'NONE',  ( -60.17857700567269319, -287.1755000690762927, -200.4050462610182706 ) ) ;
#4079 = CARTESIAN_POINT ( 'NONE',  ( 73.43068321062709458, -134.2391364535880598, 0.000000000000000000 ) ) ;
#4080 = CARTESIAN_POINT ( 'NONE',  ( -68.85373024178605306, -286.4297520551655793, -204.3200775937451112 ) ) ;
#4081 = CARTESIAN_POINT ( 'NONE',  ( 37.79901751891349448, -295.4594404071306144, -264.6796259179565141 ) ) ;
#4082 = CARTESIAN_POINT ( 'NONE',  ( -70.95269423249102658, -275.5720255812921096, -338.0339727869271087 ) ) ;
#4083 = CARTESIAN_POINT ( 'NONE',  ( -1.473817414965842953, -276.9230220807195337, -338.4730793496436263 ) ) ;
#4084 = CARTESIAN_POINT ( 'NONE',  ( -39.15220980889361613, -290.1094812653827830, -194.8100163439370931 ) ) ;
#4085 = CARTESIAN_POINT ( 'NONE',  ( -84.56693291321538197, -279.4222895713034518, -209.4760689945764227 ) ) ;
#4086 = CARTESIAN_POINT ( 'NONE',  ( -93.40984197675048506, -297.8440626786731400, -319.6379916073888694 ) ) ;
#4087 = CARTESIAN_POINT ( 'NONE',  ( -48.18343439339133027, -276.2959221541308352, -501.8817130774843918 ) ) ;
#4088 = CARTESIAN_POINT ( 'NONE',  ( 161.2494399300530290, 8.542400036368780647, 9.000000000000001776 ) ) ;
#4089 = CARTESIAN_POINT ( 'NONE',  ( -94.57320003151176024, -276.0324729095927410, -317.6612810275421452 ) ) ;
#4090 = CARTESIAN_POINT ( 'NONE',  ( 22.99824609884386106, -278.9442864648622731, -225.8179755173599688 ) ) ;
#4091 = FACE_OUTER_BOUND ( 'NONE', #61074, .T. ) ;
#4092 = CARTESIAN_POINT ( 'NONE',  ( -1.608873715906876889, -272.9969432454428784, -202.9380294246406038 ) ) ;
#4093 = CARTESIAN_POINT ( 'NONE',  ( -99.30589279305291939, -297.5242994286335829, -310.3437424455297560 ) ) ;
#4094 = CARTESIAN_POINT ( 'NONE',  ( -55.64179531581449112, -282.2027015615037158, -344.8366107637288565 ) ) ;
#4095 = CARTESIAN_POINT ( 'NONE',  ( -63.17364631683722109, -298.6486375961428053, -201.7792268935036191 ) ) ;
#4096 = CARTESIAN_POINT ( 'NONE',  ( -113.6304927380235199, -297.9482890320134629, -263.9286994929665298 ) ) ;
#4097 = CARTESIAN_POINT ( 'NONE',  ( -68.28767609271420724, -273.3008831616714929, -204.2079119657149135 ) ) ;
#4098 = CARTESIAN_POINT ( 'NONE',  ( 26.53834025783352146, -295.0238672201796817, -230.9644721543005517 ) ) ;
#4099 = CARTESIAN_POINT ( 'NONE',  ( 24.14348973896150952, -288.3360602956159937, -316.7138032504097964 ) ) ;
#4100 = CARTESIAN_POINT ( 'NONE',  ( 33.02806802026004362, -274.0553942585200389, -298.5809362263261164 ) ) ;
#4101 = CARTESIAN_POINT ( 'NONE',  ( -26.14665468220148625, -288.7466964752044305, -346.5429462748469405 ) ) ;
#4102 = EDGE_CURVE ( 'NONE', #88194, #58673, #62613, .T. ) ;
#4103 = CARTESIAN_POINT ( 'NONE',  ( 32.89903587378962868, -286.3369763580445237, -249.5889153477106106 ) ) ;
#4104 = CARTESIAN_POINT ( 'NONE',  ( -111.1979718964696247, -288.7195278131462146, -257.3130617650502359 ) ) ;
#4105 = ORIENTED_EDGE ( 'NONE', *, *, #42456, .T. ) ;
#4106 = CARTESIAN_POINT ( 'NONE',  ( -68.16629546550866792, -198.4621125041185792, -363.1570911012638021 ) ) ;
#4107 = CARTESIAN_POINT ( 'NONE',  ( 27.08177225225482232, -287.5304661620513684, -304.9304168731330833 ) ) ;
#4108 = FACE_OUTER_BOUND ( 'NONE', #54869, .T. ) ;
#4109 = CARTESIAN_POINT ( 'NONE',  ( -113.9180873375829890, -285.5697025661181101, -264.2788542957584355 ) ) ;
#4110 = CARTESIAN_POINT ( 'NONE',  ( 36.48119578051298362, -292.3457168723773520, -249.2656232489793808 ) ) ;
#4111 = CARTESIAN_POINT ( 'NONE',  ( 3.377078620101252149, -282.1894655818741171, -205.8905600691232678 ) ) ;
#4112 = CARTESIAN_POINT ( 'NONE',  ( 36.12146946061618991, -282.5971331870076142, -248.9492403676707113 ) ) ;
#4113 = CARTESIAN_POINT ( 'NONE',  ( -64.05734815539319982, -283.2439246382484725, -338.2969270598796356 ) ) ;
#4114 = CARTESIAN_POINT ( 'NONE',  ( 33.15005505654980311, -277.8861981994871257, -296.1229791198512089 ) ) ;
#4115 = CARTESIAN_POINT ( 'NONE',  ( -107.1663718575286310, -296.1367403650606320, -302.8190171424707273 ) ) ;
#4116 = CARTESIAN_POINT ( 'NONE',  ( -3.895108466936783032, -275.8180782213758562, -204.9056516308431810 ) ) ;
#4117 = CARTESIAN_POINT ( 'NONE',  ( -94.68762819549425558, -289.2355056356366845, -222.5573747271971285 ) ) ;
#4118 = CARTESIAN_POINT ( 'NONE',  ( -37.13499189490923413, -296.9751344645247286, -197.0491815705110525 ) ) ;
#4119 = ORIENTED_EDGE ( 'NONE', *, *, #18958, .F. ) ;
#4120 = DIRECTION ( 'NONE',  ( -0.000000000000000000, -0.000000000000000000, -1.000000000000000000 ) ) ;
#4121 = CARTESIAN_POINT ( 'NONE',  ( -105.4205781120815146, -286.0749260667905105, -300.4705943560637706 ) ) ;
#4122 = CARTESIAN_POINT ( 'NONE',  ( -37.67378505188158044, -296.1358488637872028, -347.0643144774864481 ) ) ;
#4123 = CARTESIAN_POINT ( 'NONE',  ( -107.4873929206173671, -284.9311557883818864, -290.9842884770891942 ) ) ;
#4124 = EDGE_CURVE ( 'NONE', #29329, #86133, #42429, .T. ) ;
#4125 = CARTESIAN_POINT ( 'NONE',  ( -35.72850811834609885, -276.0911642997310196, -347.1219561182802522 ) ) ;
#4126 = CARTESIAN_POINT ( 'NONE',  ( -112.2199138107177276, -291.4228324734360172, -252.8520945127737320 ) ) ;
#4127 = CARTESIAN_POINT ( 'NONE',  ( -110.6853137216536851, -282.4494680301459084, -289.4131381243500982 ) ) ;
#4128 = CARTESIAN_POINT ( 'NONE',  ( -73.42755987748770963, -291.9201075764639768, -202.3494939518758713 ) ) ;
#4129 = CARTESIAN_POINT ( 'NONE',  ( -31.86553411512128164, -289.3145719985016058, -343.2272700366625600 ) ) ;
#4130 = CARTESIAN_POINT ( 'NONE',  ( 196.8934835002044395, 70.76361186333477349, 10.57047112608304928 ) ) ;
#4131 = DIRECTION ( 'NONE',  ( 0.000000000000000000, 0.000000000000000000, 1.000000000000000000 ) ) ;
#4132 = CARTESIAN_POINT ( 'NONE',  ( 179.7466012574299725, 251.0770343007640690, -164.2655899362252683 ) ) ;
#4133 = CARTESIAN_POINT ( 'NONE',  ( 8.805032570909716583, -283.9522771636744665, -331.1327134209747101 ) ) ;
#4134 = CARTESIAN_POINT ( 'NONE',  ( 21.27581636871891391, -279.6952119285918457, -317.1477375740089997 ) ) ;
#4135 = ORIENTED_EDGE ( 'NONE', *, *, #16496, .F. ) ;
#4136 = CARTESIAN_POINT ( 'NONE',  ( 33.03517741311532774, -280.2020894803011402, -249.8350082299948838 ) ) ;
#4137 = CARTESIAN_POINT ( 'NONE',  ( -37.13128573027449164, -276.7162712372314672, -347.3527415445742577 ) ) ;
#4138 = CARTESIAN_POINT ( 'NONE',  ( -108.9895957406937157, -280.8312899120113002, -248.7600188987238425 ) ) ;
#4139 = CARTESIAN_POINT ( 'NONE',  ( 186.7585022445316838, 260.8546661130829989, -152.0293674503833472 ) ) ;
#4140 = CARTESIAN_POINT ( 'NONE',  ( 3.522310748714557516, -279.1645524513189685, -205.7328376492112056 ) ) ;
#4141 = CARTESIAN_POINT ( 'NONE',  ( -107.7330614769566210, -282.2472148643521450, -295.3527209834237510 ) ) ;
#4142 = CARTESIAN_POINT ( 'NONE',  ( -106.9521679608413649, -274.8013060087374129, -240.3170026231693726 ) ) ;
#4143 = CARTESIAN_POINT ( 'NONE',  ( -93.98628086929754488, -296.3916493914846910, -316.5259833511778993 ) ) ;
#4144 = EDGE_LOOP ( 'NONE', ( #46379, #25207, #12148, #83850 ) ) ;
#4145 = CARTESIAN_POINT ( 'NONE',  ( -2.188920048612625902, -291.2125573395861693, -205.8059427533700898 ) ) ;
#4146 = CARTESIAN_POINT ( 'NONE',  ( -31.44978770529064604, -277.6311453919358314, -347.0856882651813180 ) ) ;
#4147 = CARTESIAN_POINT ( 'NONE',  ( -2.913658196528595923, -274.5206400460447753, -205.9894632830011290 ) ) ;
#4148 = CARTESIAN_POINT ( 'NONE',  ( 39.24651482946023862, -274.4111064346867010, -265.4732363449367654 ) ) ;
#4149 = FACE_OUTER_BOUND ( 'NONE', #63894, .T. ) ;
#4150 = CARTESIAN_POINT ( 'NONE',  ( -37.62384662711495764, -272.0484977391615757, -195.3490580416540752 ) ) ;
#4151 = EDGE_CURVE ( 'NONE', #60845, #54318, #30836, .T. ) ;
#4152 = CARTESIAN_POINT ( 'NONE',  ( 219.8344101925596021, 0.000000000000000000, 7.000000000000000000 ) ) ;
#4153 = CARTESIAN_POINT ( 'NONE',  ( 198.9506515269346210, 68.58287003104832991, 4.213754548330891581 ) ) ;
#4154 = CARTESIAN_POINT ( 'NONE',  ( 34.53647105710715692, -282.8219959130820484, -284.8380436314721464 ) ) ;
#4155 = CARTESIAN_POINT ( 'NONE',  ( 37.15655596374822522, -283.5019555704919298, -285.3272081728183593 ) ) ;
#4156 = CARTESIAN_POINT ( 'NONE',  ( -98.18731870919012295, -284.4624293883412633, -229.8431791444158137 ) ) ;
#4157 = CARTESIAN_POINT ( 'NONE',  ( -24.20702140016851089, -275.2816531584898030, -343.0348947746628028 ) ) ;
#4158 = CARTESIAN_POINT ( 'NONE',  ( -65.76711976480913791, -285.2883568993897256, -338.9523532805414447 ) ) ;
#4159 = CARTESIAN_POINT ( 'NONE',  ( -107.7850624035687019, -276.7460210517311339, -292.1756294858532783 ) ) ;
#4160 = CARTESIAN_POINT ( 'NONE',  ( -0.4023431909508938253, -275.6353175274970795, -207.0241959188328451 ) ) ;
#4161 = DIRECTION ( 'NONE',  ( 0.000000000000000000, 0.000000000000000000, 1.000000000000000000 ) ) ;
#4162 = CARTESIAN_POINT ( 'NONE',  ( -86.70881855613100697, -280.1890482956134178, -211.4101285665891794 ) ) ;
#4163 = ORIENTED_EDGE ( 'NONE', *, *, #48459, .F. ) ;
#4164 = CARTESIAN_POINT ( 'NONE',  ( 200.6868442215911728, 15.43634792868212635, 10.00000000000000178 ) ) ;
#4165 = CARTESIAN_POINT ( 'NONE',  ( -33.80900922685039234, -287.9565731022641444, -194.6787185946306238 ) ) ;
#4166 = CARTESIAN_POINT ( 'NONE',  ( -15.55446817405715620, -293.9601632847988526, -340.2564994466360986 ) ) ;
#4167 = CARTESIAN_POINT ( 'NONE',  ( -105.9094572422793590, -290.3508329957741694, -235.4331688118980708 ) ) ;
#4168 = CARTESIAN_POINT ( 'NONE',  ( 28.57063116371966416, -285.3395244654289513, -236.5799861972809026 ) ) ;
#4170 = CARTESIAN_POINT ( 'NONE',  ( -110.1801013938541587, -288.6211012695011391, -283.4966163001510608 ) ) ;
#4169 = CARTESIAN_POINT ( 'NONE',  ( -8.003490661816455187, -285.0189374764179888, -202.8730124851904293 ) ) ;
#4171 = CARTESIAN_POINT ( 'NONE',  ( -59.05101491641170242, -284.5443575837082903, -340.5275692681016722 ) ) ;
#4172 = CARTESIAN_POINT ( 'NONE',  ( 36.52684549812997972, -273.3844072228177993, -257.3092040343902909 ) ) ;
#4173 = CARTESIAN_POINT ( 'NONE',  ( -18.36138724680209933, -284.6924780804628767, -196.5082907733637398 ) ) ;
#4174 = CARTESIAN_POINT ( 'NONE',  ( -92.21726406034277090, -299.2684638619484758, -219.1612401178895766 ) ) ;
#4175 = CARTESIAN_POINT ( 'NONE',  ( 20.69137334903584957, -284.8945380587588261, -222.5888371770631124 ) ) ;
#4176 = CARTESIAN_POINT ( 'NONE',  ( -38.36916137511170177, -280.9802185442484301, -197.1205897335820225 ) ) ;
#4177 = CARTESIAN_POINT ( 'NONE',  ( -77.14350140077200990, -291.5840230152290360, -334.1858022588729114 ) ) ;
#4178 = DIRECTION ( 'NONE',  ( -0.000000000000000000, -1.000000000000000000, -0.000000000000000000 ) ) ;
#4179 = FACE_BOUND ( 'NONE', #64618, .T. ) ;
#4180 = CARTESIAN_POINT ( 'NONE',  ( -32.08776164674274156, -296.9065414848801652, -345.7512453865664384 ) ) ;
#4181 = CARTESIAN_POINT ( 'NONE',  ( -38.35599340309022409, -278.0392828225816402, -195.3552326248492079 ) ) ;
#4182 = CARTESIAN_POINT ( 'NONE',  ( 11.02509503695413784, -291.8990194406365504, -210.5866092699514525 ) ) ;
#4183 = CARTESIAN_POINT ( 'NONE',  ( -109.5577762349642796, -295.1512399430864093, -255.0925855094758390 ) ) ;
#4184 = CARTESIAN_POINT ( 'NONE',  ( 35.62734420842953398, -280.3571962879857438, -279.5363100645913619 ) ) ;
#4185 = CARTESIAN_POINT ( 'NONE',  ( -29.82052890166939818, -272.2279485180540064, -196.3020457450574270 ) ) ;
#4186 = CARTESIAN_POINT ( 'NONE',  ( 10.62596837776658809, -295.6879674950345134, -326.0418709839166240 ) ) ;
#4187 = CARTESIAN_POINT ( 'NONE',  ( -85.33152481854862970, -293.9090924074130839, -210.2361428286348826 ) ) ;
#4188 = CARTESIAN_POINT ( 'NONE',  ( -99.34676823814790225, -295.6267883916999040, -225.8855147573280249 ) ) ;
#4189 = CARTESIAN_POINT ( 'NONE',  ( 38.22099402024237236, -291.6842995323007131, -261.8618256588219424 ) ) ;
#4190 = CARTESIAN_POINT ( 'NONE',  ( -9.521413983935405057, -293.8481037876265987, -202.1790362693750467 ) ) ;
#4191 = CARTESIAN_POINT ( 'NONE',  ( 157.4851178187871312, 15.00000000000000000, -7.000000000000000888 ) ) ;
#4192 = CARTESIAN_POINT ( 'NONE',  ( -77.35199403553258435, -292.3030660243553029, -209.1093579413192458 ) ) ;
#4193 = FACE_OUTER_BOUND ( 'NONE', #12147, .T. ) ;
#4195 = CARTESIAN_POINT ( 'NONE',  ( -77.94974150490634202, -295.6143802988760285, -331.0850701778412599 ) ) ;
#4194 = CARTESIAN_POINT ( 'NONE',  ( -34.56536661339670502, -281.0375271304656621, -345.6651602215052890 ) ) ;
#4196 = CARTESIAN_POINT ( 'NONE',  ( -65.25218816925747944, -283.4069928950823396, -342.1388546935320392 ) ) ;
#4197 = CARTESIAN_POINT ( 'NONE',  ( -52.91748554546068561, -282.9131172425765612, -345.8021939631918258 ) ) ;
#4198 = CARTESIAN_POINT ( 'NONE',  ( 2.260736105578529109, -286.5201396416985062, -333.8565939625161150 ) ) ;
#4199 = CARTESIAN_POINT ( 'NONE',  ( 164.6329196456214277, 275.5000000000000568, 23.09031830825856346 ) ) ;
#4200 = CARTESIAN_POINT ( 'NONE',  ( 27.70377035048882419, -280.5592194406066255, -310.3585126206784253 ) ) ;
#4201 = CARTESIAN_POINT ( 'NONE',  ( 38.36756507663325522, -286.6301174334181496, -282.9147199469671818 ) ) ;
#4202 = CARTESIAN_POINT ( 'NONE',  ( 223.4306832106270804, -141.7221692137691775, 21.50000000000000000 ) ) ;
#4203 = CARTESIAN_POINT ( 'NONE',  ( 33.39002088987867012, -294.8745263657532973, -249.1266023085734957 ) ) ;
#4204 = CARTESIAN_POINT ( 'NONE',  ( 16.55260188110149144, -277.7297356807420670, -324.6015270113794031 ) ) ;
#4205 = CARTESIAN_POINT ( 'NONE',  ( -24.86860773075179054, -279.8823871677609532, -198.4131544760020063 ) ) ;
#4206 = CARTESIAN_POINT ( 'NONE',  ( -39.21381946646181405, -292.1959778550440774, -193.3708447783596114 ) ) ;
#4207 = CARTESIAN_POINT ( 'NONE',  ( -22.04190996844411998, -280.9374547131282611, -344.3559192611696744 ) ) ;
#4208 = CARTESIAN_POINT ( 'NONE',  ( 30.80010111909687964, -292.9702563063384559, -297.3345522005225803 ) ) ;
#4209 = CARTESIAN_POINT ( 'NONE',  ( -112.2382565473547658, -294.4900537429583096, -275.1846851534240272 ) ) ;
#4210 = VERTEX_POINT ( 'NONE', #41488 ) ;
#4211 = CARTESIAN_POINT ( 'NONE',  ( 9.339199855150265961, -212.1443419142231051, 25.50000000000000000 ) ) ;
#4212 = CARTESIAN_POINT ( 'NONE',  ( -31.60377231116232011, -294.4855549584206642, -343.2471480796669994 ) ) ;
#4213 = CARTESIAN_POINT ( 'NONE',  ( 207.5109667085373246, 0.03340139000135432246, -7.446935725088736469 ) ) ;
#4214 = CARTESIAN_POINT ( 'NONE',  ( -67.68488546085839630, -283.1237833571631768, -207.2794874003663779 ) ) ;
#4215 = CARTESIAN_POINT ( 'NONE',  ( -20.56176820114410120, -297.3161699555620316, -193.5990152263022992 ) ) ;
#4216 = CARTESIAN_POINT ( 'NONE',  ( 31.26368744270867239, -280.1115420893711416, -302.6343871963346714 ) ) ;
#4217 = CARTESIAN_POINT ( 'NONE',  ( -52.09470046452793213, -287.1824143256771436, -195.2361257388816114 ) ) ;
#4218 = CARTESIAN_POINT ( 'NONE',  ( -56.06763861630832935, -289.1333197238089951, -340.9710225178475298 ) ) ;
#4219 = CARTESIAN_POINT ( 'NONE',  ( -94.98335340706431396, -279.4297103065441092, -316.2958365410439683 ) ) ;
#4220 = CARTESIAN_POINT ( 'NONE',  ( -111.7408124191033210, -294.4863248658026009, -277.0218771891208007 ) ) ;
#4221 = CARTESIAN_POINT ( 'NONE',  ( -93.52809752311577540, -298.9888713023584046, -222.1642072319880583 ) ) ;
#4222 = CARTESIAN_POINT ( 'NONE',  ( -96.42170391911561467, -276.7397615785031348, -313.9331218638359928 ) ) ;
#4223 = VERTEX_POINT ( 'NONE', #28254 ) ;
#4224 = CARTESIAN_POINT ( 'NONE',  ( -54.58630197043935794, -297.5031075614586484, -195.3386680176760422 ) ) ;
#4225 = CARTESIAN_POINT ( 'NONE',  ( -97.71240946786747372, -291.8749898890026202, -313.9121415457458397 ) ) ;
#4226 = CARTESIAN_POINT ( 'NONE',  ( 36.68770856708837869, -295.3811537351722336, -288.4736578652758112 ) ) ;
#4227 = LINE ( 'NONE', #33103, #24888 ) ;
#4228 = CARTESIAN_POINT ( 'NONE',  ( -70.01055816976165147, -290.1456800510612197, -335.7710074219556304 ) ) ;
#4229 = CARTESIAN_POINT ( 'NONE',  ( -48.18343439339133027, -253.0206516614774159, -465.6442049081569508 ) ) ;
#4230 = CARTESIAN_POINT ( 'NONE',  ( -106.4253858110398454, -297.6378463578126343, -236.5860212583945668 ) ) ;
#4231 = CARTESIAN_POINT ( 'NONE',  ( -112.9536128793037335, -288.7528828597431243, -265.5502835054620618 ) ) ;
#4232 = CARTESIAN_POINT ( 'NONE',  ( -101.5344022653336111, -297.4447039228560357, -227.8513359639053419 ) ) ;
#4233 = FACE_OUTER_BOUND ( 'NONE', #78998, .T. ) ;
#4234 = CARTESIAN_POINT ( 'NONE',  ( -113.4195521062967060, -291.9895813127763518, -276.9135001440978385 ) ) ;
#4235 = CARTESIAN_POINT ( 'NONE',  ( -2.602324593224680793, -291.1233781216987495, -342.4248175857292154 ) ) ;
#4236 = CARTESIAN_POINT ( 'NONE',  ( -101.1864263408305931, -287.0781584895506739, -231.2254389232448943 ) ) ;
#4237 = CARTESIAN_POINT ( 'NONE',  ( 24.58339754690349821, -272.9817730931796973, -228.3225214590135863 ) ) ;
#4238 = CARTESIAN_POINT ( 'NONE',  ( -91.25609276290481375, -275.1983037933019318, -219.0145704904673778 ) ) ;
#4239 = CARTESIAN_POINT ( 'NONE',  ( -100.0680832594036218, -288.0883092018522120, -310.4449683020284283 ) ) ;
#4240 = CARTESIAN_POINT ( 'NONE',  ( -48.29167134814407802, -279.0503558092549952, -345.3834968706803465 ) ) ;
#4241 = ORIENTED_EDGE ( 'NONE', *, *, #72732, .F. ) ;
#4243 = CARTESIAN_POINT ( 'NONE',  ( 23.77230217607897700, -280.3443105839075429, -230.1578303610482408 ) ) ;
#4242 = CARTESIAN_POINT ( 'NONE',  ( 19.67601529265115445, -280.9081409778063403, -224.7762506667461082 ) ) ;
#4244 = CARTESIAN_POINT ( 'NONE',  ( 37.88186786092692415, -276.8192925845438594, -285.2911993525877961 ) ) ;
#4245 = CARTESIAN_POINT ( 'NONE',  ( 38.03210091993377517, -280.5198121281973158, -284.1013343015498549 ) ) ;
#4246 = CARTESIAN_POINT ( 'NONE',  ( -49.04336257823442224, -154.3693876292917935, -362.0194686267980160 ) ) ;
#4247 = CARTESIAN_POINT ( 'NONE',  ( 28.89897917431056129, -276.9998969056514966, -309.1553523223985280 ) ) ;
#4248 = EDGE_CURVE ( 'NONE', #38673, #23012, #57142, .T. ) ;
#4249 = APPLICATION_PROTOCOL_DEFINITION ( 'draft international standard', 'automotive_design', 1998, #57764 ) ;
#4250 = CARTESIAN_POINT ( 'NONE',  ( -95.51182510166704276, -274.7442099589068789, -220.9553241550526650 ) ) ;
#4251 = CARTESIAN_POINT ( 'NONE',  ( 35.77081079830085031, -295.8376638359844719, -253.6410175316879361 ) ) ;
#4252 = ORIENTED_EDGE ( 'NONE', *, *, #90122, .F. ) ;
#4253 = VECTOR ( 'NONE', #13080, 1000.000000000000000 ) ;
#4254 = DIRECTION ( 'NONE',  ( 0.000000000000000000, 0.000000000000000000, 1.000000000000000000 ) ) ;
#4255 = CARTESIAN_POINT ( 'NONE',  ( 19.74728301808315578, -287.9840996634037538, -224.3512985151637338 ) ) ;
#4256 = CARTESIAN_POINT ( 'NONE',  ( 24.70455110511624142, -288.7237657098153818, -226.4725704908159685 ) ) ;
#4257 = CARTESIAN_POINT ( 'NONE',  ( -58.72686164203720693, -288.6846035173604719, -340.3179858515813407 ) ) ;
#4258 = CARTESIAN_POINT ( 'NONE',  ( -23.79057737923814742, -285.7283635367068086, -194.5712588073002109 ) ) ;
#4259 = CARTESIAN_POINT ( 'NONE',  ( 197.1195687025391976, 25.83768540896262778, 10.52967080450865822 ) ) ;
#4260 = CARTESIAN_POINT ( 'NONE',  ( 23.22985545500804960, -280.5333187678874651, -312.5218469854566479 ) ) ;
#4261 = CARTESIAN_POINT ( 'NONE',  ( 35.50071217969385629, -289.5990877771174041, -284.7394628909108860 ) ) ;
#4262 = CARTESIAN_POINT ( 'NONE',  ( -76.51189502661767960, -282.0660008204415021, -332.8426557925588440 ) ) ;
#4263 = CARTESIAN_POINT ( 'NONE',  ( -65.01724975514589744, -280.9980117507555519, -202.2780258716403523 ) ) ;
#4264 = CARTESIAN_POINT ( 'NONE',  ( -43.20578305953556963, -277.6205470209709461, -343.1869442604946130 ) ) ;
#4265 = CARTESIAN_POINT ( 'NONE',  ( -88.37348079797668277, -290.1504330764801693, -213.2317378068778453 ) ) ;
#4266 = CARTESIAN_POINT ( 'NONE',  ( -114.1930572173051814, -285.3237382281208738, -272.8542162425276842 ) ) ;
#4267 = CARTESIAN_POINT ( 'NONE',  ( -91.86380583107865050, -285.7917353686707429, -216.0760657778604639 ) ) ;
#4268 = CARTESIAN_POINT ( 'NONE',  ( 15.82731910058799585, -282.4396211179411580, -320.4545988898785254 ) ) ;
#4269 = VERTEX_POINT ( 'NONE', #6939 ) ;
#4270 = CARTESIAN_POINT ( 'NONE',  ( 145.2857639756989272, -299.5541904835127980, -192.9639945212225882 ) ) ;
#4271 = CARTESIAN_POINT ( 'NONE',  ( -107.2369079515141124, -292.7905245998764485, -241.1213265772720149 ) ) ;
#4272 = CARTESIAN_POINT ( 'NONE',  ( -30.72313024643193913, -290.8188571003982474, -194.0886686684267772 ) ) ;
#4273 = CARTESIAN_POINT ( 'NONE',  ( 35.87839481415820586, -274.5912753839438096, -268.8690911606510667 ) ) ;
#4274 = CARTESIAN_POINT ( 'NONE',  ( -44.79401450493713810, -294.4925861155777511, -346.9505620046683703 ) ) ;
#4275 = CARTESIAN_POINT ( 'NONE',  ( -104.1770757972027326, -289.4471480319974717, -239.3169509027828497 ) ) ;
#4276 = CARTESIAN_POINT ( 'NONE',  ( -89.22800780922275976, -294.0339188043994341, -323.2137024254167841 ) ) ;
#4277 = CARTESIAN_POINT ( 'NONE',  ( -100.6386522667229855, -291.2485799324754225, -307.6179672432508028 ) ) ;
#4278 = CYLINDRICAL_SURFACE ( 'NONE', #44327, 20.00000000000000355 ) ;
#4279 = CARTESIAN_POINT ( 'NONE',  ( -112.2524175955854844, -292.5053411541834976, -274.0196770573660388 ) ) ;
#4280 = CARTESIAN_POINT ( 'NONE',  ( -5.360478627843927590, -290.4718106534627964, -202.3373728463376438 ) ) ;
#4281 = CARTESIAN_POINT ( 'NONE',  ( 37.60692213002425177, -295.6027232527513320, -274.2868913662403543 ) ) ;
#4282 = CARTESIAN_POINT ( 'NONE',  ( -37.29271205320124238, -286.9939975706553810, -197.1133604448681638 ) ) ;
#4283 = CARTESIAN_POINT ( 'NONE',  ( -16.26216608198313907, -276.3030766908516398, -197.9601632865850718 ) ) ;
#4284 = CARTESIAN_POINT ( 'NONE',  ( -12.01203535027179825, -275.5247400301428229, -342.7107126001876622 ) ) ;
#4285 = CARTESIAN_POINT ( 'NONE',  ( -36.53244849369291813, -297.2592142849998709, -193.5227000370792609 ) ) ;
#4286 = CARTESIAN_POINT ( 'NONE',  ( 20.80483173727489188, -274.4293722689355945, -316.1740407382618514 ) ) ;
#4287 = CARTESIAN_POINT ( 'NONE',  ( -39.72327999011758237, -278.1018875852079191, -195.9464540011245788 ) ) ;
#4288 = CARTESIAN_POINT ( 'NONE',  ( -54.31819140029412551, -275.0342719877373838, -198.9543308562912500 ) ) ;
#4289 = CARTESIAN_POINT ( 'NONE',  ( -79.79754388434909629, -276.0152815932032127, -333.7013552730261381 ) ) ;
#4290 = CARTESIAN_POINT ( 'NONE',  ( 199.9390245229544405, 68.58287003104832991, 4.389327654508852206 ) ) ;
#4291 = CARTESIAN_POINT ( 'NONE',  ( -107.2964998494803126, -273.4861947032821377, -248.9692968721127215 ) ) ;
#4292 = CARTESIAN_POINT ( 'NONE',  ( 197.2116943569230330, 276.0000000000000568, -11.92446933126074882 ) ) ;
#4294 = CARTESIAN_POINT ( 'NONE',  ( 0.6142787894519449177, -274.4069187278359436, -208.0045331745921544 ) ) ;
#4293 = CARTESIAN_POINT ( 'NONE',  ( 22.81363351863807054, -286.1898352083263148, -315.7455056044452704 ) ) ;
#4295 = CARTESIAN_POINT ( 'NONE',  ( -6.919925778501975877, -288.6638310299311456, -341.1108912274279987 ) ) ;
#4296 = CARTESIAN_POINT ( 'NONE',  ( -111.5227320609347288, -289.9611542323395383, -290.9261074780434910 ) ) ;
#4297 = CARTESIAN_POINT ( 'NONE',  ( -4.335954344953206530, -300.4432659257108753, -194.9948368513721562 ) ) ;
#4298 = CARTESIAN_POINT ( 'NONE',  ( 15.59562159072019583, -292.3014939920101938, -323.3269408233277318 ) ) ;
#4299 = ADVANCED_FACE ( 'NONE', ( #57596 ), #86440, .F. ) ;
#4300 = CARTESIAN_POINT ( 'NONE',  ( 27.72008475687179185, -280.2118207979277145, -229.3820127615050524 ) ) ;
#4301 = ADVANCED_FACE ( 'NONE', ( #44761 ), #59459, .F. ) ;
#4302 = LINE ( 'NONE', #17587, #66830 ) ;
#4303 = CARTESIAN_POINT ( 'NONE',  ( -112.0563281125624258, -276.6431129019024979, -263.2641419807241050 ) ) ;
#4304 = CARTESIAN_POINT ( 'NONE',  ( 204.6539576904058606, 287.9062406767683910, -5.225551010890931103 ) ) ;
#4305 = CARTESIAN_POINT ( 'NONE',  ( -92.72137645607988077, -288.6633476063824446, -318.6057721245113044 ) ) ;
#4306 = CARTESIAN_POINT ( 'NONE',  ( -36.09237171215956863, -55.96374926131388605, 22.50000000000000000 ) ) ;
#4307 = LINE ( 'NONE', #67779, #57934 ) ;
#4308 = CARTESIAN_POINT ( 'NONE',  ( -41.68383955003493924, -289.9974237814847697, -195.4357007680625316 ) ) ;
#4309 = CARTESIAN_POINT ( 'NONE',  ( -32.66619857750620071, -275.6322390957025164, -196.8036057870655497 ) ) ;
#4310 = CARTESIAN_POINT ( 'NONE',  ( -19.04178497067908182, -284.2464920273695839, -344.6027149983022468 ) ) ;
#4312 = CARTESIAN_POINT ( 'NONE',  ( -48.32868293023025785, -283.1958957875103238, -342.5295751429100619 ) ) ;
#4311 = CARTESIAN_POINT ( 'NONE',  ( -15.38253172874556185, -296.3458519441296630, -195.0132753957137766 ) ) ;
#4313 = CARTESIAN_POINT ( 'NONE',  ( 22.75159493093351415, -276.3890078506522059, -227.8637798803263195 ) ) ;
#4314 = CARTESIAN_POINT ( 'NONE',  ( 13.60178376479612794, -275.5911607936069458, -217.8505173805758091 ) ) ;
#4315 = CARTESIAN_POINT ( 'NONE',  ( -11.37006930069944310, -284.7141020945844616, -340.7759129648206908 ) ) ;
#4317 = CARTESIAN_POINT ( 'NONE',  ( -39.16220003467072530, -297.0875296385581805, -197.1360045099840477 ) ) ;
#4316 = AXIS2_PLACEMENT_3D ( 'NONE', #76033, #91140, #68939 ) ;
#4318 = ORIENTED_EDGE ( 'NONE', *, *, #34465, .T. ) ;
#4319 = CARTESIAN_POINT ( 'NONE',  ( 204.4793297709846911, 295.2867319150298613, -54.00000000005014300 ) ) ;
#4320 = CARTESIAN_POINT ( 'NONE',  ( 38.07015933274296771, -293.5800473194682354, -285.9191209774903655 ) ) ;
#4321 = CARTESIAN_POINT ( 'NONE',  ( -84.71067997099605407, -287.3759808388974761, -212.6048904755965623 ) ) ;
#4322 = DIRECTION ( 'NONE',  ( -0.8195702660915913373, 0.000000000000000000, 0.5729786897769918452 ) ) ;
#4323 = CARTESIAN_POINT ( 'NONE',  ( -19.11405058567864046, -274.3380690714489560, -350.3683826091709648 ) ) ;
#4324 = CARTESIAN_POINT ( 'NONE',  ( -113.1415552914096025, -277.5915202344523891, -282.9524156863793110 ) ) ;
#4325 = CARTESIAN_POINT ( 'NONE',  ( -99.23253275600042400, -288.3564317357208324, -314.8353118505963835 ) ) ;
#4326 = CARTESIAN_POINT ( 'NONE',  ( -87.38560458511349793, -285.2851078335249895, -324.5263425455733568 ) ) ;
#4327 = CARTESIAN_POINT ( 'NONE',  ( -26.85610241278956067, -278.6771306295833597, -343.6279334750709040 ) ) ;
#4328 = CARTESIAN_POINT ( 'NONE',  ( -110.3683287282665191, -286.2640424177569685, -247.6947197772464904 ) ) ;
#4329 = CARTESIAN_POINT ( 'NONE',  ( -57.67936274330781998, -281.7897016535160901, -198.1712286255379638 ) ) ;
#4330 = CARTESIAN_POINT ( 'NONE',  ( -24.16169608688228010, -274.3825450011969451, -194.4433407492400647 ) ) ;
#4331 = CARTESIAN_POINT ( 'NONE',  ( -65.09705353670513261, -277.2381374406559189, -342.2410803135458082 ) ) ;
#4332 = CARTESIAN_POINT ( 'NONE',  ( -38.33750351381376476, -296.9848841524737963, -344.7944611630506984 ) ) ;
#4333 = CARTESIAN_POINT ( 'NONE',  ( 151.9709352735115147, -299.5541904835127980, -192.9639945212225882 ) ) ;
#4334 = CARTESIAN_POINT ( 'NONE',  ( 175.2296996224750103, 214.5000000000000568, 0.000000000000000000 ) ) ;
#4335 = CARTESIAN_POINT ( 'NONE',  ( -29.20084367881113252, -296.2926237717836671, -194.5988578826594164 ) ) ;
#4336 = CARTESIAN_POINT ( 'NONE',  ( -8.720343734134340608, -276.1749290462664135, -337.5967390545733906 ) ) ;
#4337 = CARTESIAN_POINT ( 'NONE',  ( -40.44158779905904311, -299.0938404527728949, -193.6809872192189346 ) ) ;
#4338 = CARTESIAN_POINT ( 'NONE',  ( 34.36481372306668902, -289.0730028061952339, -251.9756347728458366 ) ) ;
#4339 = CARTESIAN_POINT ( 'NONE',  ( -113.6175786899859190, -298.1173755723638692, -266.7872336141744540 ) ) ;
#4340 = CARTESIAN_POINT ( 'NONE',  ( -88.32963576417394336, -296.9525763058929897, -327.6007515792217646 ) ) ;
#4341 = CARTESIAN_POINT ( 'NONE',  ( -108.6925730765285181, -292.2585448293478976, -293.0951522366988229 ) ) ;
#4342 = CARTESIAN_POINT ( 'NONE',  ( -88.77258847826377064, -277.3284009994634971, -215.9306094870748041 ) ) ;
#4343 = CARTESIAN_POINT ( 'NONE',  ( -111.3325675027123651, -280.3608082087097273, -278.9803645532674068 ) ) ;
#4344 = CARTESIAN_POINT ( 'NONE',  ( -75.93673604751245421, -295.6126749478929128, -206.6481063102666553 ) ) ;
#4345 = CARTESIAN_POINT ( 'NONE',  ( -35.89857773759159443, -284.8946778257179062, -346.1250828407030440 ) ) ;
#4346 = CARTESIAN_POINT ( 'NONE',  ( 18.01861155572832018, -285.7902995542362987, -222.3042561985201644 ) ) ;
#4347 = CARTESIAN_POINT ( 'NONE',  ( 104.7134020687092288, 115.3893350944124023, -282.6128408094983797 ) ) ;
#4348 = VERTEX_POINT ( 'NONE', #36269 ) ;
#4349 = CARTESIAN_POINT ( 'NONE',  ( 15.04762028614208980, -286.4836426377549401, -219.4941680710666958 ) ) ;
#4350 = VERTEX_POINT ( 'NONE', #30561 ) ;
#4351 = CARTESIAN_POINT ( 'NONE',  ( 30.44214174502560866, -282.1654325912812169, -234.3753410823629508 ) ) ;
#4352 = CARTESIAN_POINT ( 'NONE',  ( -93.79743264964480431, -273.5414747823694483, -224.0291723794845495 ) ) ;
#4353 = CARTESIAN_POINT ( 'NONE',  ( -37.96374475585426467, -284.8394515829972420, -193.7607147140849122 ) ) ;
#4354 = CARTESIAN_POINT ( 'NONE',  ( -28.26475800910624159, -281.1057687455061682, -194.0814854761429160 ) ) ;
#4355 = CARTESIAN_POINT ( 'NONE',  ( 196.8803347170859865, 73.40565171261609123, -12.49999999999998579 ) ) ;
#4356 = CARTESIAN_POINT ( 'NONE',  ( -38.18186819212120042, -281.5619175406736190, -194.0590742811003793 ) ) ;
#4357 = CARTESIAN_POINT ( 'NONE',  ( 38.40552625923182717, -282.0579204756764966, -284.1493837232054034 ) ) ;
#4358 = CARTESIAN_POINT ( 'NONE',  ( -105.5795714935544112, -282.2666405000203440, -254.7536222014695397 ) ) ;
#4359 = CARTESIAN_POINT ( 'NONE',  ( 45.61465944062903333, 12.28553147226080355, -332.1500543120573639 ) ) ;
#4360 = ORIENTED_EDGE ( 'NONE', *, *, #66323, .T. ) ;
#4361 = CARTESIAN_POINT ( 'NONE',  ( -75.22288142050554427, -275.5466224907591481, -205.7639240263404758 ) ) ;
#4362 = CARTESIAN_POINT ( 'NONE',  ( 201.5581938671040518, 293.7308772661893386, -83.16477369446880630 ) ) ;
#4363 = CARTESIAN_POINT ( 'NONE',  ( 29.61557273233616883, -280.0108887494052965, -303.4718305634746685 ) ) ;
#4364 = CARTESIAN_POINT ( 'NONE',  ( 38.23175922701547336, -295.4187360515148839, -278.7602937214786607 ) ) ;
#4365 = CARTESIAN_POINT ( 'NONE',  ( -10.46022511962803314, -294.0404835468467013, -338.3411074621490684 ) ) ;
#4366 = CARTESIAN_POINT ( 'NONE',  ( -74.64356818023807705, -291.0770540033107636, -203.0699778292946860 ) ) ;
#4367 = CARTESIAN_POINT ( 'NONE',  ( 170.2305261370685798, 250.5000000000000568, -24.90909090909090295 ) ) ;
#4369 = CARTESIAN_POINT ( 'NONE',  ( 34.47493497500671111, -286.1737906604378736, -287.3555682555879685 ) ) ;
#4368 = CARTESIAN_POINT ( 'NONE',  ( -110.6552176378702228, -294.8541593320919674, -291.9418012946524073 ) ) ;
#4370 = CARTESIAN_POINT ( 'NONE',  ( 24.35486496336018902, -294.8487427027795320, -229.0767464079922036 ) ) ;
#4371 = CARTESIAN_POINT ( 'NONE',  ( -100.0387176662299851, -286.3932823897014259, -231.9192731867592840 ) ) ;
#4372 = ORIENTED_EDGE ( 'NONE', *, *, #31927, .F. ) ;
#4373 = CARTESIAN_POINT ( 'NONE',  ( 31.96834765718888249, -294.0677181543535994, -237.2385729010899524 ) ) ;
#4374 = CARTESIAN_POINT ( 'NONE',  ( 33.38466208303379545, -282.2867953956458109, -288.7349995409943517 ) ) ;
#4375 = CARTESIAN_POINT ( 'NONE',  ( -109.4717886956513269, -295.6743550546011079, -244.5685019611752864 ) ) ;
#4376 = CARTESIAN_POINT ( 'NONE',  ( -99.73316204540834917, -290.7590045266941274, -315.2330078204165034 ) ) ;
#4377 = CARTESIAN_POINT ( 'NONE',  ( -68.30975204457119787, -292.1485224526916227, -199.9158975258618796 ) ) ;
#4378 = CARTESIAN_POINT ( 'NONE',  ( -8.216541390353109264, -288.8266213144314634, -337.3533770767477336 ) ) ;
#4379 = ORIENTED_EDGE ( 'NONE', *, *, #41255, .F. ) ;
#4380 = CARTESIAN_POINT ( 'NONE',  ( 222.8344101925596306, 0.000000000000000000, 21.50000000000000000 ) ) ;
#4381 = CARTESIAN_POINT ( 'NONE',  ( -85.59020269727244568, -297.5719576801733979, -328.7767620998354801 ) ) ;
#4382 = CARTESIAN_POINT ( 'NONE',  ( 30.26323651991097208, -297.5666936174177977, -193.8689913825462554 ) ) ;
#4383 = CARTESIAN_POINT ( 'NONE',  ( -16.84441383036666195, -279.3822257687527895, -200.0527279998552501 ) ) ;
#4384 = ORIENTED_EDGE ( 'NONE', *, *, #60666, .F. ) ;
#4385 = CARTESIAN_POINT ( 'NONE',  ( 37.53052916771648029, -275.2821372374443172, -288.1287512367670729 ) ) ;
#4386 = CIRCLE ( 'NONE', #64928, 5.603083949679982467 ) ;
#4387 = CARTESIAN_POINT ( 'NONE',  ( -52.76144917968251491, -296.3309848438457834, -198.2466920969861235 ) ) ;
#4388 = CARTESIAN_POINT ( 'NONE',  ( -18.68400137620172430, -278.6697342516281992, -342.2134370463454047 ) ) ;
#4389 = CARTESIAN_POINT ( 'NONE',  ( 34.71373914236907865, -273.4600155537742694, -252.5039302194523998 ) ) ;
#4390 = CARTESIAN_POINT ( 'NONE',  ( -71.09984203453312546, -296.7131203023845956, -335.5481651650862887 ) ) ;
#4391 = CARTESIAN_POINT ( 'NONE',  ( -97.14282222425553925, -298.2214131598252038, -227.9576762577838451 ) ) ;
#4392 = DIRECTION ( 'NONE',  ( 0.000000000000000000, 1.000000000000000000, 0.000000000000000000 ) ) ;
#4393 = CARTESIAN_POINT ( 'NONE',  ( -106.4323516233798017, -297.7366112216848251, -302.5002263921336976 ) ) ;
#4394 = CARTESIAN_POINT ( 'NONE',  ( -93.83628602626684767, -271.2622846344066829, -220.4936078306820946 ) ) ;
#4395 = CARTESIAN_POINT ( 'NONE',  ( 6.731104131827689407, -293.3213210597814964, -212.0389044399694569 ) ) ;
#4396 = CARTESIAN_POINT ( 'NONE',  ( -107.9556217973475611, -289.3992553413693258, -249.6029152947801322 ) ) ;
#4397 = CARTESIAN_POINT ( 'NONE',  ( 207.4724402404596333, 29.73442829110635444, 14.90057469441955362 ) ) ;
#4398 = CARTESIAN_POINT ( 'NONE',  ( -18.57106110723369596, -274.7798704578709135, -195.6925283120649510 ) ) ;
#4399 = CARTESIAN_POINT ( 'NONE',  ( -92.01956818916413283, -273.4098560835121248, -221.9944895202328041 ) ) ;
#4400 = CARTESIAN_POINT ( 'NONE',  ( 17.93608662617683791, -282.8191428185303380, -219.1481011331267439 ) ) ;
#4401 = CARTESIAN_POINT ( 'NONE',  ( 17.46125741984589652, -280.9743632908815698, -323.8215731871285357 ) ) ;
#4402 = CARTESIAN_POINT ( 'NONE',  ( -106.2577176533503405, -277.4603495535039883, -304.5968569752323560 ) ) ;
#4403 = CARTESIAN_POINT ( 'NONE',  ( -108.8801102275217971, -283.5468169684576196, -285.7457221856930119 ) ) ;
#4404 = CARTESIAN_POINT ( 'NONE',  ( -0.06353451936536706757, -280.5572363385340395, -335.6474702640018108 ) ) ;
#4405 = CARTESIAN_POINT ( 'NONE',  ( -2.619734573024061319, -273.0955980956678104, -205.4784544565968929 ) ) ;
#4406 = CARTESIAN_POINT ( 'NONE',  ( -112.3822258285517961, -280.5359418150429178, -271.6364700943818775 ) ) ;
#4407 = CARTESIAN_POINT ( 'NONE',  ( 157.7374095173865385, 14.19731191252289015, 10.00000000000000000 ) ) ;
#4408 = FACE_OUTER_BOUND ( 'NONE', #57371, .T. ) ;
#4409 = CARTESIAN_POINT ( 'NONE',  ( -36.18080114837113115, -296.3063621436284052, -194.3747869642731985 ) ) ;
#4410 = CARTESIAN_POINT ( 'NONE',  ( -69.49315066435812582, -279.4743752187947621, -338.3186618418029639 ) ) ;
#4411 = EDGE_CURVE ( 'NONE', #22214, #89903, #24812, .T. ) ;
#4412 = DIRECTION ( 'NONE',  ( 0.000000000000000000, 1.000000000000000000, 0.000000000000000000 ) ) ;
#4413 = CARTESIAN_POINT ( 'NONE',  ( -104.4929723554661507, -286.0159826572646011, -305.1165235463112708 ) ) ;
#4414 = CARTESIAN_POINT ( 'NONE',  ( 156.4892692376084256, 15.19211566834932192, -9.995848581181771664 ) ) ;
#4415 = CARTESIAN_POINT ( 'NONE',  ( 17.04995857286303362, -284.8273217527765269, -218.7039645495036098 ) ) ;
#4416 = CARTESIAN_POINT ( 'NONE',  ( 207.3051956367744424, 29.36351352329048581, 13.69055975427936289 ) ) ;
#4417 = CARTESIAN_POINT ( 'NONE',  ( -106.3658192058961873, -295.0146595374200160, -295.4666403463573943 ) ) ;
#4418 = CARTESIAN_POINT ( 'NONE',  ( -7.747493166749691795, -286.7998529430500412, -338.4972519408854055 ) ) ;
#4419 = CARTESIAN_POINT ( 'NONE',  ( -115.8664652629750549, -267.0802710791712116, -295.7299871733738996 ) ) ;
#4420 = CARTESIAN_POINT ( 'NONE',  ( -96.00004155097701641, -295.1944313328239105, -223.6256963487992380 ) ) ;
#4421 = CARTESIAN_POINT ( 'NONE',  ( -87.28143286770665554, -283.8509541772170337, -212.5960267653878475 ) ) ;
#4422 = CARTESIAN_POINT ( 'NONE',  ( 34.72599896870750058, -283.3597053636372038, -286.2572547625211996 ) ) ;
#4423 = CARTESIAN_POINT ( 'NONE',  ( 37.79620794229941083, -279.6441498786120405, -258.6936146589770260 ) ) ;
#4424 = CARTESIAN_POINT ( 'NONE',  ( -101.6431463815702898, -290.0796025691736304, -305.0272853527728216 ) ) ;
#4425 = CARTESIAN_POINT ( 'NONE',  ( -104.9908093272758833, -280.3634047989733062, -241.3960883750020798 ) ) ;
#4426 = CARTESIAN_POINT ( 'NONE',  ( 18.95381865755613404, -281.6935403467549577, -223.6146377524373747 ) ) ;
#4427 = CARTESIAN_POINT ( 'NONE',  ( 25.74663376963620820, -288.9787978701504585, -229.1510594006102508 ) ) ;
#4428 = ORIENTED_EDGE ( 'NONE', *, *, #46324, .T. ) ;
#4429 = CARTESIAN_POINT ( 'NONE',  ( -88.03637051047577700, -273.3660892892744982, -212.3329135229915039 ) ) ;
#4430 = CARTESIAN_POINT ( 'NONE',  ( -91.77531105708733605, -291.8124940825813383, -321.5132671151195609 ) ) ;
#4431 = CARTESIAN_POINT ( 'NONE',  ( 157.7374095173865385, -21.37379927922774314, 13.00000000000000178 ) ) ;
#4432 = CARTESIAN_POINT ( 'NONE',  ( 44.71564893372296723, -290.0519495502701943, -270.3284710469131937 ) ) ;
#4433 = VERTEX_POINT ( 'NONE', #7388 ) ;
#4434 = CARTESIAN_POINT ( 'NONE',  ( 37.78970020583974332, -273.5983726905885192, -273.9816781106921439 ) ) ;
#4435 = LINE ( 'NONE', #11542, #57938 ) ;
#4436 = CARTESIAN_POINT ( 'NONE',  ( -1.104756786260240764, -292.9794252604567077, -337.4081104003678888 ) ) ;
#4437 = CARTESIAN_POINT ( 'NONE',  ( -96.14612360009986958, -296.6672362159974341, -226.9807065598966460 ) ) ;
#4438 = CARTESIAN_POINT ( 'NONE',  ( 12.64013289151602493, -289.8605528047412463, -324.5832618425941973 ) ) ;
#4439 = CARTESIAN_POINT ( 'NONE',  ( -69.42847045845644516, -285.2404528966351336, -337.0715356234218234 ) ) ;
#4440 = CARTESIAN_POINT ( 'NONE',  ( -66.80513984946860262, -293.0988363928310605, -199.8592597562300170 ) ) ;
#4441 = CARTESIAN_POINT ( 'NONE',  ( -105.5719445902916931, -292.3171037527162639, -235.6331031278305375 ) ) ;
#4442 = CARTESIAN_POINT ( 'NONE',  ( -6.208915370107641607, -288.4613230956734924, -202.1139585754389714 ) ) ;
#4443 = CARTESIAN_POINT ( 'NONE',  ( -3.659525067055291903, -280.6510602797544038, -201.1041918721884372 ) ) ;
#4444 = CARTESIAN_POINT ( 'NONE',  ( -112.7974062411733343, -294.5700472872175055, -275.2219055470237663 ) ) ;
#4445 = CARTESIAN_POINT ( 'NONE',  ( -65.25416720483168831, -283.2403397505250950, -342.1380851777612975 ) ) ;
#4446 = CARTESIAN_POINT ( 'NONE',  ( 26.32316238324563074, -276.8949517552385942, -232.0824090322860798 ) ) ;
#4447 = CARTESIAN_POINT ( 'NONE',  ( 30.91033621190086578, -284.2662352645559167, -285.9065529553535612 ) ) ;
#4448 = VECTOR ( 'NONE', #56643, 1000.000000000000000 ) ;
#4449 = CARTESIAN_POINT ( 'NONE',  ( -79.55791378705039563, -275.7550359584861894, -333.3376935469220257 ) ) ;
#4450 = CARTESIAN_POINT ( 'NONE',  ( 154.7659666677267865, 20.47222690886501439, -12.53936336329526391 ) ) ;
#4451 = CARTESIAN_POINT ( 'NONE',  ( -67.81574721948939555, -282.9709276078943958, -336.7638355152207623 ) ) ;
#4452 = CARTESIAN_POINT ( 'NONE',  ( -113.6820063142510548, -279.6698648228827437, -277.3104055157913876 ) ) ;
#4453 = AXIS2_PLACEMENT_3D ( 'NONE', #13982, #86861, #13518 ) ;
#4454 = CARTESIAN_POINT ( 'NONE',  ( -40.79385542200716941, -285.0686119178861304, -193.6220391609869012 ) ) ;
#4455 = CARTESIAN_POINT ( 'NONE',  ( -70.69719085749100884, -293.3661162045929132, -204.2900558275705691 ) ) ;
#4456 = CARTESIAN_POINT ( 'NONE',  ( 37.93409632436373613, -277.0016873660071610, -258.4452096673913388 ) ) ;
#4457 = ADVANCED_FACE ( 'NONE', ( #73661 ), #33869, .F. ) ;
#4458 = CARTESIAN_POINT ( 'NONE',  ( 13.62340598719713824, -276.0633693407946794, -213.2302261979895661 ) ) ;
#4459 = CARTESIAN_POINT ( 'NONE',  ( 0.000000000000000000, 0.000000000000000000, 13.00000000000000178 ) ) ;
#4460 = CARTESIAN_POINT ( 'NONE',  ( 31.26103323153933644, -275.7197067577321832, -295.4612537763394471 ) ) ;
#4461 = CARTESIAN_POINT ( 'NONE',  ( -61.58357070194952598, -297.3678486710958850, -341.2140544523533663 ) ) ;
#4462 = CARTESIAN_POINT ( 'NONE',  ( -111.9250100420552769, -282.4733336955501954, -276.4732621857104391 ) ) ;
#4463 = CARTESIAN_POINT ( 'NONE',  ( -58.92868767960735710, -291.4469950619443352, -196.4710221652081259 ) ) ;
#4464 = CARTESIAN_POINT ( 'NONE',  ( 38.77727348086906289, -289.0952099648609419, -265.8452818068897159 ) ) ;
#4465 = CARTESIAN_POINT ( 'NONE',  ( 34.78978374617169322, -292.2996452670188887, -257.2040322935956169 ) ) ;
#4466 = EDGE_LOOP ( 'NONE', ( #42447, #92408, #69125, #53684, #20238, #13242 ) ) ;
#4467 = CARTESIAN_POINT ( 'NONE',  ( 19.94902896013509164, -291.4367960760712322, -219.7807011821576850 ) ) ;
#4468 = CARTESIAN_POINT ( 'NONE',  ( 10.94796830920859598, -292.4086912619670215, -215.5196029281491406 ) ) ;
#4469 = VERTEX_POINT ( 'NONE', #80752 ) ;
#4470 = CARTESIAN_POINT ( 'NONE',  ( -67.91795386975798010, -290.5239002095117939, -340.6930823913618838 ) ) ;
#4471 = CARTESIAN_POINT ( 'NONE',  ( -66.08193070137932068, -279.9986603228350077, -203.2200835328744404 ) ) ;
#4472 = CARTESIAN_POINT ( 'NONE',  ( -113.9260196751459944, -295.4103946427232472, -275.3056861123669705 ) ) ;
#4473 = CARTESIAN_POINT ( 'NONE',  ( -102.4366065921983733, -285.7403426842598151, -229.4225550025113023 ) ) ;
#4474 = CARTESIAN_POINT ( 'NONE',  ( 9.794459312831646614, -287.0146167073599486, -209.5012234328941361 ) ) ;
#4475 = CARTESIAN_POINT ( 'NONE',  ( -109.8932482333227370, -284.7706486160037116, -279.0650878718708441 ) ) ;
#4476 = CARTESIAN_POINT ( 'NONE',  ( 121.4031722996727325, 149.7340073792644830, -263.5263209816934022 ) ) ;
#4477 = CARTESIAN_POINT ( 'NONE',  ( -64.80429634339824929, -181.9903270017377963, -361.1305515816413845 ) ) ;
#4478 = CARTESIAN_POINT ( 'NONE',  ( 199.9948420232396131, 290.8510889670257598, -82.40867480343716522 ) ) ;
#4479 = CARTESIAN_POINT ( 'NONE',  ( 28.01010196456579138, -274.3039257947781380, -237.4712458382358022 ) ) ;
#4480 = CARTESIAN_POINT ( 'NONE',  ( -37.82554206253664120, -275.9786430995062574, -343.6811398426501682 ) ) ;
#4481 = CARTESIAN_POINT ( 'NONE',  ( -95.52044571051723665, -296.7411457569862137, -219.9352081809657591 ) ) ;
#4482 = CARTESIAN_POINT ( 'NONE',  ( -75.69614664873641630, -208.8793829413635308, -354.1463231226688890 ) ) ;
#4483 = CARTESIAN_POINT ( 'NONE',  ( 25.65125340681422372, -274.8149596424457286, -313.8715148012267946 ) ) ;
#4484 = CARTESIAN_POINT ( 'NONE',  ( -33.76073202455672373, -299.9578568962608642, -196.1247607683412468 ) ) ;
#4485 = CARTESIAN_POINT ( 'NONE',  ( -35.84592400321518113, -299.0116964481301238, -193.5961778596468719 ) ) ;
#4486 = CARTESIAN_POINT ( 'NONE',  ( 35.05624986874159532, -287.9101389311853723, -260.1670901906311997 ) ) ;
#4487 = CARTESIAN_POINT ( 'NONE',  ( -76.99012796964659344, -296.3715381577441121, -336.2421676807063022 ) ) ;
#4488 = CARTESIAN_POINT ( 'NONE',  ( -91.59657762063839925, -297.7964346795590700, -215.8089853806745566 ) ) ;
#4489 = CARTESIAN_POINT ( 'NONE',  ( 6.064644046955196544, -294.6115597621364373, -329.1172945606851954 ) ) ;
#4490 = VERTEX_POINT ( 'NONE', #73200 ) ;
#4491 = ADVANCED_FACE ( 'NONE', ( #1223 ), #8772, .T. ) ;
#4492 = CARTESIAN_POINT ( 'NONE',  ( 37.31688773893979061, -277.6248027674322429, -282.3267299317424772 ) ) ;
#4493 = ORIENTED_EDGE ( 'NONE', *, *, #8814, .T. ) ;
#4494 = CARTESIAN_POINT ( 'NONE',  ( -64.71456643181417689, -279.2119233047650937, -198.4004635590715679 ) ) ;
#4495 = CARTESIAN_POINT ( 'NONE',  ( -35.09845810005103317, -277.9645489644905751, -343.5620490826685227 ) ) ;
#4496 = CARTESIAN_POINT ( 'NONE',  ( 30.95448136916065707, -277.7470418235819807, -303.7917817540888450 ) ) ;
#4497 = CARTESIAN_POINT ( 'NONE',  ( -107.1425661717945985, -276.2037867860376537, -298.7555875120523865 ) ) ;
#4498 = CARTESIAN_POINT ( 'NONE',  ( -76.60257407051686585, -274.0034220950490180, -208.7447872019239412 ) ) ;
#4499 = CARTESIAN_POINT ( 'NONE',  ( -84.87240992961781672, -294.2970994256663744, -326.6081637078360700 ) ) ;
#4500 = CARTESIAN_POINT ( 'NONE',  ( 152.0139507567511998, 20.82771571514204467, -9.304222368685264755 ) ) ;
#4501 = CARTESIAN_POINT ( 'NONE',  ( -76.35402572753500294, -277.7560769139649892, -332.1217705409205223 ) ) ;
#4502 = CARTESIAN_POINT ( 'NONE',  ( 22.01188697103727421, -286.8890492353381205, -318.6564642408707755 ) ) ;
#4503 = CARTESIAN_POINT ( 'NONE',  ( -1.036491026389169123, -276.5341259920437551, -204.7192931778294565 ) ) ;
#4504 = CARTESIAN_POINT ( 'NONE',  ( 208.6208076322478746, 32.98517505407394168, 10.00000000000000000 ) ) ;
#4505 = CARTESIAN_POINT ( 'NONE',  ( -53.45401580810245434, -288.4613374929169254, -341.7263406743113023 ) ) ;
#4506 = CARTESIAN_POINT ( 'NONE',  ( -92.36659915629896034, -283.1629151545395757, -324.0786502548191379 ) ) ;
#4507 = EDGE_CURVE ( 'NONE', #50747, #1828, #77739, .T. ) ;
#4508 = CARTESIAN_POINT ( 'NONE',  ( 34.75247382928597517, -279.5741336227684997, -253.6158470662637114 ) ) ;
#4510 = CARTESIAN_POINT ( 'NONE',  ( -111.8315654330356779, -282.6250756368986004, -270.8957085002210192 ) ) ;
#4509 = CARTESIAN_POINT ( 'NONE',  ( 20.99406027203965053, -279.5004030761576814, -225.4818076967800096 ) ) ;
#4512 = CARTESIAN_POINT ( 'NONE',  ( -102.4856526618863768, -287.0491087079658428, -233.0922363453260573 ) ) ;
#4511 = CIRCLE ( 'NONE', #30206, 1.000000000000000888 ) ;
#4513 = CARTESIAN_POINT ( 'NONE',  ( -102.5154956978138756, -280.2151364249276071, -236.4938788253674886 ) ) ;
#4514 = CARTESIAN_POINT ( 'NONE',  ( 154.5829541210975151, 19.45714094959671314, -12.72029999255603450 ) ) ;
#4515 = CARTESIAN_POINT ( 'NONE',  ( 24.82058582463015028, -294.9835569248187994, -228.3073100600224166 ) ) ;
#4516 = CARTESIAN_POINT ( 'NONE',  ( -111.8051715203650360, -276.5993514929936055, -285.5637239842043869 ) ) ;
#4517 = AXIS2_PLACEMENT_3D ( 'NONE', #5375, #12457, #71640 ) ;
#4518 = CARTESIAN_POINT ( 'NONE',  ( 26.86024205217384164, -276.6813364551920245, -305.4241236169632998 ) ) ;
#4519 = CARTESIAN_POINT ( 'NONE',  ( -106.5294224214257497, -286.1676952650918793, -299.8725170507947837 ) ) ;
#4520 = CARTESIAN_POINT ( 'NONE',  ( 197.4836817735085219, 24.47698789593438917, 11.66666666666666785 ) ) ;
#4521 = CARTESIAN_POINT ( 'NONE',  ( -79.71251375888961377, -291.5397226768191672, -332.9865081745542170 ) ) ;
#4522 = CARTESIAN_POINT ( 'NONE',  ( -56.01809048318838080, -293.2923762727940584, -343.0515620962855792 ) ) ;
#4523 = CARTESIAN_POINT ( 'NONE',  ( -21.00830358765497508, -285.4537868550945632, -195.2786368205123040 ) ) ;
#4524 = CARTESIAN_POINT ( 'NONE',  ( -100.3845383080752782, -289.4747267172832608, -231.9939318939462396 ) ) ;
#4525 = LINE ( 'NONE', #41426, #82904 ) ;
#4526 = CARTESIAN_POINT ( 'NONE',  ( -11.09345012332124192, -275.3875286777388851, -339.0071145870588225 ) ) ;
#4527 = CARTESIAN_POINT ( 'NONE',  ( -0.1594568512881724687, -292.6919181326035755, -334.6719867168451970 ) ) ;
#4528 = CARTESIAN_POINT ( 'NONE',  ( 197.2564953664965515, 42.34359863175593119, 11.92066879148802272 ) ) ;
#4529 = CARTESIAN_POINT ( 'NONE',  ( -103.9948696362666425, -289.5180309084092301, -233.2119222219740777 ) ) ;
#4530 = CARTESIAN_POINT ( 'NONE',  ( -109.1485954315176343, -286.3752296681469147, -253.2710706312244611 ) ) ;
#4531 = CARTESIAN_POINT ( 'NONE',  ( -29.10953442217389764, -287.1891884170248090, -345.9533682510087829 ) ) ;
#4532 = EDGE_CURVE ( 'NONE', #63778, #79604, #52334, .T. ) ;
#4533 = CARTESIAN_POINT ( 'NONE',  ( -108.9430120123302004, -286.2004018803217491, -253.3177627417776421 ) ) ;
#4534 = DIRECTION ( 'NONE',  ( 1.049727191138614998E-16, 0.5150380749100592626, -0.8571673007021092250 ) ) ;
#4535 = CARTESIAN_POINT ( 'NONE',  ( -37.29100371760605270, -286.8556005776840721, -197.1871922649171722 ) ) ;
#4536 = CARTESIAN_POINT ( 'NONE',  ( 16.30063956946690240, -294.7885894542404799, -217.3640803795730960 ) ) ;
#4537 = CARTESIAN_POINT ( 'NONE',  ( -79.44448346107091652, -275.6953074511906721, -333.1670029207481321 ) ) ;
#4538 = CARTESIAN_POINT ( 'NONE',  ( 10.51623328085961440, -276.7453061544791240, -330.7231549890655629 ) ) ;
#4539 = CARTESIAN_POINT ( 'NONE',  ( -19.69882036959028326, -290.3569827999576773, -196.8359410986647049 ) ) ;
#4540 = CARTESIAN_POINT ( 'NONE',  ( -113.2991671191070822, -278.3942231741314117, -282.9889922418026345 ) ) ;
#4541 = CARTESIAN_POINT ( 'NONE',  ( -78.84376550447035470, -297.5939536340089262, -332.4672736319399178 ) ) ;
#4542 = CARTESIAN_POINT ( 'NONE',  ( -48.18343439339133027, -249.2745803555438897, -480.5695237573682448 ) ) ;
#4543 = CARTESIAN_POINT ( 'NONE',  ( 209.8616357346614905, 36.89613957940296274, 15.00000000000000000 ) ) ;
#4544 = CARTESIAN_POINT ( 'NONE',  ( 2.729830342520385589, -285.2870244002904201, -208.7533593551256388 ) ) ;
#4545 = CARTESIAN_POINT ( 'NONE',  ( -105.4133529992866158, -276.2986472282068462, -300.1061580810805367 ) ) ;
#4546 = CARTESIAN_POINT ( 'NONE',  ( 5.754406211532351101, -280.4684074942066445, -331.8064174026715136 ) ) ;
#4547 = DIRECTION ( 'NONE',  ( 1.000000000000000000, 0.000000000000000000, 0.000000000000000000 ) ) ;
#4548 = CARTESIAN_POINT ( 'NONE',  ( 37.27156885159967459, -273.8295064046976108, -254.3127855910245501 ) ) ;
#4549 = CARTESIAN_POINT ( 'NONE',  ( -48.63175651213587258, -276.5481531940310447, -342.6374180482945349 ) ) ;
#4550 = CARTESIAN_POINT ( 'NONE',  ( 36.22549824357571424, -295.0054804273252103, -265.2491425634210032 ) ) ;
#4551 = CARTESIAN_POINT ( 'NONE',  ( -11.60010616948785156, -279.2998869186145043, -198.0636588701368623 ) ) ;
#4552 = CARTESIAN_POINT ( 'NONE',  ( -39.68459460023145624, -296.0235152069855644, -343.5713980076945404 ) ) ;
#4553 = CARTESIAN_POINT ( 'NONE',  ( -36.21040288203779056, -299.3812042098762731, -193.8540181952150192 ) ) ;
#4554 = CARTESIAN_POINT ( 'NONE',  ( -79.72632205034507535, -297.2943201316504087, -210.9259110005620812 ) ) ;
#4555 = CARTESIAN_POINT ( 'NONE',  ( -58.23589824656193059, -293.7824356898728979, -198.2760078724264474 ) ) ;
#4556 = CARTESIAN_POINT ( 'NONE',  ( -30.88596906252780983, -286.2982626311953709, -193.6189267934908003 ) ) ;
#4557 = CARTESIAN_POINT ( 'NONE',  ( 28.01822719600309242, -274.1986802453183714, -308.6806349260861566 ) ) ;
#4558 = CARTESIAN_POINT ( 'NONE',  ( -69.35924035416215361, -289.2952204175426232, -340.4032300449738386 ) ) ;
#4559 = CARTESIAN_POINT ( 'NONE',  ( -110.2179709872880267, -280.7411115577180567, -254.1502397022773607 ) ) ;
#4560 = CARTESIAN_POINT ( 'NONE',  ( 8.116651766637280829, -287.4714484460505446, -327.7801626488054580 ) ) ;
#4561 = CARTESIAN_POINT ( 'NONE',  ( -112.0129842500113142, -288.6489151959764285, -262.8122605209726430 ) ) ;
#4562 = ORIENTED_EDGE ( 'NONE', *, *, #31405, .F. ) ;
#4563 = CARTESIAN_POINT ( 'NONE',  ( -105.6472514815422983, -266.3687386123619376, -319.2208520127341558 ) ) ;
#4564 = CARTESIAN_POINT ( 'NONE',  ( -26.47192077230818796, -288.4178894023264093, -342.6606448618233003 ) ) ;
#4565 = DIRECTION ( 'NONE',  ( 0.000000000000000000, -0.000000000000000000, 1.000000000000000000 ) ) ;
#4566 = CARTESIAN_POINT ( 'NONE',  ( -66.47581498246137244, -284.3657095104144332, -341.3965489403619245 ) ) ;
#4567 = CARTESIAN_POINT ( 'NONE',  ( 35.23409891286262763, -292.2928483653100784, -245.1886690202075272 ) ) ;
#4568 = CARTESIAN_POINT ( 'NONE',  ( -17.22302613152774597, -281.9077621208018058, -196.8649999206666052 ) ) ;
#4569 = CARTESIAN_POINT ( 'NONE',  ( -38.18140300432223455, -281.3570027617740266, -193.8588750487726884 ) ) ;
#4570 = CARTESIAN_POINT ( 'NONE',  ( 35.13951695391511265, -281.5055051004177926, -279.4603423341849293 ) ) ;
#4571 = CARTESIAN_POINT ( 'NONE',  ( 26.97827236433429121, -277.0346737862777786, -231.6867313962381445 ) ) ;
#4572 = CARTESIAN_POINT ( 'NONE',  ( -89.60830321496932527, -297.3397075891438135, -213.7450823601406000 ) ) ;
#4573 = CARTESIAN_POINT ( 'NONE',  ( -110.3132991166835808, -288.7750131857864062, -254.6451214292655436 ) ) ;
#4574 = UNCERTAINTY_MEASURE_WITH_UNIT (LENGTH_MEASURE( 1.000000000000000082E-05 ), #34987, 'distance_accuracy_value', 'NONE');
#4575 = CARTESIAN_POINT ( 'NONE',  ( -106.6764805985710041, -271.6655836948855267, -246.2816927061899719 ) ) ;
#4576 = VERTEX_POINT ( 'NONE', #16358 ) ;
#4577 = CARTESIAN_POINT ( 'NONE',  ( -98.55372046247600792, -287.0512902252251024, -227.9781847445313474 ) ) ;
#4578 = CARTESIAN_POINT ( 'NONE',  ( -69.38618270091909324, -296.5436682635711350, -340.0507645811265434 ) ) ;
#4579 = CARTESIAN_POINT ( 'NONE',  ( -51.02886024927795461, -283.8829917290034928, -342.2219175641175184 ) ) ;
#4580 = CARTESIAN_POINT ( 'NONE',  ( -51.28168796317569900, -276.2849532974807403, -345.8495074969753205 ) ) ;
#4581 = CARTESIAN_POINT ( 'NONE',  ( -114.0866327045799977, -291.2643075570744031, -265.5105396513649225 ) ) ;
#4582 = CARTESIAN_POINT ( 'NONE',  ( -111.7800741921122523, -282.8745649293283577, -255.9735814802576783 ) ) ;
#4583 = AXIS2_PLACEMENT_3D ( 'NONE', #12243, #84664, #56773 ) ;
#4584 = CARTESIAN_POINT ( 'NONE',  ( 32.16504706785190137, -293.4598451725764789, -237.1531742276629871 ) ) ;
#4585 = CARTESIAN_POINT ( 'NONE',  ( -94.96463191180620811, -290.2534627175618880, -315.2331318636522610 ) ) ;
#4586 = CARTESIAN_POINT ( 'NONE',  ( 184.8920641257441844, 2.973978534295031118, 8.999830714574057922 ) ) ;
#4587 = CARTESIAN_POINT ( 'NONE',  ( 175.2296996224750103, 20.99999999999998934, 0.000000000000000000 ) ) ;
#4588 = CARTESIAN_POINT ( 'NONE',  ( 121.7894184752417601, 147.3656319919282964, -260.3019867207437983 ) ) ;
#4589 = AXIS2_PLACEMENT_3D ( 'NONE', #91344, #62022, #39737 ) ;
#4590 = CARTESIAN_POINT ( 'NONE',  ( -76.38633874452972350, -285.0840267372630592, -335.9832136526091517 ) ) ;
#4591 = CARTESIAN_POINT ( 'NONE',  ( -54.49178911615187104, -286.7666405000204009, -345.3538533559490702 ) ) ;
#4592 = ORIENTED_EDGE ( 'NONE', *, *, #28, .F. ) ;
#4593 = CARTESIAN_POINT ( 'NONE',  ( 36.01194568088035197, -280.4852213886582035, -271.3315130013310181 ) ) ;
#4594 = CARTESIAN_POINT ( 'NONE',  ( -62.40312021176868029, -277.0360426768332331, -343.2025032670061933 ) ) ;
#4595 = CARTESIAN_POINT ( 'NONE',  ( -94.50676637562121130, -281.2219457790112642, -222.0487110240886182 ) ) ;
#4596 = CARTESIAN_POINT ( 'NONE',  ( 123.4377129911925266, 147.5673827398361482, -261.9833486453449041 ) ) ;
#4597 = CARTESIAN_POINT ( 'NONE',  ( 35.04499807880887374, -280.4393464766956754, -294.9952549754937650 ) ) ;
#4598 = CARTESIAN_POINT ( 'NONE',  ( -106.1031036191608194, -282.9550969145678891, -241.1815773895232837 ) ) ;
#4599 = CARTESIAN_POINT ( 'NONE',  ( -3.987567352928275355, -300.2244201198217866, -194.3646069505561798 ) ) ;
#4600 = CARTESIAN_POINT ( 'NONE',  ( -4.303226799851355366, -295.0968185298930280, -335.5399021057482400 ) ) ;
#4601 = ORIENTED_EDGE ( 'NONE', *, *, #8722, .T. ) ;
#4602 = CARTESIAN_POINT ( 'NONE',  ( -67.99169109399944944, -290.3259492870271856, -203.5504249638108263 ) ) ;
#4603 = CARTESIAN_POINT ( 'NONE',  ( -17.37636037328670824, -277.4524591733365355, -344.6221305986123298 ) ) ;
#4604 = CARTESIAN_POINT ( 'NONE',  ( 25.27582940987185722, -275.0348354874549273, -232.7392820504886117 ) ) ;
#4605 = CARTESIAN_POINT ( 'NONE',  ( 33.89201201114089201, -274.8360130969343800, -298.9163875505229271 ) ) ;
#4606 = PLANE ( 'NONE',  #73366 ) ;
#4607 = CARTESIAN_POINT ( 'NONE',  ( -80.44399200687146845, -271.4683023672242825, -208.9211940534819121 ) ) ;
#4608 = CARTESIAN_POINT ( 'NONE',  ( 175.2296996224750103, 276.0000000000000568, 0.000000000000000000 ) ) ;
#4609 = CARTESIAN_POINT ( 'NONE',  ( 196.7383257810085979, 42.27872732282705925, 11.00000000000000000 ) ) ;
#4610 = CARTESIAN_POINT ( 'NONE',  ( 34.79206666094296452, -282.8045007752463107, -283.5061529161840213 ) ) ;
#4611 = CARTESIAN_POINT ( 'NONE',  ( 25.89123344371115465, -283.8742959451880097, -312.4986324492521703 ) ) ;
#4612 = CARTESIAN_POINT ( 'NONE',  ( -109.9750105505696638, -283.7861129506249540, -279.0622644067480564 ) ) ;
#4613 = CARTESIAN_POINT ( 'NONE',  ( 24.64538066923214288, -274.5016016829282535, -310.5058020067859275 ) ) ;
#4614 = CARTESIAN_POINT ( 'NONE',  ( 22.82676018172396581, -284.0109317930480870, -313.8641736651790666 ) ) ;
#4615 = CARTESIAN_POINT ( 'NONE',  ( -46.00867426013731887, -275.6437788181847850, -343.5941307776746498 ) ) ;
#4616 = DIRECTION ( 'NONE',  ( -0.000000000000000000, -1.000000000000000000, -0.000000000000000000 ) ) ;
#4617 = CARTESIAN_POINT ( 'NONE',  ( -3.976223985848467368, -275.5826136997434332, -205.0709126687969501 ) ) ;
#4618 = DIRECTION ( 'NONE',  ( -1.000000000000000000, 0.000000000000000000, 0.000000000000000000 ) ) ;
#4619 = CARTESIAN_POINT ( 'NONE',  ( -41.01093377548058072, -280.8099413262089001, -193.5970834523247390 ) ) ;
#4620 = VERTEX_POINT ( 'NONE', #31045 ) ;
#4621 = ORIENTED_EDGE ( 'NONE', *, *, #37438, .F. ) ;
#4622 = DIRECTION ( 'NONE',  ( -0.000000000000000000, -1.000000000000000000, -0.000000000000000000 ) ) ;
#4623 = CARTESIAN_POINT ( 'NONE',  ( -110.5342538430796253, -286.6639124639017382, -250.5893364286434633 ) ) ;
#4624 = CARTESIAN_POINT ( 'NONE',  ( -28.88744741633575330, -294.1395400012453933, -343.0836092450228989 ) ) ;
#4625 = CARTESIAN_POINT ( 'NONE',  ( -109.7723447150396510, -289.5725216538727409, -296.3475900868487543 ) ) ;
#4626 = EDGE_CURVE ( 'NONE', #41151, #90952, #49009, .T. ) ;
#4627 = CARTESIAN_POINT ( 'NONE',  ( 11.82370490451610578, -284.9856325003853499, -214.9683122456135322 ) ) ;
#4629 = CARTESIAN_POINT ( 'NONE',  ( -109.4090960094531084, -289.0120973177457699, -253.4457738176095347 ) ) ;
#4628 = CARTESIAN_POINT ( 'NONE',  ( 11.53889236592828027, -285.3204475261889570, -215.2829788251914067 ) ) ;
#4630 = CARTESIAN_POINT ( 'NONE',  ( -102.5983984975132586, -286.2114585151029473, -236.7650792044286163 ) ) ;
#4631 = CARTESIAN_POINT ( 'NONE',  ( 36.75567406075547439, -273.7051210505691756, -282.2872240046474985 ) ) ;
#4632 = CARTESIAN_POINT ( 'NONE',  ( -1.329459978771967643, -284.9215743562727425, -203.2078680525330867 ) ) ;
#4633 = CARTESIAN_POINT ( 'NONE',  ( -34.17880835822248287, -300.0919018263072644, -195.3600309377237920 ) ) ;
#4634 = CARTESIAN_POINT ( 'NONE',  ( 35.93817630864670321, -285.3369260564052183, -253.5680727324181589 ) ) ;
#4635 = CARTESIAN_POINT ( 'NONE',  ( -4.251946925675381905, -281.4406959398218646, -205.0136029960060284 ) ) ;
#4636 = CARTESIAN_POINT ( 'NONE',  ( -5.095886315687366164, -290.6288725320699768, -338.2739735961027350 ) ) ;
#4637 = LINE ( 'NONE', #33511, #61063 ) ;
#4638 = CARTESIAN_POINT ( 'NONE',  ( 195.4412442344684848, 39.86655514736339967, 13.94770545599002354 ) ) ;
#4639 = CARTESIAN_POINT ( 'NONE',  ( -73.88802776502943459, -297.4533385869179938, -336.5535102211179606 ) ) ;
#4640 = CARTESIAN_POINT ( 'NONE',  ( -102.5381542272229751, -277.0462243174715127, -233.2879063699319317 ) ) ;
#4641 = CARTESIAN_POINT ( 'NONE',  ( -33.53711398094534957, -291.2960718897893457, -193.6168416813030149 ) ) ;
#4642 = CARTESIAN_POINT ( 'NONE',  ( -86.61949574754180503, -295.7533906512398403, -215.4235236385858059 ) ) ;
#4643 = CARTESIAN_POINT ( 'NONE',  ( 20.07169716844475360, -279.5931799692712616, -224.4814352175958447 ) ) ;
#4644 = CARTESIAN_POINT ( 'NONE',  ( -40.81819004538845519, -272.0880624479161725, -195.9516555355553749 ) ) ;
#4645 = CARTESIAN_POINT ( 'NONE',  ( 26.65580675681370693, -294.3748127827618077, -234.1246795753736194 ) ) ;
#4646 = CARTESIAN_POINT ( 'NONE',  ( -95.99890600148557951, -293.6948066931273615, -223.6242672951989618 ) ) ;
#4647 = CARTESIAN_POINT ( 'NONE',  ( -107.7429233821329291, -294.6527196711982128, -299.9322141047771311 ) ) ;
#4648 = CARTESIAN_POINT ( 'NONE',  ( -39.10706366233343090, -293.3138862350286331, -346.3272782651158082 ) ) ;
#4649 = EDGE_CURVE ( 'NONE', #11243, #34447, #37650, .T. ) ;
#4650 = CARTESIAN_POINT ( 'NONE',  ( -94.55099831294803892, -291.3279414469306516, -316.6479532626935907 ) ) ;
#4651 = DIRECTION ( 'NONE',  ( 0.8620390091940283162, 0.000000000000000000, -0.5068419345592647396 ) ) ;
#4652 = CARTESIAN_POINT ( 'NONE',  ( -81.83533469017216078, -292.2313995384226928, -212.2201737899346199 ) ) ;
#4653 = DIRECTION ( 'NONE',  ( 0.000000000000000000, 1.000000000000000000, 0.000000000000000000 ) ) ;
#4655 = CARTESIAN_POINT ( 'NONE',  ( 35.20692541208019577, -293.6649332262791745, -278.9105385297491466 ) ) ;
#4654 = CARTESIAN_POINT ( 'NONE',  ( 0.03024653560056232010, -280.5775013590695721, -335.8110618514120347 ) ) ;
#4656 = CARTESIAN_POINT ( 'NONE',  ( 19.16016125881708021, -280.8395701745132556, -218.0491723122284498 ) ) ;
#4657 = CIRCLE ( 'NONE', #63638, 7.500000000000012434 ) ;
#4658 = CARTESIAN_POINT ( 'NONE',  ( -97.15864897314560267, -283.5686332918953667, -318.8346656861278348 ) ) ;
#4659 = CARTESIAN_POINT ( 'NONE',  ( -23.46969991109115838, -286.8743885574860428, -343.9504703888119366 ) ) ;
#4660 = CARTESIAN_POINT ( 'NONE',  ( -98.56424538953238823, -282.1160091610662448, -312.4348571509264048 ) ) ;
#4661 = CARTESIAN_POINT ( 'NONE',  ( 169.2494399300530290, -11.64849832608277325, 9.974999999999996092 ) ) ;
#4662 = CARTESIAN_POINT ( 'NONE',  ( 16.74545725553502606, -279.2844388542310412, -216.4605519834392169 ) ) ;
#4663 = CARTESIAN_POINT ( 'NONE',  ( -40.78875968947717467, -284.9302148697245229, -193.6957519755633825 ) ) ;
#4664 = CARTESIAN_POINT ( 'NONE',  ( 195.0811277904324470, 39.36132622696000283, 15.19607843137254832 ) ) ;
#4665 = CARTESIAN_POINT ( 'NONE',  ( 33.52401861852879961, -295.4223969751753884, -291.0097463781291367 ) ) ;
#4666 = CARTESIAN_POINT ( 'NONE',  ( -23.03131561166794583, -278.2979531165901221, -345.4736618230061822 ) ) ;
#4667 = CARTESIAN_POINT ( 'NONE',  ( -95.29238934966666363, -277.5940112745445276, -314.7886444228770415 ) ) ;
#4668 = CARTESIAN_POINT ( 'NONE',  ( -112.8675802045441969, -290.5304660515217847, -285.4226547636037026 ) ) ;
#4669 = CARTESIAN_POINT ( 'NONE',  ( 6.077178295763310700, -280.5484010394340544, -332.2645156247864406 ) ) ;
#4670 = CARTESIAN_POINT ( 'NONE',  ( 35.85688529438362337, -292.5804076283258723, -268.0425969958330370 ) ) ;
#4671 = CARTESIAN_POINT ( 'NONE',  ( -106.5398738202464983, -294.1727584096531132, -299.4199111992413691 ) ) ;
#4672 = ORIENTED_EDGE ( 'NONE', *, *, #28909, .T. ) ;
#4673 = CARTESIAN_POINT ( 'NONE',  ( -26.20420625952874261, -294.4141798106948045, -342.5687676593620381 ) ) ;
#4674 = CARTESIAN_POINT ( 'NONE',  ( 207.9682738430187214, 0.04008605884692675175, -7.489252814170929362 ) ) ;
#4675 = CARTESIAN_POINT ( 'NONE',  ( -6.941161984400256557, -283.9809262143061233, -207.3071070584150277 ) ) ;
#4676 = CARTESIAN_POINT ( 'NONE',  ( -104.0841914154499790, -272.2460806622759719, -232.1807672738869144 ) ) ;
#4677 = CARTESIAN_POINT ( 'NONE',  ( 0.7734125911568857648, -278.6939772016694405, -204.8220396975919186 ) ) ;
#4678 = CARTESIAN_POINT ( 'NONE',  ( -10.18477647504847283, -287.7143726996027340, -198.7798669876611086 ) ) ;
#4679 = CARTESIAN_POINT ( 'NONE',  ( -0.9932859839907813848, -288.3889003757029741, -333.7264328488492993 ) ) ;
#4680 = CARTESIAN_POINT ( 'NONE',  ( -98.21069622439456737, -279.4997387556539934, -311.9023392816845330 ) ) ;
#4681 = CARTESIAN_POINT ( 'NONE',  ( -111.8855327853735702, -294.5221831127911400, -274.2423307797836856 ) ) ;
#4682 = CARTESIAN_POINT ( 'NONE',  ( -111.1071850747128451, -298.2257558864490079, -277.0127101735137103 ) ) ;
#4683 = CARTESIAN_POINT ( 'NONE',  ( -110.3004818743221733, -277.2360821265341428, -278.8204235032721385 ) ) ;
#4684 = ORIENTED_EDGE ( 'NONE', *, *, #1783, .F. ) ;
#4685 = CARTESIAN_POINT ( 'NONE',  ( -62.83404288312284791, -297.3958719303138878, -197.7258321199578290 ) ) ;
#4686 = CARTESIAN_POINT ( 'NONE',  ( -98.51867147455267570, -291.8925429663333944, -312.7944959491256327 ) ) ;
#4687 = CARTESIAN_POINT ( 'NONE',  ( 1.380638594652329854, -296.1439354805377207, -335.9890152450253140 ) ) ;
#4688 = CARTESIAN_POINT ( 'NONE',  ( -113.3111558597828576, -274.3094957117917829, -270.3834931753972910 ) ) ;
#4689 = CARTESIAN_POINT ( 'NONE',  ( -58.71101569970753786, -289.9872201842382538, -340.3228271646576104 ) ) ;
#4690 = CARTESIAN_POINT ( 'NONE',  ( -48.18343439339135159, -250.7819852860406229, -452.8786885270839093 ) ) ;
#4691 = ORIENTED_EDGE ( 'NONE', *, *, #85740, .T. ) ;
#4692 = CARTESIAN_POINT ( 'NONE',  ( -114.2640200941087016, -297.1770886592582315, -272.4752790926569901 ) ) ;
#4693 = CARTESIAN_POINT ( 'NONE',  ( -113.0186961824049376, -288.6453862187887012, -274.0077254815403194 ) ) ;
#4694 = CARTESIAN_POINT ( 'NONE',  ( -62.84204564026332918, -298.0623268394326715, -197.7286412917449638 ) ) ;
#4695 = CARTESIAN_POINT ( 'NONE',  ( -57.23711263161519724, -282.8906705383787994, 47.50000000000000000 ) ) ;
#4696 = DIRECTION ( 'NONE',  ( -1.000000000000000000, -0.000000000000000000, -0.000000000000000000 ) ) ;
#4697 = CARTESIAN_POINT ( 'NONE',  ( -41.70142007710229848, -290.6262233335039014, -346.5562439460481983 ) ) ;
#4698 = CARTESIAN_POINT ( 'NONE',  ( 36.57525178469696669, -277.6233781216988064, -234.7283546768995564 ) ) ;
#4699 = CARTESIAN_POINT ( 'NONE',  ( 30.63559147151739026, -280.4346265870901789, -234.2975993593122155 ) ) ;
#4700 = CARTESIAN_POINT ( 'NONE',  ( -110.1551400786540711, -286.7751970328142193, -253.0364720606785909 ) ) ;
#4701 = CARTESIAN_POINT ( 'NONE',  ( -3.732033264719329946, -285.0616457423262204, -201.7245701883663287 ) ) ;
#4702 = CARTESIAN_POINT ( 'NONE',  ( -32.54879122782131162, -272.1125250118368513, -195.6685848506718060 ) ) ;
#4703 = CARTESIAN_POINT ( 'NONE',  ( -40.86714032344767134, -275.9277501725102866, -195.9539622819045235 ) ) ;
#4704 = CARTESIAN_POINT ( 'NONE',  ( -108.3326535388154923, -288.3388626676915578, -292.9281880220445942 ) ) ;
#4705 = CARTESIAN_POINT ( 'NONE',  ( -59.28427648553832086, -279.1936555258983503, -342.8789007752742464 ) ) ;
#4706 = ORIENTED_EDGE ( 'NONE', *, *, #999, .T. ) ;
#4708 = CARTESIAN_POINT ( 'NONE',  ( 35.62210993554892013, -280.8415650315028529, -265.8694491492755674 ) ) ;
#4707 = CARTESIAN_POINT ( 'NONE',  ( 4.923154784574807152, -280.6413668813862046, -210.8406841869959862 ) ) ;
#4709 = CARTESIAN_POINT ( 'NONE',  ( -4.116277169682523329, -277.7039592856522745, -339.4954832554731752 ) ) ;
#4710 = CARTESIAN_POINT ( 'NONE',  ( 31.67044634921600021, -279.9169872171020188, -236.9924942324666404 ) ) ;
#4711 = CARTESIAN_POINT ( 'NONE',  ( 172.0061749996893354, 242.1526343824411072, -177.7416445279219772 ) ) ;
#4712 = CARTESIAN_POINT ( 'NONE',  ( 38.50518149417412417, -276.6460587157657756, -282.5302153825796267 ) ) ;
#4713 = EDGE_CURVE ( 'NONE', #49742, #87677, #73147, .T. ) ;
#4714 = CARTESIAN_POINT ( 'NONE',  ( -105.0032030312531504, -274.5327892572519772, -234.9675638856268165 ) ) ;
#4715 = CARTESIAN_POINT ( 'NONE',  ( -6.941161984400275209, -279.1233781216987495, -333.4151289067050357 ) ) ;
#4716 = EDGE_LOOP ( 'NONE', ( #87629, #16247, #76327, #79717 ) ) ;
#4717 = CARTESIAN_POINT ( 'NONE',  ( 165.7865175155837676, 3.000000000000000000, 9.000000000000001776 ) ) ;
#4718 = AXIS2_PLACEMENT_3D ( 'NONE', #30902, #45071, #24716 ) ;
#4719 = CARTESIAN_POINT ( 'NONE',  ( 34.00508519049079581, -288.8531565856383736, -287.2093315194344427 ) ) ;
#4720 = CARTESIAN_POINT ( 'NONE',  ( 33.89633579638270078, -288.9735314842162097, -243.9203114543053630 ) ) ;
#4721 = CARTESIAN_POINT ( 'NONE',  ( -84.75744235378564895, -289.0744099093689101, -326.0664147626069962 ) ) ;
#4722 = CARTESIAN_POINT ( 'NONE',  ( -20.99092746370978801, -285.7642222696639465, -195.1801420888355096 ) ) ;
#4723 = CARTESIAN_POINT ( 'NONE',  ( -62.48528110653271739, -183.4704917803509829, -362.4204795493197366 ) ) ;
#4724 = CARTESIAN_POINT ( 'NONE',  ( 34.42335972128890376, -280.1773038927441917, -287.6257651022099822 ) ) ;
#4725 = CARTESIAN_POINT ( 'NONE',  ( 34.90707358132212335, -289.1905743615654956, -253.2481120857285077 ) ) ;
#4726 = CARTESIAN_POINT ( 'NONE',  ( -4.535737291793926040, -281.0916447503937547, -336.3495757375241624 ) ) ;
#4727 = CARTESIAN_POINT ( 'NONE',  ( -67.52402796698864051, -280.9628967905017589, -203.3379368807701155 ) ) ;
#4728 = CARTESIAN_POINT ( 'NONE',  ( -45.90909642145814473, -277.6559237010195034, -342.9692679963890782 ) ) ;
#4729 = CARTESIAN_POINT ( 'NONE',  ( -109.4967426273986746, -289.0189483437380318, -296.2411898321437889 ) ) ;
#4730 = CARTESIAN_POINT ( 'NONE',  ( -112.0597234316401511, -285.1296096367069026, -288.3437432660147692 ) ) ;
#4731 = CARTESIAN_POINT ( 'NONE',  ( -114.0909617899771575, -285.1208700617415275, -264.2593677967915369 ) ) ;
#4732 = CARTESIAN_POINT ( 'NONE',  ( 26.85605756591158411, -282.1929873405071589, -305.1123469039780502 ) ) ;
#4733 = ORIENTED_EDGE ( 'NONE', *, *, #61391, .F. ) ;
#4734 = DIRECTION ( 'NONE',  ( -0.000000000000000000, 1.000000000000000000, -0.000000000000000000 ) ) ;
#4735 = CARTESIAN_POINT ( 'NONE',  ( -109.5965772592458620, -292.1194841406426121, -293.3257201945652355 ) ) ;
#4736 = CARTESIAN_POINT ( 'NONE',  ( 20.02012098263473305, -291.5468765720261786, -219.7160324225135639 ) ) ;
#4737 = CARTESIAN_POINT ( 'NONE',  ( 33.74044315437132013, -274.3790307910541628, -252.7333740770584711 ) ) ;
#4738 = CARTESIAN_POINT ( 'NONE',  ( -103.0328220945177407, -295.3780743163102898, -310.3359760959696132 ) ) ;
#4739 = CARTESIAN_POINT ( 'NONE',  ( -4.506929531580985859, -290.9727079686190905, -204.3729313823540679 ) ) ;
#4740 = CARTESIAN_POINT ( 'NONE',  ( -50.67546114282041003, -293.4646461627337430, -343.1634862706560511 ) ) ;
#4741 = CARTESIAN_POINT ( 'NONE',  ( -109.5669331250463614, -291.5858390791577222, -283.4242808501812760 ) ) ;
#4742 = DIRECTION ( 'NONE',  ( 1.000000000000000000, 0.000000000000000000, 0.000000000000000000 ) ) ;
#4743 = CARTESIAN_POINT ( 'NONE',  ( -106.9329693694158578, -292.1879274377781712, -298.3263802150158881 ) ) ;
#4744 = CARTESIAN_POINT ( 'NONE',  ( -30.83008176695459923, -290.1339811200797953, -195.4255237265460039 ) ) ;
#4745 = CARTESIAN_POINT ( 'NONE',  ( 37.05095200606859152, -295.4249422599753530, -260.4410809049220461 ) ) ;
#4746 = CARTESIAN_POINT ( 'NONE',  ( -57.47052722810708758, -286.7272679176734869, -199.8935698004119104 ) ) ;
#4747 = CARTESIAN_POINT ( 'NONE',  ( -19.69243258534993757, -296.8260355621781059, -343.4799579227356503 ) ) ;
#4748 = CARTESIAN_POINT ( 'NONE',  ( -24.46599358326421481, -276.1954652938281924, -196.0610714254875973 ) ) ;
#4749 = CARTESIAN_POINT ( 'NONE',  ( 22.32202329137529873, -274.9945508533119209, -318.4260988948511226 ) ) ;
#4750 = CARTESIAN_POINT ( 'NONE',  ( 53.36098360292933762, -298.3578056523604687, -193.5345460460098650 ) ) ;
#4751 = CARTESIAN_POINT ( 'NONE',  ( -5.865760172917629411, -274.8724399112180663, -337.3619337298343908 ) ) ;
#4752 = CARTESIAN_POINT ( 'NONE',  ( 18.15231950314754528, -278.9359384421925370, -220.7453142062751965 ) ) ;
#4753 = CARTESIAN_POINT ( 'NONE',  ( -110.7387727487133446, -273.7570339776519859, -270.3764257432318345 ) ) ;
#4754 = CARTESIAN_POINT ( 'NONE',  ( -27.05771434395720831, -272.7550404801909281, -194.5925365816114549 ) ) ;
#4755 = CARTESIAN_POINT ( 'NONE',  ( -105.5008819928261232, -297.6087568374248349, -298.1046008810332637 ) ) ;
#4756 = FACE_OUTER_BOUND ( 'NONE', #53050, .T. ) ;
#4757 = CARTESIAN_POINT ( 'NONE',  ( -94.58404058921487945, -297.9969704448878360, -224.7988947476130477 ) ) ;
#4758 = CARTESIAN_POINT ( 'NONE',  ( 196.1963538710216994, 282.2246705312485915, -40.00000000000000711 ) ) ;
#4760 = CARTESIAN_POINT ( 'NONE',  ( -102.0294619080500524, -272.8471769016366579, -236.4212762380294635 ) ) ;
#4759 = CARTESIAN_POINT ( 'NONE',  ( -3.815661055587151740, -286.6322703723892005, -337.8618123248742791 ) ) ;
#4761 = CARTESIAN_POINT ( 'NONE',  ( 25.54510566533832971, -286.9639087269663378, -225.9058560106946629 ) ) ;
#4762 = CARTESIAN_POINT ( 'NONE',  ( -60.02509543646795720, -289.0050368228770026, -343.9220306246539280 ) ) ;
#4763 = CARTESIAN_POINT ( 'NONE',  ( -109.6302365437836812, -298.2587740187327086, -291.6850719994691872 ) ) ;
#4764 = CARTESIAN_POINT ( 'NONE',  ( 31.15825626278251548, -291.9474178855201671, -300.4905786151506391 ) ) ;
#4765 = CARTESIAN_POINT ( 'NONE',  ( 36.32093819717986349, -281.0262658275285048, -292.4067044790296563 ) ) ;
#4766 = DIRECTION ( 'NONE',  ( 0.000000000000000000, 0.000000000000000000, 1.000000000000000000 ) ) ;
#4767 = CARTESIAN_POINT ( 'NONE',  ( -104.6370817574469498, -276.1139376130111600, -303.5881779673679830 ) ) ;
#4768 = FACE_OUTER_BOUND ( 'NONE', #90044, .T. ) ;
#4769 = CARTESIAN_POINT ( 'NONE',  ( -37.28302428000554158, -287.8463238919713945, -343.7581687639628285 ) ) ;
#4770 = EDGE_CURVE ( 'NONE', #55951, #76475, #59935, .T. ) ;
#4771 = DIRECTION ( 'NONE',  ( 1.000000000000000000, 0.000000000000000000, 0.000000000000000000 ) ) ;
#4772 = CARTESIAN_POINT ( 'NONE',  ( -69.64177404394288828, -287.4772168803207251, -338.0494174040621260 ) ) ;
#4773 = CARTESIAN_POINT ( 'NONE',  ( -50.11216171078302750, -299.4865958640592680, -197.6744223341751479 ) ) ;
#4774 = CARTESIAN_POINT ( 'NONE',  ( 21.17060116043438356, -283.6441664382444969, -319.5029219026433225 ) ) ;
#4776 = CARTESIAN_POINT ( 'NONE',  ( -40.23435849278468623, -283.0895227110742098, -343.3037840127039431 ) ) ;
#4775 = CARTESIAN_POINT ( 'NONE',  ( -100.0004653762155868, -271.2000396087570948, -228.0401388598519077 ) ) ;
#4777 = CARTESIAN_POINT ( 'NONE',  ( 9.849144460514617450, -276.1418520665376946, -213.8284904838072862 ) ) ;
#4778 = ADVANCED_FACE ( 'NONE', ( #9230 ), #25439, .F. ) ;
#4779 = CARTESIAN_POINT ( 'NONE',  ( 27.54323223260126241, -283.0500678251806903, -232.7453473655083087 ) ) ;
#4780 = CARTESIAN_POINT ( 'NONE',  ( -56.93104289254733175, -272.7139623974682650, -199.6648252726962767 ) ) ;
#4781 = AXIS2_PLACEMENT_3D ( 'NONE', #7869, #18135, #67044 ) ;
#4782 = ORIENTED_EDGE ( 'NONE', *, *, #13516, .T. ) ;
#4783 = CARTESIAN_POINT ( 'NONE',  ( 203.6182477417019356, 295.8614695731350821, -54.00000000006011902 ) ) ;
#4784 = CARTESIAN_POINT ( 'NONE',  ( 36.70474744800839062, -293.1201637223051080, -249.1914313631092739 ) ) ;
#4785 = CARTESIAN_POINT ( 'NONE',  ( -111.9619450001418244, -286.4884964043978925, -273.7371169228075587 ) ) ;
#4786 = DIRECTION ( 'NONE',  ( -0.000000000000000000, -1.000000000000000000, -0.000000000000000000 ) ) ;
#4787 = CARTESIAN_POINT ( 'NONE',  ( -115.3288506153726871, -276.2666405000204009, -252.5284128619063608 ) ) ;
#4788 = CARTESIAN_POINT ( 'NONE',  ( -114.2234999861203590, -277.7338498405199516, -271.5955770909419584 ) ) ;
#4789 = CARTESIAN_POINT ( 'NONE',  ( -72.81966113325424317, -287.9139445196076394, -337.8127652717201954 ) ) ;
#4790 = AXIS2_PLACEMENT_3D ( 'NONE', #49606, #85120, #20272 ) ;
#4791 = CARTESIAN_POINT ( 'NONE',  ( -93.07087735107516835, -285.3914876462631582, -318.5982219497129222 ) ) ;
#4793 = CARTESIAN_POINT ( 'NONE',  ( -97.69925530789522838, -279.7220536453020259, -313.2193144267465073 ) ) ;
#4792 = PRODUCT_RELATED_PRODUCT_CATEGORY ( 'part', '', ( #64119 ) ) ;
#4794 = CARTESIAN_POINT ( 'NONE',  ( -71.45923539320028794, -284.9192038175204402, -338.7321650897167729 ) ) ;
#4795 = CARTESIAN_POINT ( 'NONE',  ( -32.13275347443686059, -281.7799021204014593, -343.5731209595419386 ) ) ;
#4796 = CARTESIAN_POINT ( 'NONE',  ( -7.218923341825066231, -282.4473899130564973, -201.6621481302328505 ) ) ;
#4797 = CARTESIAN_POINT ( 'NONE',  ( 16.02550869841847714, -274.9506917812724396, -214.8548928671532110 ) ) ;
#4798 = CARTESIAN_POINT ( 'NONE',  ( -17.35994470371500853, -276.6344976110535754, -344.7232686685538852 ) ) ;
#4799 = CARTESIAN_POINT ( 'NONE',  ( -6.139478730825269182, -296.5590464803067334, -337.9461428114860837 ) ) ;
#4800 = CARTESIAN_POINT ( 'NONE',  ( -23.68628624284178130, -55.96374926131388605, -21.50000000000000000 ) ) ;
#4801 = DIRECTION ( 'NONE',  ( 0.000000000000000000, 1.000000000000000000, 0.000000000000000000 ) ) ;
#4802 = CARTESIAN_POINT ( 'NONE',  ( -69.03319148580604292, -293.6040565877264612, -339.1935961930356029 ) ) ;
#4803 = CARTESIAN_POINT ( 'NONE',  ( 34.18287681988810078, -274.8625136281199275, -255.3928601204138999 ) ) ;
#4804 = CARTESIAN_POINT ( 'NONE',  ( -85.03497123102626176, -298.4909342040351135, -210.3041083969167460 ) ) ;
#4805 = CARTESIAN_POINT ( 'NONE',  ( 21.12757724937024051, -288.6818328797277786, -224.9814130557638521 ) ) ;
#4806 = CARTESIAN_POINT ( 'NONE',  ( 36.03210093131030334, -294.8066932907680666, -249.3613887885495899 ) ) ;
#4807 = CARTESIAN_POINT ( 'NONE',  ( 39.04396412927923876, -294.6847487297396810, -264.5957893989631771 ) ) ;
#4808 = CARTESIAN_POINT ( 'NONE',  ( -110.4484133573006517, -292.3459322630665156, -286.4029862868962368 ) ) ;
#4809 = CARTESIAN_POINT ( 'NONE',  ( -24.53829087852558999, -278.2157762149737437, -196.6311977641455542 ) ) ;
#4810 = CARTESIAN_POINT ( 'NONE',  ( -69.16056666271923348, -281.5504392788729433, -203.0642091813285788 ) ) ;
#4811 = CARTESIAN_POINT ( 'NONE',  ( -34.50117269507498463, -284.8772145006497567, -346.0726553238088741 ) ) ;
#4812 = CARTESIAN_POINT ( 'NONE',  ( -19.72833028419634616, -285.2043201651664504, -199.1993636801954892 ) ) ;
#4813 = CARTESIAN_POINT ( 'NONE',  ( 86.44575683232005758, 81.85753257257081827, -301.4767831277452501 ) ) ;
#4814 = VERTEX_POINT ( 'NONE', #75409 ) ;
#4815 = CARTESIAN_POINT ( 'NONE',  ( -109.4413297541693595, -284.3724205562562020, -258.7177366062745136 ) ) ;
#4816 = EDGE_LOOP ( 'NONE', ( #42290, #11420, #12767, #2855, #7733 ) ) ;
#4817 = CARTESIAN_POINT ( 'NONE',  ( 21.38222218702756194, -283.2986214375645773, -319.6865014955888569 ) ) ;
#4818 = CARTESIAN_POINT ( 'NONE',  ( -64.58061434928194444, -274.0197913115372899, -202.5971427892014844 ) ) ;
#4819 = CARTESIAN_POINT ( 'NONE',  ( -57.63588892406294661, -284.5908492520185291, -196.4402669667841508 ) ) ;
#4820 = CARTESIAN_POINT ( 'NONE',  ( -45.26105567974459376, -280.8955505605646294, -193.9531714973741998 ) ) ;
#4821 = CARTESIAN_POINT ( 'NONE',  ( -105.5644583403313419, -280.5172715435263058, -236.0620520223841936 ) ) ;
#4822 = CARTESIAN_POINT ( 'NONE',  ( -6.279157895928174860, -281.1010252308510076, -200.0017785381950546 ) ) ;
#4823 = CARTESIAN_POINT ( 'NONE',  ( -37.37352853689063181, -280.5523547857346784, -340.3611179825599606 ) ) ;
#4824 = CARTESIAN_POINT ( 'NONE',  ( 65.82139847730509530, 47.41426247659997273, -318.9771648146296457 ) ) ;
#4825 = VERTEX_POINT ( 'NONE', #46506 ) ;
#4826 = CARTESIAN_POINT ( 'NONE',  ( -79.91857489696971584, -275.4753622649810723, -208.7576189306324466 ) ) ;
#4827 = CARTESIAN_POINT ( 'NONE',  ( 179.3423712301919579, 254.3167496676224744, -166.5185575139265666 ) ) ;
#4828 = CARTESIAN_POINT ( 'NONE',  ( -88.64315556899686044, -277.3486660267244588, -216.0678736075912525 ) ) ;
#4829 = CARTESIAN_POINT ( 'NONE',  ( 16.75226959300215768, -294.5688739103903231, -216.9221133745738257 ) ) ;
#4830 = CARTESIAN_POINT ( 'NONE',  ( -108.4000593501074690, -295.6739364221820097, -287.5779105873440358 ) ) ;
#4831 = CARTESIAN_POINT ( 'NONE',  ( -99.15140905067138988, -290.6696191897650010, -224.5232583887171813 ) ) ;
#4832 = CARTESIAN_POINT ( 'NONE',  ( 165.4421947725420523, 276.0000000000000568, 22.46007009812166544 ) ) ;
#4833 = EDGE_CURVE ( 'NONE', #43507, #93231, #73286, .T. ) ;
#4835 = CARTESIAN_POINT ( 'NONE',  ( 35.91590325600594724, -286.0685564630210820, -279.2921851719104893 ) ) ;
#4834 = CARTESIAN_POINT ( 'NONE',  ( -110.2431222966178979, -294.8365315187070337, -293.2957511565517734 ) ) ;
#4836 = CARTESIAN_POINT ( 'NONE',  ( 9.612090873140548553, -294.5660433463754089, -212.7948340075635372 ) ) ;
#4837 = ADVANCED_FACE ( 'NONE', ( #90061 ), #74766, .T. ) ;
#4838 = CARTESIAN_POINT ( 'NONE',  ( -99.43881027987846721, -285.3266107964624894, -309.7652917306182871 ) ) ;
#4839 = ORIENTED_EDGE ( 'NONE', *, *, #80738, .T. ) ;
#4840 = CARTESIAN_POINT ( 'NONE',  ( -98.16919230591311418, -292.1203836765540700, -223.5121124017161378 ) ) ;
#4841 = CARTESIAN_POINT ( 'NONE',  ( -8.464153608215625013, -283.1559737728903769, -337.4735292697905606 ) ) ;
#4842 = CARTESIAN_POINT ( 'NONE',  ( -112.2091346281442412, -295.5516251887492558, -254.0865016796416285 ) ) ;
#4843 = CARTESIAN_POINT ( 'NONE',  ( -75.57444452775595778, -290.3516462975356944, -337.0125701513002241 ) ) ;
#4844 = CARTESIAN_POINT ( 'NONE',  ( -66.99752152933037053, -292.1660619823408069, -199.3677439231391020 ) ) ;
#4845 = CARTESIAN_POINT ( 'NONE',  ( 33.70982118210871192, -287.4971128931756539, -253.5535546370061297 ) ) ;
#4846 = ORIENTED_EDGE ( 'NONE', *, *, #37797, .T. ) ;
#4847 = CARTESIAN_POINT ( 'NONE',  ( 184.7149167944524493, -12.49482340714361506, -3.999999999999998224 ) ) ;
#4848 = CARTESIAN_POINT ( 'NONE',  ( -112.4252009086281134, -298.2788406506198271, -280.8821943108006849 ) ) ;
#4849 = CARTESIAN_POINT ( 'NONE',  ( -31.93592802908120376, -296.8033309403293742, -193.8554441496146694 ) ) ;
#4850 = CARTESIAN_POINT ( 'NONE',  ( 15.43724516592988927, -279.8795028648297603, -219.5167046605941437 ) ) ;
#4851 = ORIENTED_EDGE ( 'NONE', *, *, #36821, .T. ) ;
#4852 = CARTESIAN_POINT ( 'NONE',  ( -18.55892191033718319, -273.7953345295165946, -195.6955810522516686 ) ) ;
#4853 = CARTESIAN_POINT ( 'NONE',  ( -92.34965465860433653, -295.7267187377690902, -221.3220244783978217 ) ) ;
#4854 = CARTESIAN_POINT ( 'NONE',  ( -4.498637119073520374, -278.4751869823304560, -336.9500054205054198 ) ) ;
#4855 = CARTESIAN_POINT ( 'NONE',  ( 1.274900704134463769, -272.7134559620038203, -206.9606162493793988 ) ) ;
#4856 = VECTOR ( 'NONE', #8693, 1000.000000000000000 ) ;
#4857 = CARTESIAN_POINT ( 'NONE',  ( 10.56221645920129859, -295.5778869349519482, -325.9699777021423301 ) ) ;
#4858 = CARTESIAN_POINT ( 'NONE',  ( -102.8145700360186083, -298.0788727304875465, -237.2703378846572093 ) ) ;
#4859 = CARTESIAN_POINT ( 'NONE',  ( 202.9738562182569694, 293.9636489450776367, -44.00000000000000000 ) ) ;
#4860 = CARTESIAN_POINT ( 'NONE',  ( -1.068852149940670682, -296.1791649933183521, -337.3886918087338245 ) ) ;
#4861 = CIRCLE ( 'NONE', #51675, 6.151811579824029153 ) ;
#4862 = CARTESIAN_POINT ( 'NONE',  ( 50.92442080470556220, -297.1544086963463087, -195.2244517004290003 ) ) ;
#4863 = CARTESIAN_POINT ( 'NONE',  ( -77.31782574601211877, -292.1516710513772068, -209.1581601406573441 ) ) ;
#4864 = CARTESIAN_POINT ( 'NONE',  ( -97.84361190735582170, -288.5476566689508218, -312.2747138637416811 ) ) ;
#4865 = CARTESIAN_POINT ( 'NONE',  ( 165.2494399300530290, 8.542400036368780647, 13.00000000000000178 ) ) ;
#4866 = CARTESIAN_POINT ( 'NONE',  ( 39.49247728902545163, -275.9828719430831825, -265.4374620945740162 ) ) ;
#4867 = CARTESIAN_POINT ( 'NONE',  ( -81.96039047585614412, -297.7583462934829299, -212.4933984757655310 ) ) ;
#4868 = CIRCLE ( 'NONE', #339, 4.999999999999993783 ) ;
#4869 = CARTESIAN_POINT ( 'NONE',  ( -5.658979525416277134, -282.4466340785737088, -201.9899835612124548 ) ) ;
#4870 = CARTESIAN_POINT ( 'NONE',  ( -6.414266453204220397, -279.1347559247186041, -200.3698526432170866 ) ) ;
#4871 = CARTESIAN_POINT ( 'NONE',  ( -108.5651488163527745, -277.5320518653529120, -299.3530676111329853 ) ) ;
#4872 = CARTESIAN_POINT ( 'NONE',  ( -37.55123024062151416, -282.2520423766524118, -343.5347520565074433 ) ) ;
#4873 = CARTESIAN_POINT ( 'NONE',  ( 37.80882081822648644, -279.5109957560512726, -267.1614423308773780 ) ) ;
#4874 = CARTESIAN_POINT ( 'NONE',  ( -1.419265025288412030, -273.1131209992068989, -206.1208858896487754 ) ) ;
#4875 = CARTESIAN_POINT ( 'NONE',  ( -108.7132350886247849, -280.8517928231246970, -247.1495585002936650 ) ) ;
#4876 = CYLINDRICAL_SURFACE ( 'NONE', #71586, 4.999999999999984013 ) ;
#4877 = DIRECTION ( 'NONE',  ( 0.000000000000000000, 1.000000000000000000, 0.000000000000000000 ) ) ;
#4878 = CARTESIAN_POINT ( 'NONE',  ( -113.5409431168329348, -270.9881429158849073, -267.5031164987000238 ) ) ;
#4879 = CARTESIAN_POINT ( 'NONE',  ( 19.45216918942022488, -278.2340522687968019, -319.6196649199679314 ) ) ;
#4880 = CARTESIAN_POINT ( 'NONE',  ( -67.84831361232535585, -271.6516253541363994, -201.8317462266525979 ) ) ;
#4881 = LINE ( 'NONE', #62677, #78619 ) ;
#4882 = CARTESIAN_POINT ( 'NONE',  ( -111.5880302844671235, -286.6545215665677233, -256.0599809794483122 ) ) ;
#4883 = VERTEX_POINT ( 'NONE', #4367 ) ;
#4884 = DIRECTION ( 'NONE',  ( -1.000000000000000000, 0.000000000000000000, 0.000000000000000000 ) ) ;
#4885 = CARTESIAN_POINT ( 'NONE',  ( -13.57756048138342919, -286.7436221479175629, -341.5503320769163338 ) ) ;
#4886 = DIRECTION ( 'NONE',  ( 3.961265963009670520E-15, 7.202301750926674102E-15, -1.000000000000000000 ) ) ;
#4887 = CARTESIAN_POINT ( 'NONE',  ( -10.35822302490307578, -293.4869103911102002, -338.6181503568845983 ) ) ;
#4888 = CARTESIAN_POINT ( 'NONE',  ( 33.45866640173591833, -285.4002933035421279, -247.9987146828482594 ) ) ;
#4889 = CARTESIAN_POINT ( 'NONE',  ( 155.4202272374187714, 20.25578850494577665, -12.04866793599389396 ) ) ;
#4890 = CARTESIAN_POINT ( 'NONE',  ( -87.85530130619319777, -293.7581209928216595, -325.7991621610911466 ) ) ;
#4891 = CARTESIAN_POINT ( 'NONE',  ( -32.33242597101487803, -284.5940918933791295, -194.2059996633515482 ) ) ;
#4892 = CARTESIAN_POINT ( 'NONE',  ( -74.93061786766870114, -281.1431284043267169, -206.7924221029747116 ) ) ;
#4893 = CARTESIAN_POINT ( 'NONE',  ( 37.72228080054952670, -288.9492813795278607, -285.6387973564200706 ) ) ;
#4894 = CARTESIAN_POINT ( 'NONE',  ( 25.86636303626246303, -280.3545814169787036, -312.5359299505789750 ) ) ;
#4895 = CARTESIAN_POINT ( 'NONE',  ( -96.55861513423624842, -289.9551460553725519, -313.0501912584443289 ) ) ;
#4896 = CARTESIAN_POINT ( 'NONE',  ( -7.779263522804096276, -281.8725946465293646, -202.9571503172723794 ) ) ;
#4897 = CARTESIAN_POINT ( 'NONE',  ( -38.36636668151981411, -280.8418215704745080, -197.1943884165333714 ) ) ;
#4898 = CARTESIAN_POINT ( 'NONE',  ( 33.53423964131933843, -289.8640512299933221, -296.1062003288715232 ) ) ;
#4899 = ORIENTED_EDGE ( 'NONE', *, *, #27543, .F. ) ;
#4900 = CARTESIAN_POINT ( 'NONE',  ( -29.83888329357132818, -274.1446523376640130, -193.7275239160685771 ) ) ;
#4901 = CARTESIAN_POINT ( 'NONE',  ( -111.6119060365011677, -292.6284037242052136, -262.8922950790631035 ) ) ;
#4902 = DIRECTION ( 'NONE',  ( 0.3024135303176525569, 0.9531768234072912627, 0.000000000000000000 ) ) ;
#4903 = CARTESIAN_POINT ( 'NONE',  ( 13.79469577742117714, -295.1948066931273615, -206.1857440867352693 ) ) ;
#4904 = ORIENTED_EDGE ( 'NONE', *, *, #49759, .T. ) ;
#4905 = CARTESIAN_POINT ( 'NONE',  ( -73.05090154096768629, -271.5802567210113239, -204.1603793793584032 ) ) ;
#4906 = CARTESIAN_POINT ( 'NONE',  ( 139.6925840978351516, 15.36528803885690664, 21.50000000000000000 ) ) ;
#4907 = CARTESIAN_POINT ( 'NONE',  ( -108.6956756763882765, -294.6085409226148499, -297.2505245158820344 ) ) ;
#4908 = CARTESIAN_POINT ( 'NONE',  ( -88.16405079995766414, -296.8251525760260279, -217.8016618235631086 ) ) ;
#4909 = CARTESIAN_POINT ( 'NONE',  ( -56.22474751579643026, -290.8198502892797137, -341.6471563432843368 ) ) ;
#4911 = EDGE_CURVE ( 'NONE', #16098, #8882, #2173, .T. ) ;
#4910 = CARTESIAN_POINT ( 'NONE',  ( -6.815334853809469351, -284.4060385047582713, -337.7999086390247498 ) ) ;
#4912 = CARTESIAN_POINT ( 'NONE',  ( -105.9762053092477885, -291.5414491266811297, -304.0657165305063927 ) ) ;
#4913 = CARTESIAN_POINT ( 'NONE',  ( -113.3217359044789845, -291.7490144751628236, -279.7604153408674392 ) ) ;
#4914 = CARTESIAN_POINT ( 'NONE',  ( -52.51785430827889201, -287.8579096330275320, -196.9125986646392050 ) ) ;
#4915 = CARTESIAN_POINT ( 'NONE',  ( -4.945919163748738079, -280.6337153502207116, -200.5076042538772185 ) ) ;
#4916 = CARTESIAN_POINT ( 'NONE',  ( -96.29949634516779611, -293.9865766989832423, -317.6393263222292944 ) ) ;
#4917 = CARTESIAN_POINT ( 'NONE',  ( -8.040852057305190925, -282.5122491631590265, -341.6248211671182275 ) ) ;
#4918 = CARTESIAN_POINT ( 'NONE',  ( 0.05585840449479470560, -276.4159360852512464, -206.2191581809597949 ) ) ;
#4919 = CARTESIAN_POINT ( 'NONE',  ( -102.0172624299486870, -280.6233781216988064, -301.5434626090942061 ) ) ;
#4920 = CARTESIAN_POINT ( 'NONE',  ( 21.08624753894064696, -273.1299242581312683, -221.7797537773550403 ) ) ;
#4922 = CIRCLE ( 'NONE', #69947, 155.4364916446740210 ) ;
#4921 = CARTESIAN_POINT ( 'NONE',  ( 222.8344101925596306, 36.73669859915801794, -7.000000000000000888 ) ) ;
#4923 = CARTESIAN_POINT ( 'NONE',  ( 2.742981955218880774, -280.1132504048805458, -209.2168044745507984 ) ) ;
#4924 = CIRCLE ( 'NONE', #92569, 4.999999999999986677 ) ;
#4925 = CARTESIAN_POINT ( 'NONE',  ( -101.7547436198937589, -279.2093028552251326, -311.9183268072246165 ) ) ;
#4926 = CARTESIAN_POINT ( 'NONE',  ( -65.77902170535318760, -284.7479032151845786, -199.0438594783251460 ) ) ;
#4927 = CARTESIAN_POINT ( 'NONE',  ( -0.7752702841963073910, -294.3049853421233593, -205.9968502007601217 ) ) ;
#4928 = CARTESIAN_POINT ( 'NONE',  ( 37.12823885938615831, -277.3570837300402445, -286.5673899319208999 ) ) ;
#4929 = COLOUR_RGB ( '',0.7921568627450980005, 0.8196078431372548767, 0.9333333333333333481 ) ;
#4930 = CARTESIAN_POINT ( 'NONE',  ( -73.72520433340224599, -274.8950556267691354, -203.0003704561559630 ) ) ;
#4931 = DIRECTION ( 'NONE',  ( 0.000000000000000000, 1.000000000000000000, 0.000000000000000000 ) ) ;
#4932 = CARTESIAN_POINT ( 'NONE',  ( 20.83563444569399437, -276.0051415752525941, -314.4564436579703965 ) ) ;
#4933 = CARTESIAN_POINT ( 'NONE',  ( -93.55132711363044962, -297.8643276987417039, -319.7625983513416941 ) ) ;
#4934 = EDGE_CURVE ( 'NONE', #64042, #74853, #40323, .T. ) ;
#4935 = CARTESIAN_POINT ( 'NONE',  ( -106.2767011911338670, -282.9348318859209144, -241.1076986055834652 ) ) ;
#4936 = AXIS2_PLACEMENT_3D ( 'NONE', #87857, #44781, #58554 ) ;
#4937 = CARTESIAN_POINT ( 'NONE',  ( 35.43401436272014848, -292.9007211873821461, -245.1111015900268626 ) ) ;
#4938 = CARTESIAN_POINT ( 'NONE',  ( 37.01909597755875581, -273.4810238765877557, -263.2894477876452015 ) ) ;
#4939 = CARTESIAN_POINT ( 'NONE',  ( 30.97927332278542067, -289.5918030207013771, -304.2245906810972542 ) ) ;
#4940 = CARTESIAN_POINT ( 'NONE',  ( -38.89038250136956520, -290.9525967321614530, -197.0683648794951637 ) ) ;
#4941 = EDGE_LOOP ( 'NONE', ( #13432, #18060, #5533, #32770 ) ) ;
#4942 = CARTESIAN_POINT ( 'NONE',  ( -81.57440894148207633, -290.0377729313602799, -208.0548280712945370 ) ) ;
#4943 = CARTESIAN_POINT ( 'NONE',  ( -109.2004807792858116, -290.0477307534052898, -283.3381411446984544 ) ) ;
#4944 = ORIENTED_EDGE ( 'NONE', *, *, #75080, .F. ) ;
#4945 = CARTESIAN_POINT ( 'NONE',  ( 34.78646382197024423, -288.9639754743878370, -296.5737237019787926 ) ) ;
#4946 = CARTESIAN_POINT ( 'NONE',  ( -104.4631710304650198, -279.2715894534917993, -241.6070638233822194 ) ) ;
#4947 = CARTESIAN_POINT ( 'NONE',  ( -95.35670707001334279, -294.7922099516945309, -320.5183854517390500 ) ) ;
#4948 = CARTESIAN_POINT ( 'NONE',  ( -100.9169036468908303, -285.7758635820551376, -227.0061311238433177 ) ) ;
#4949 = CARTESIAN_POINT ( 'NONE',  ( -23.79379967551184905, -286.5538590166527797, -194.5296199704773414 ) ) ;
#4950 = CARTESIAN_POINT ( 'NONE',  ( 20.20025431565767349, -282.5189068736929698, -315.3167735296333376 ) ) ;
#4951 = CARTESIAN_POINT ( 'NONE',  ( -99.96309284007092799, -248.1514199804641123, -334.2866369982713763 ) ) ;
#4952 = CARTESIAN_POINT ( 'NONE',  ( -100.6449816371857224, -246.9771042453164682, -333.4387840234001601 ) ) ;
#4953 = CARTESIAN_POINT ( 'NONE',  ( -108.6942105140528412, -263.8743016747102388, -305.4261820326353813 ) ) ;
#4954 = CARTESIAN_POINT ( 'NONE',  ( 31.41000280236153230, -275.0836566985414038, -295.5243731600141359 ) ) ;
#4955 = CARTESIAN_POINT ( 'NONE',  ( -7.393901917673681545, -275.5702496660196630, -337.2741619783982969 ) ) ;
#4956 = CARTESIAN_POINT ( 'NONE',  ( -111.5610360496762183, -296.3161605688875966, -249.8907584823023740 ) ) ;
#4957 = CARTESIAN_POINT ( 'NONE',  ( 197.9387763173789097, 281.7318850872235316, -110.5339443574438860 ) ) ;
#4958 = ADVANCED_FACE ( 'NONE', ( #82957 ), #83417, .T. ) ;
#4959 = CARTESIAN_POINT ( 'NONE',  ( 23.11797070549487287, -274.8672739589834464, -317.2644080136721527 ) ) ;
#4960 = CARTESIAN_POINT ( 'NONE',  ( -51.78079317222831435, -275.6251783136739846, -197.7173767555002541 ) ) ;
#4961 = ORIENTED_EDGE ( 'NONE', *, *, #30594, .F. ) ;
#4962 = CARTESIAN_POINT ( 'NONE',  ( -111.7376368498547379, -297.2552913091812457, -289.3367519162903250 ) ) ;
#4963 = CARTESIAN_POINT ( 'NONE',  ( 14.13117871769071243, -288.7973272495085553, -322.2121660426234371 ) ) ;
#4964 = VECTOR ( 'NONE', #8166, 1000.000000000000000 ) ;
#4965 = CARTESIAN_POINT ( 'NONE',  ( -112.1462409552617885, -297.1341629097532859, -287.9804424136190164 ) ) ;
#4966 = CARTESIAN_POINT ( 'NONE',  ( -113.3297600418439686, -297.1964372639040448, -258.2218421832878334 ) ) ;
#4967 = CARTESIAN_POINT ( 'NONE',  ( 32.75077106834511653, -293.9891801096249537, -290.8032446466365286 ) ) ;
#4968 = ORIENTED_EDGE ( 'NONE', *, *, #8073, .T. ) ;
#4969 = CARTESIAN_POINT ( 'NONE',  ( 17.86806103522776823, -278.1892442910119598, -321.9479037952636418 ) ) ;
#4970 = CARTESIAN_POINT ( 'NONE',  ( 29.23647073066169710, -280.5579615726911697, -231.8011119115069505 ) ) ;
#4971 = CARTESIAN_POINT ( 'NONE',  ( -26.97640279445920797, -277.8583732964011119, -342.8591804315925060 ) ) ;
#4972 = CARTESIAN_POINT ( 'NONE',  ( -37.10728521600817231, -278.8093545905229007, -346.3603136168954961 ) ) ;
#4973 = CARTESIAN_POINT ( 'NONE',  ( -81.60103170033016795, -275.6713841243881689, -331.3489722555592607 ) ) ;
#4974 = CARTESIAN_POINT ( 'NONE',  ( -105.9043195660262313, -297.5429670248083198, -244.8564382559320620 ) ) ;
#4975 = CARTESIAN_POINT ( 'NONE',  ( -107.2609801142003505, -295.4309342995090901, -247.2504198751506976 ) ) ;
#4976 = CARTESIAN_POINT ( 'NONE',  ( 209.7513585654922679, 305.7026273589066818, 13.99999999999999112 ) ) ;
#4977 = CARTESIAN_POINT ( 'NONE',  ( -25.41132162454394106, -280.6926714256533728, -194.3532698887637196 ) ) ;
#4978 = CARTESIAN_POINT ( 'NONE',  ( -103.1300894707911482, -278.2894091312853675, -302.1148870780011180 ) ) ;
#4979 = CARTESIAN_POINT ( 'NONE',  ( -54.40801074653987257, -287.9516542541475133, -344.9945628488656553 ) ) ;
#4980 = CARTESIAN_POINT ( 'NONE',  ( -29.33009274934805788, -300.1523752840889756, -195.1917187978136212 ) ) ;
#4981 = DIRECTION ( 'NONE',  ( 0.000000000000000000, 1.000000000000000000, 0.000000000000000000 ) ) ;
#4982 = AXIS2_PLACEMENT_3D ( 'NONE', #64437, #27960, #7553 ) ;
#4983 = CARTESIAN_POINT ( 'NONE',  ( -92.54027316206729381, -289.0655257662701842, -318.4547449679207034 ) ) ;
#4984 = CARTESIAN_POINT ( 'NONE',  ( 17.83297878087867971, -279.0959254406582204, -221.0282808264427103 ) ) ;
#4986 = CARTESIAN_POINT ( 'NONE',  ( -10.47849546694213707, -280.7789102076216068, -339.8396795446543024 ) ) ;
#4985 = CARTESIAN_POINT ( 'NONE',  ( -93.52843072218699660, -277.7970669226219229, -222.8188386279254019 ) ) ;
#4987 = CARTESIAN_POINT ( 'NONE',  ( -70.74467444915229919, -287.6118242585804978, -203.1961492263329205 ) ) ;
#4988 = CARTESIAN_POINT ( 'NONE',  ( -69.93033913081247022, -280.8181370833739834, -204.5816185000254563 ) ) ;
#4989 = CARTESIAN_POINT ( 'NONE',  ( 153.4740190581475474, 20.31595717416274738, -12.31823986473498245 ) ) ;
#4990 = AXIS2_PLACEMENT_3D ( 'NONE', #56009, #66271, #51112 ) ;
#4991 = CARTESIAN_POINT ( 'NONE',  ( -70.04914007322521741, -293.6214269492350581, -202.8687182185756797 ) ) ;
#4992 = CARTESIAN_POINT ( 'NONE',  ( -106.6610099386179940, -276.3877442776427529, -301.6149065844991242 ) ) ;
#4993 = AXIS2_PLACEMENT_3D ( 'NONE', #83914, #61688, #84371 ) ;
#4994 = CARTESIAN_POINT ( 'NONE',  ( 9.736015795006476736, -277.0351785203231429, -326.2859007832590805 ) ) ;
#4995 = CARTESIAN_POINT ( 'NONE',  ( -104.1428859094904595, -286.0959762065048153, -304.9366175320544698 ) ) ;
#4996 = VECTOR ( 'NONE', #54963, 1000.000000000000000 ) ;
#4997 = CARTESIAN_POINT ( 'NONE',  ( 197.1849154220910236, 70.00167207606656916, 10.14165260477480146 ) ) ;
#4998 = CARTESIAN_POINT ( 'NONE',  ( -69.99422823214790412, -291.3989432542661007, -338.5158228649826242 ) ) ;
#4999 = AXIS2_PLACEMENT_3D ( 'NONE', #62706, #24823, #39459 ) ;
#5000 = CARTESIAN_POINT ( 'NONE',  ( -31.34530361948588251, -292.9763882565214317, -345.1722658401024546 ) ) ;
#5001 = CARTESIAN_POINT ( 'NONE',  ( 37.66507928011557027, -286.9590909606237688, -287.0987363539143189 ) ) ;
#5002 = DIRECTION ( 'NONE',  ( -1.000000000000000000, 0.000000000000000000, 0.000000000000000000 ) ) ;
#5003 = CARTESIAN_POINT ( 'NONE',  ( -63.46647306729474991, -272.3892828533277566, -201.6544512081398466 ) ) ;
#5004 = CARTESIAN_POINT ( 'NONE',  ( 36.76941570174395935, -291.6254867809028610, -265.2545850194514401 ) ) ;
#5005 = CARTESIAN_POINT ( 'NONE',  ( 223.4306832106270804, -134.2391364535880882, 21.50000000000000000 ) ) ;
#5006 = CYLINDRICAL_SURFACE ( 'NONE', #17159, 7.910944475430059519 ) ;
#5007 = CARTESIAN_POINT ( 'NONE',  ( -113.3145806173120747, -289.1288763778699149, -262.6872617894036921 ) ) ;
#5008 = CARTESIAN_POINT ( 'NONE',  ( -72.77583245151139124, -287.1747305923090039, -205.6098712105278423 ) ) ;
#5009 = CARTESIAN_POINT ( 'NONE',  ( 13.58459175419786469, -284.9932857787292733, -213.8947004972047523 ) ) ;
#5010 = AXIS2_PLACEMENT_3D ( 'NONE', #36406, #29781, #44884 ) ;
#5011 = CARTESIAN_POINT ( 'NONE',  ( -109.7762140521277985, -286.1482823676980729, -257.3049056694184742 ) ) ;
#5012 = LINE ( 'NONE', #69401, #47218 ) ;
#5013 = CARTESIAN_POINT ( 'NONE',  ( -102.3866143922282959, -285.8092800991270792, -236.8684194527228044 ) ) ;
#5014 = CARTESIAN_POINT ( 'NONE',  ( -2.832048895173628011, -294.4858264621272497, -203.3579218688950618 ) ) ;
#5015 = CARTESIAN_POINT ( 'NONE',  ( 36.18484919670623157, -273.8545614876391596, -287.8282825112267460 ) ) ;
#5016 = CARTESIAN_POINT ( 'NONE',  ( 36.47439572649278006, -276.1600111458380979, -292.2463213957709058 ) ) ;
#5017 = CIRCLE ( 'NONE', #18666, 4.000000000000003553 ) ;
#5018 = CARTESIAN_POINT ( 'NONE',  ( 21.11112761909973656, -290.9768259910583197, -222.4802122861924545 ) ) ;
#5019 = CARTESIAN_POINT ( 'NONE',  ( -103.4115949214931049, -279.0689577831113297, -230.7129256192662012 ) ) ;
#5020 = CARTESIAN_POINT ( 'NONE',  ( -109.1790465747947252, -298.2698734096895805, -290.6402318670120621 ) ) ;
#5021 = CARTESIAN_POINT ( 'NONE',  ( -48.18343439339133027, -251.4422407193385709, -487.0093695598080785 ) ) ;
#5022 = CARTESIAN_POINT ( 'NONE',  ( 164.2231345125756263, 291.1800221208779931, 7.500000000000000000 ) ) ;
#5023 = CARTESIAN_POINT ( 'NONE',  ( -54.85775004620027318, -284.5071882890613324, -198.9331834819201674 ) ) ;
#5024 = CARTESIAN_POINT ( 'NONE',  ( 32.47230984654849095, -279.1936863048373993, -242.8147828625224633 ) ) ;
#5025 = LINE ( 'NONE', #55224, #27169 ) ;
#5026 = CARTESIAN_POINT ( 'NONE',  ( 2.076564583637728223, -273.0497195135510538, -205.0242359065937592 ) ) ;
#5027 = CARTESIAN_POINT ( 'NONE',  ( -92.80938918636424262, -277.2237864368000260, -317.9765371131321103 ) ) ;
#5028 = CARTESIAN_POINT ( 'NONE',  ( 21.08463185388143657, -295.6985930922944021, -315.2936044259757296 ) ) ;
#5029 = AXIS2_PLACEMENT_3D ( 'NONE', #20873, #6206, #93302 ) ;
#5030 = CARTESIAN_POINT ( 'NONE',  ( 38.36049495791547059, -280.6276452433605755, -282.7178377671999101 ) ) ;
#5031 = CARTESIAN_POINT ( 'NONE',  ( 6.212465513629102709, -295.3860070676503824, -329.3008315412002958 ) ) ;
#5032 = CARTESIAN_POINT ( 'NONE',  ( -13.91701166505555598, -296.0695788362795611, -343.1936810450267217 ) ) ;
#5033 = CARTESIAN_POINT ( 'NONE',  ( -65.57075502926024058, -297.5057496763832319, -203.0400925603047426 ) ) ;
#5034 = CARTESIAN_POINT ( 'NONE',  ( -109.6876677991897111, -292.8066095137401703, -250.5858401657527565 ) ) ;
#5035 = CARTESIAN_POINT ( 'NONE',  ( -83.27758010909099085, -285.6092075321863035, -208.4974189148646246 ) ) ;
#5036 = CARTESIAN_POINT ( 'NONE',  ( 22.52719625648783008, -274.3221202761614563, -316.8151213583173558 ) ) ;
#5037 = CARTESIAN_POINT ( 'NONE',  ( 36.78383620576741464, -287.6472096046332467, -291.2518487455981244 ) ) ;
#5038 = CARTESIAN_POINT ( 'NONE',  ( -46.68682590685827449, -281.9129743228164671, -196.2513484276414033 ) ) ;
#5039 = CARTESIAN_POINT ( 'NONE',  ( 23.69900906503054117, -287.1708816242754096, -310.8493154275352595 ) ) ;
#5040 = CARTESIAN_POINT ( 'NONE',  ( -110.3226133027325488, -288.3293463810759363, -287.7016012181065321 ) ) ;
#5041 = CARTESIAN_POINT ( 'NONE',  ( 202.9739649223127742, 291.4636489454787807, -68.19743562414970484 ) ) ;
#5042 = CARTESIAN_POINT ( 'NONE',  ( 27.71579033283434867, -286.6071144906486552, -237.0003213354131617 ) ) ;
#5043 = CARTESIAN_POINT ( 'NONE',  ( 169.7306087885279169, 215.0000000000000568, -24.89999999999998792 ) ) ;
#5044 = CARTESIAN_POINT ( 'NONE',  ( 36.25654271108132320, -282.7700688847044148, -292.3642315058255008 ) ) ;
#5045 = CARTESIAN_POINT ( 'NONE',  ( -81.78437819734608638, -290.5217153100768428, -207.7698360146215748 ) ) ;
#5046 = CARTESIAN_POINT ( 'NONE',  ( -38.18174308455428445, -281.6419110099115528, -194.1657457726626603 ) ) ;
#5047 = CARTESIAN_POINT ( 'NONE',  ( 31.56994647985871794, -282.4368314243427562, -237.0055265298853442 ) ) ;
#5048 = CARTESIAN_POINT ( 'NONE',  ( 18.49298438396720101, -282.0537006252001220, -317.4069823893198645 ) ) ;
#5049 = CARTESIAN_POINT ( 'NONE',  ( 8.534723961188817043, -276.6807212584855620, -211.0285438057990461 ) ) ;
#5050 = CARTESIAN_POINT ( 'NONE',  ( -88.60543184964716090, -295.7476945571318652, -327.8872069434855234 ) ) ;
#5051 = CARTESIAN_POINT ( 'NONE',  ( -109.6967354547859657, -288.8096750788182590, -251.9626610498688137 ) ) ;
#5052 = CARTESIAN_POINT ( 'NONE',  ( -41.87377477762861133, -296.9140259600816307, -197.1922286007973071 ) ) ;
#5053 = ORIENTED_EDGE ( 'NONE', *, *, #31405, .T. ) ;
#5054 = ORIENTED_EDGE ( 'NONE', *, *, #48, .T. ) ;
#5055 = CARTESIAN_POINT ( 'NONE',  ( -110.3879110723479755, -286.2868295445725266, -284.6986654427787471 ) ) ;
#5056 = VECTOR ( 'NONE', #90212, 1000.000000000000000 ) ;
#5057 = CARTESIAN_POINT ( 'NONE',  ( 31.90093501509288387, -294.2061152915784419, -237.2688259575994323 ) ) ;
#5058 = CARTESIAN_POINT ( 'NONE',  ( 20.26641750026905697, -282.8369874063569682, -315.3633118388252115 ) ) ;
#5059 = EDGE_CURVE ( 'NONE', #3540, #71727, #67204, .T. ) ;
#5060 = CARTESIAN_POINT ( 'NONE',  ( 33.50105024918833863, -274.2322092032831051, -240.6581716900169567 ) ) ;
#5061 = CARTESIAN_POINT ( 'NONE',  ( -114.2880357200276222, -291.1926095281505695, -271.2358884801321892 ) ) ;
#5062 = CARTESIAN_POINT ( 'NONE',  ( -64.08860717743114321, -283.8465434078051999, -199.4605909208435151 ) ) ;
#5063 = CARTESIAN_POINT ( 'NONE',  ( -13.87693914222193925, -292.6816548335221455, -196.9897498673465464 ) ) ;
#5065 = CARTESIAN_POINT ( 'NONE',  ( 32.33507116531379921, -288.1768837280231423, -292.3751480622312897 ) ) ;
#5064 = CIRCLE ( 'NONE', #57926, 24.00000000000001066 ) ;
#5066 = DIRECTION ( 'NONE',  ( 0.000000000000000000, 0.000000000000000000, -1.000000000000000000 ) ) ;
#5067 = CIRCLE ( 'NONE', #41325, 5.024999999999987921 ) ;
#5068 = DIRECTION ( 'NONE',  ( -0.000000000000000000, -0.000000000000000000, -1.000000000000000000 ) ) ;
#5069 = CARTESIAN_POINT ( 'NONE',  ( 84.55120471034096852, 81.53809721804566379, -298.7488921200802565 ) ) ;
#5070 = CARTESIAN_POINT ( 'NONE',  ( 1.755669219107143464, -284.0592657388145312, -335.8905271248909230 ) ) ;
#5071 = CARTESIAN_POINT ( 'NONE',  ( -114.2704648735229114, -288.0523547857346784, -270.3284710469133074 ) ) ;
#5072 = EDGE_LOOP ( 'NONE', ( #48504, #81925, #52420, #87146, #87917, #35825, #76451, #55613, #54390, #82572, #65555 ) ) ;
#5073 = CARTESIAN_POINT ( 'NONE',  ( 10.09830747003844920, -281.3006949694444643, -326.3176821264667069 ) ) ;
#5074 = CARTESIAN_POINT ( 'NONE',  ( 19.85864627916476977, -275.9185262159213039, -321.8965172615079950 ) ) ;
#5075 = CARTESIAN_POINT ( 'NONE',  ( -7.285914942196468402, -282.4473899109673312, -201.8147896459126116 ) ) ;
#5076 = CARTESIAN_POINT ( 'NONE',  ( 27.32813335771293239, -24.61695715926212102, -343.0477418883668861 ) ) ;
#5077 = CARTESIAN_POINT ( 'NONE',  ( 35.90857445423406347, -280.4039265822380571, -292.2916365071041582 ) ) ;
#5079 = AXIS2_PLACEMENT_3D ( 'NONE', #33405, #68468, #26311 ) ;
#5078 = CARTESIAN_POINT ( 'NONE',  ( -84.67175412479804208, -283.4168336077982531, -212.5729866804885546 ) ) ;
#5080 = CARTESIAN_POINT ( 'NONE',  ( -67.79224647856602814, -299.4182591044454966, -200.6865393352724993 ) ) ;
#5081 = CARTESIAN_POINT ( 'NONE',  ( 12.40135767224208685, -294.8293791304913043, -323.9432353398989335 ) ) ;
#5082 = ORIENTED_EDGE ( 'NONE', *, *, #793, .T. ) ;
#5083 = CARTESIAN_POINT ( 'NONE',  ( -86.24477230005112460, -290.0418852153470084, -215.4316006113672586 ) ) ;
#5084 = CARTESIAN_POINT ( 'NONE',  ( 31.76732283218936104, -276.6384922139824880, -304.2056527103570147 ) ) ;
#5085 = CARTESIAN_POINT ( 'NONE',  ( -43.48212421531537331, -273.9725701068415447, -197.5691177544540835 ) ) ;
#5086 = CARTESIAN_POINT ( 'NONE',  ( -27.02443708261399280, -273.1005857086767037, -194.3141744618107225 ) ) ;
#5087 = CARTESIAN_POINT ( 'NONE',  ( 216.5288609127277084, 293.9636489450776935, 13.99999999999999112 ) ) ;
#5088 = CARTESIAN_POINT ( 'NONE',  ( 30.22679961042809538, -273.1219261130304972, -237.6930814542139387 ) ) ;
#5089 = VECTOR ( 'NONE', #77679, 1000.000000000000000 ) ;
#5090 = EDGE_CURVE ( 'NONE', #63778, #72125, #60743, .T. ) ;
#5091 = CARTESIAN_POINT ( 'NONE',  ( 194.3144103428324172, 249.5000000000000568, 16.91223866672520515 ) ) ;
#5092 = CARTESIAN_POINT ( 'NONE',  ( 35.87533242312211001, -282.6800807273444889, -274.0342933361034738 ) ) ;
#5093 = CARTESIAN_POINT ( 'NONE',  ( 33.37305974970083611, -282.9533825498997430, -242.4076021657018885 ) ) ;
#5094 = CARTESIAN_POINT ( 'NONE',  ( -84.93441606973981095, -283.0780242595014329, -325.8482881856795643 ) ) ;
#5095 = CARTESIAN_POINT ( 'NONE',  ( -35.34851826131681918, -272.4774188881562509, -196.5753937415116468 ) ) ;
#5096 = CARTESIAN_POINT ( 'NONE',  ( 33.14203194492596793, -283.1064974253362720, -246.8988552184602270 ) ) ;
#5097 = CARTESIAN_POINT ( 'NONE',  ( 29.72499716802074943, -273.6226756817299020, -239.6963876090953818 ) ) ;
#5098 = CARTESIAN_POINT ( 'NONE',  ( 207.4652116465272798, 29.76295193202772538, 14.90818566952114921 ) ) ;
#5099 = CARTESIAN_POINT ( 'NONE',  ( 33.80587072756687661, -276.3996271837275458, -252.6905425564350764 ) ) ;
#5100 = CARTESIAN_POINT ( 'NONE',  ( 175.2296996224750103, 275.0000000000000568, 0.000000000000000000 ) ) ;
#5101 = CARTESIAN_POINT ( 'NONE',  ( -20.15226036016875000, -277.6396767212351619, -345.3068580607388185 ) ) ;
#5102 = AXIS2_PLACEMENT_3D ( 'NONE', #7934, #51481, #30188 ) ;
#5103 = EDGE_CURVE ( 'NONE', #85761, #66913, #89584, .T. ) ;
#5104 = VERTEX_POINT ( 'NONE', #62140 ) ;
#5105 = FACE_OUTER_BOUND ( 'NONE', #23551, .T. ) ;
#5106 = CARTESIAN_POINT ( 'NONE',  ( -86.95920298751730115, -287.2309480093535967, -213.0342522295029539 ) ) ;
#5107 = CARTESIAN_POINT ( 'NONE',  ( -94.90681123830276533, -295.1140213192787201, -315.5148521626750835 ) ) ;
#5108 = CARTESIAN_POINT ( 'NONE',  ( -17.75830013185584022, -288.1545815999714364, -344.7237647272082768 ) ) ;
#5109 = CARTESIAN_POINT ( 'NONE',  ( -14.22856941916255558, -284.5957515971525140, -199.9955003492453329 ) ) ;
#5111 = CARTESIAN_POINT ( 'NONE',  ( -83.19132075283120287, -287.9299288940537735, -328.4626351696686015 ) ) ;
#5110 = CARTESIAN_POINT ( 'NONE',  ( -65.30040432951437879, -284.2542696943920646, -202.2357010858243598 ) ) ;
#5112 = CARTESIAN_POINT ( 'NONE',  ( -78.58716304388681806, -284.8265352353776620, -331.0730796778912577 ) ) ;
#5113 = CARTESIAN_POINT ( 'NONE',  ( -38.53925083100407534, -275.0670126289074915, -345.3515608738567835 ) ) ;
#5114 = CARTESIAN_POINT ( 'NONE',  ( 1.135500732134293589, -284.9566924188076200, -204.5740170980117796 ) ) ;
#5115 = CARTESIAN_POINT ( 'NONE',  ( -108.9124582445111997, -298.8435117785385842, -247.7694212526806723 ) ) ;
#5116 = CARTESIAN_POINT ( 'NONE',  ( 32.17388447191516576, -285.1782093035108687, -241.6311128308203706 ) ) ;
#5117 = AXIS2_PLACEMENT_3D ( 'NONE', #36297, #318, #35383 ) ;
#5118 = CARTESIAN_POINT ( 'NONE',  ( 34.79680009934898521, -282.3273694958396050, -257.7339554567607820 ) ) ;
#5119 = CARTESIAN_POINT ( 'NONE',  ( -20.87267618207762609, -290.8415605568310980, -343.7547885268265873 ) ) ;
#5120 = CARTESIAN_POINT ( 'NONE',  ( 175.2296996224750103, 249.5000000000000568, 0.000000000000000000 ) ) ;
#5121 = PLANE ( 'NONE',  #20122 ) ;
#5122 = CARTESIAN_POINT ( 'NONE',  ( -41.83501847219821457, -297.0283678103869534, -345.8388161005366896 ) ) ;
#5123 = CARTESIAN_POINT ( 'NONE',  ( -7.172173674521296505, -278.4477156150321662, -201.6826648416823673 ) ) ;
#5124 = CARTESIAN_POINT ( 'NONE',  ( -8.562192552985097294, -291.6165615031683842, -199.1157759289823730 ) ) ;
#5125 = CARTESIAN_POINT ( 'NONE',  ( -104.6747840226607451, -294.5480159960924311, -300.6969782868713423 ) ) ;
#5126 = CARTESIAN_POINT ( 'NONE',  ( 21.39400427248041225, -280.8533649351057875, -314.5561145920430022 ) ) ;
#5127 = CARTESIAN_POINT ( 'NONE',  ( 20.99903835387845419, -272.9918385989889771, -224.1057428699021443 ) ) ;
#5128 = CARTESIAN_POINT ( 'NONE',  ( 36.02583457602933237, -294.8005654733542542, -265.2655767428273634 ) ) ;
#5129 = CARTESIAN_POINT ( 'NONE',  ( -95.95921662488163406, -292.4090924074130839, -317.1477375740089997 ) ) ;
#5130 = CARTESIAN_POINT ( 'NONE',  ( -107.1310066386831892, -295.4308000253812452, -239.3734549974685422 ) ) ;
#5131 = CARTESIAN_POINT ( 'NONE',  ( -36.36852897070759383, -290.3040614007007889, -194.3678186611271315 ) ) ;
#5132 = CARTESIAN_POINT ( 'NONE',  ( -104.0984007623582954, -292.3920682971040605, -239.3947194858239698 ) ) ;
#5133 = CYLINDRICAL_SURFACE ( 'NONE', #58146, 0.5000000000000004441 ) ;
#5134 = CARTESIAN_POINT ( 'NONE',  ( -49.72609649922945607, -292.6931247937685612, -198.2040023265234083 ) ) ;
#5135 = DIRECTION ( 'NONE',  ( -0.000000000000000000, -0.000000000000000000, 1.000000000000000000 ) ) ;
#5136 = CARTESIAN_POINT ( 'NONE',  ( -86.27125971562368534, -292.5959736771948201, -211.3523733338774946 ) ) ;
#5138 = CARTESIAN_POINT ( 'NONE',  ( -32.15728590108069085, -292.1193325364559428, -197.5328273110813484 ) ) ;
#5137 = CARTESIAN_POINT ( 'NONE',  ( 33.04203922870224375, -279.9204885338987765, -297.2783250247895808 ) ) ;
#5139 = AXIS2_PLACEMENT_3D ( 'NONE', #60418, #89258, #40927 ) ;
#5140 = CARTESIAN_POINT ( 'NONE',  ( 39.61980569469341162, -281.5825985165997167, -272.7955833224256708 ) ) ;
#5141 = CARTESIAN_POINT ( 'NONE',  ( -99.77381981583235415, -283.6206010088851599, -315.4832449321209538 ) ) ;
#5142 = CARTESIAN_POINT ( 'NONE',  ( -91.94756060828976274, -287.8330834983093496, -321.6054472438466405 ) ) ;
#5143 = CARTESIAN_POINT ( 'NONE',  ( -79.09052343481252478, -281.7615372537368330, -331.7443504719050793 ) ) ;
#5144 = CARTESIAN_POINT ( 'NONE',  ( 175.2296996224750103, 131.0000000000000568, 0.000000000000000000 ) ) ;
#5145 = CARTESIAN_POINT ( 'NONE',  ( -81.81889464704876502, -277.9382048940400409, -208.3571913424385116 ) ) ;
#5146 = AXIS2_PLACEMENT_3D ( 'NONE', #20387, #56372, #64447 ) ;
#5147 = CARTESIAN_POINT ( 'NONE',  ( 5.020432208683907049, -285.5302226169452524, -206.3686620744306310 ) ) ;
#5148 = CARTESIAN_POINT ( 'NONE',  ( 121.3395553409046670, -299.5541904835127980, -192.6222259952039622 ) ) ;
#5149 = CARTESIAN_POINT ( 'NONE',  ( 27.87446622108598859, -295.6190312693804003, -305.0144347577275425 ) ) ;
#5150 = CARTESIAN_POINT ( 'NONE',  ( -17.49333229435270098, -278.2261936918599190, -344.1489800311915701 ) ) ;
#5151 = CARTESIAN_POINT ( 'NONE',  ( -64.34490735153218566, -277.0810877185979848, -338.2595982287882634 ) ) ;
#5152 = CARTESIAN_POINT ( 'NONE',  ( -86.51466323652709889, -291.5577450825049937, -211.0380268287154024 ) ) ;
#5153 = CIRCLE ( 'NONE', #88260, 24.00000000000000355 ) ;
#5154 = CARTESIAN_POINT ( 'NONE',  ( -96.92429515610150759, -281.9993398261785273, -316.8286181507845072 ) ) ;
#5155 = AXIS2_PLACEMENT_3D ( 'NONE', #54767, #68527, #54304 ) ;
#5156 = CARTESIAN_POINT ( 'NONE',  ( 25.99015165447522691, -293.1138321019154773, -307.1372651085534926 ) ) ;
#5157 = CARTESIAN_POINT ( 'NONE',  ( -109.6859245714938282, -294.8085908961669475, -250.3878057391564198 ) ) ;
#5158 = ORIENTED_EDGE ( 'NONE', *, *, #48217, .F. ) ;
#5159 = CARTESIAN_POINT ( 'NONE',  ( 219.8344101925596021, 35.72494958537217968, 7.000000000000000000 ) ) ;
#5160 = AXIS2_PLACEMENT_3D ( 'NONE', #32703, #88102, #23728 ) ;
#5161 = CARTESIAN_POINT ( 'NONE',  ( 27.54406242065528687, -292.6034922699741969, -236.7779933522577664 ) ) ;
#5162 = FACE_OUTER_BOUND ( 'NONE', #92401, .T. ) ;
#5163 = CARTESIAN_POINT ( 'NONE',  ( -6.941161984400256557, -289.9809262143061233, -207.3071070584150277 ) ) ;
#5164 = CARTESIAN_POINT ( 'NONE',  ( -86.25463878613970792, -294.7707406654784563, -329.5248285162815023 ) ) ;
#5165 = CARTESIAN_POINT ( 'NONE',  ( 21.03439454779123352, -279.0319637508834489, -222.0647718033168587 ) ) ;
#5166 = CARTESIAN_POINT ( 'NONE',  ( -30.94190509126000066, -287.4465713232191320, -194.1091984313555656 ) ) ;
#5167 = CARTESIAN_POINT ( 'NONE',  ( -17.16983973862676649, -286.1530880547942388, -200.1506183683458744 ) ) ;
#5168 = CARTESIAN_POINT ( 'NONE',  ( -109.4391165252961997, -279.8729500919551469, -285.6146521058996086 ) ) ;
#5169 = CARTESIAN_POINT ( 'NONE',  ( -109.1927484744432348, -294.3107287378887804, -290.5916309758698048 ) ) ;
#5170 = CARTESIAN_POINT ( 'NONE',  ( -109.2786872212679015, -298.0850999727042563, -287.8226540892346179 ) ) ;
#5171 = AXIS2_PLACEMENT_3D ( 'NONE', #44618, #154, #77957 ) ;
#5172 = CARTESIAN_POINT ( 'NONE',  ( -110.5536381880899768, -277.4154249027404830, -265.1512591097055633 ) ) ;
#5173 = ORIENTED_EDGE ( 'NONE', *, *, #11459, .F. ) ;
#5174 = CARTESIAN_POINT ( 'NONE',  ( 185.8264795993290477, 249.5000000000000568, 23.09031830825835385 ) ) ;
#5175 = CARTESIAN_POINT ( 'NONE',  ( -112.5789292484276984, -296.4232784899679132, -254.0176057555253522 ) ) ;
#5176 = CARTESIAN_POINT ( 'NONE',  ( -73.02812715167979718, -291.4491800446547245, -335.6894665437833964 ) ) ;
#5177 = CARTESIAN_POINT ( 'NONE',  ( 60.30377782462292657, -249.1633071459562530, -22.50000000000000000 ) ) ;
#5178 = CARTESIAN_POINT ( 'NONE',  ( -53.42289092708005427, -289.9153492663852489, -341.6723230650061964 ) ) ;
#5179 = CARTESIAN_POINT ( 'NONE',  ( -48.18343439339133027, -259.2349860072159800, -447.3766206888376473 ) ) ;
#5181 = ORIENTED_EDGE ( 'NONE', *, *, #50089, .T. ) ;
#5180 = EDGE_CURVE ( 'NONE', #14315, #57029, #44470, .T. ) ;
#5182 = CARTESIAN_POINT ( 'NONE',  ( 11.33411921951718426, -281.4554532092836894, -329.7888444128520291 ) ) ;
#5183 = CARTESIAN_POINT ( 'NONE',  ( -101.5385901050513553, -296.6450866686284940, -312.7902762043616463 ) ) ;
#5184 = CARTESIAN_POINT ( 'NONE',  ( -89.91155455344491543, -289.4594214597105974, -215.7290396917294402 ) ) ;
#5185 = CARTESIAN_POINT ( 'NONE',  ( -102.3008286208124247, -297.4269585560355722, -229.0566882328157874 ) ) ;
#5186 = CARTESIAN_POINT ( 'NONE',  ( 16.17752346111596751, -294.5992251257119960, -320.0378750546560696 ) ) ;
#5187 = DIRECTION ( 'NONE',  ( 0.000000000000000000, 0.000000000000000000, 1.000000000000000000 ) ) ;
#5188 = SURFACE_STYLE_FILL_AREA ( #21248 ) ;
#5189 = CARTESIAN_POINT ( 'NONE',  ( 208.6208076322478746, 32.98517505407394168, 12.09245862095555601 ) ) ;
#5190 = CARTESIAN_POINT ( 'NONE',  ( -59.80454023100995187, -290.8581414735180601, -343.2866180892807506 ) ) ;
#5191 = CARTESIAN_POINT ( 'NONE',  ( 36.60358173371528068, -278.4805209788416391, -305.9350535429201159 ) ) ;
#5192 = ORIENTED_EDGE ( 'NONE', *, *, #21097, .F. ) ;
#5193 = CARTESIAN_POINT ( 'NONE',  ( -6.263947264179056340, -279.7984094211952879, -200.0084954448707890 ) ) ;
#5194 = CARTESIAN_POINT ( 'NONE',  ( -92.89900469587266230, -287.2533497265698088, -220.1509817255634118 ) ) ;
#5195 = CARTESIAN_POINT ( 'NONE',  ( 1.239958049647971627, -285.1315202942427618, -204.3908957128678878 ) ) ;
#5196 = CARTESIAN_POINT ( 'NONE',  ( 18.67441364952511407, -272.8596833560802679, -220.6635065063786669 ) ) ;
#5197 = CARTESIAN_POINT ( 'NONE',  ( -59.93553525168671570, -275.6774021192776445, -199.3787818580472617 ) ) ;
#5198 = CARTESIAN_POINT ( 'NONE',  ( -107.9291627250842964, -288.9398651247442444, -246.7237678453780063 ) ) ;
#5199 = CARTESIAN_POINT ( 'NONE',  ( -110.9691125764410344, -280.1847479181629410, -288.2846260749583394 ) ) ;
#5200 = ORIENTED_EDGE ( 'NONE', *, *, #90748, .T. ) ;
#5202 = CARTESIAN_POINT ( 'NONE',  ( 35.80471126089338441, -280.9134106719703254, -271.3233667817196988 ) ) ;
#5201 = CARTESIAN_POINT ( 'NONE',  ( -72.12970831731853139, -279.5783575795214233, -206.1832831310665313 ) ) ;
#5203 = CARTESIAN_POINT ( 'NONE',  ( 39.24476117293337296, -276.5701015933856866, -265.4458315290269184 ) ) ;
#5204 = CARTESIAN_POINT ( 'NONE',  ( -92.77575336046501775, -278.0743631382828767, -217.4168829144651056 ) ) ;
#5205 = CARTESIAN_POINT ( 'NONE',  ( 83.01528650091917427, 82.86587161941417889, -299.6803353214908725 ) ) ;
#5206 = CARTESIAN_POINT ( 'NONE',  ( -110.8154329800676834, -273.7754314059740182, -247.9435182257268480 ) ) ;
#5207 = EDGE_CURVE ( 'NONE', #58726, #51305, #18800, .T. ) ;
#5208 = CARTESIAN_POINT ( 'NONE',  ( -54.48078351602919156, -299.2613780133917203, -195.8973139439567888 ) ) ;
#5209 = CARTESIAN_POINT ( 'NONE',  ( 10.64812456238590066, -290.9090924074130839, -330.4860931364851808 ) ) ;
#5210 = ORIENTED_EDGE ( 'NONE', *, *, #44156, .F. ) ;
#5211 = AXIS2_PLACEMENT_3D ( 'NONE', #50876, #15355, #79758 ) ;
#5212 = CARTESIAN_POINT ( 'NONE',  ( 35.96440432506301477, -288.6405545456452728, -271.0252885460425887 ) ) ;
#5213 = CARTESIAN_POINT ( 'NONE',  ( 35.81498924262982086, -289.5737196124663342, -290.9532980691903958 ) ) ;
#5214 = EDGE_CURVE ( 'NONE', #77986, #22426, #29416, .T. ) ;
#5215 = CARTESIAN_POINT ( 'NONE',  ( -107.4907741942367352, -290.1729894693338565, -249.7497225756217745 ) ) ;
#5216 = CARTESIAN_POINT ( 'NONE',  ( -111.6601301425914130, -284.3115295270666252, -250.2537107587252194 ) ) ;
#5217 = CARTESIAN_POINT ( 'NONE',  ( -38.34447141573473772, -278.4392501149724239, -196.5553919712435516 ) ) ;
#5218 = CARTESIAN_POINT ( 'NONE',  ( -75.37291989161539618, -287.3996389462576531, -206.6077509852390506 ) ) ;
#5219 = CARTESIAN_POINT ( 'NONE',  ( 24.70382933162989758, -280.5780566252981885, -310.2174366137197694 ) ) ;
#5220 = CARTESIAN_POINT ( 'NONE',  ( -109.0918435712439560, -280.0765010432311897, -254.3924322468265586 ) ) ;
#5221 = AXIS2_PLACEMENT_3D ( 'NONE', #77564, #25040, #32138 ) ;
#5222 = CARTESIAN_POINT ( 'NONE',  ( -13.75960945927488410, -277.2301571350907352, -339.5653938045198856 ) ) ;
#5223 = CARTESIAN_POINT ( 'NONE',  ( -84.93007324650470480, -288.4866295489613890, -330.4567619164132566 ) ) ;
#5224 = CARTESIAN_POINT ( 'NONE',  ( -99.65151941333596142, -284.7565312445059362, -315.4127301472503859 ) ) ;
#5225 = CARTESIAN_POINT ( 'NONE',  ( -90.39116480040159729, -284.2710423361637027, -326.1592125277091441 ) ) ;
#5226 = CARTESIAN_POINT ( 'NONE',  ( 1.103112464788249314, -282.6903604730115376, -332.4765417471646174 ) ) ;
#5227 = ORIENTED_EDGE ( 'NONE', *, *, #17969, .F. ) ;
#5228 = DIRECTION ( 'NONE',  ( 1.000000000000000000, 0.000000000000000000, 0.000000000000000000 ) ) ;
#5229 = CARTESIAN_POINT ( 'NONE',  ( -94.74088923696332643, -293.0913761484256383, -220.8878821829949288 ) ) ;
#5230 = CARTESIAN_POINT ( 'NONE',  ( -39.18292794993724470, -290.7143634581076981, -193.8634737358342761 ) ) ;
#5231 = VECTOR ( 'NONE', #32325, 1000.000000000000114 ) ;
#5232 = CARTESIAN_POINT ( 'NONE',  ( 17.46960225621667462, -273.9184208313080262, -221.7150878113808972 ) ) ;
#5233 = CARTESIAN_POINT ( 'NONE',  ( -53.27623570813805998, -294.5997837917406059, -345.6445963459857467 ) ) ;
#5234 = CARTESIAN_POINT ( 'NONE',  ( -82.13527866676525946, -289.9088187613551213, -211.7795256885372908 ) ) ;
#5235 = CARTESIAN_POINT ( 'NONE',  ( -72.62714917692127869, -293.7658967764913882, -335.4364132261795248 ) ) ;
#5236 = CARTESIAN_POINT ( 'NONE',  ( -53.48098859572185404, -290.4689226899012624, -341.9617735058484413 ) ) ;
#5237 = CARTESIAN_POINT ( 'NONE',  ( 196.1227023549103592, 275.0000000000000568, -11.81026827902096876 ) ) ;
#5238 = AXIS2_PLACEMENT_3D ( 'NONE', #91230, #26396, #3009 ) ;
#5239 = CARTESIAN_POINT ( 'NONE',  ( -109.3201032708799545, -292.8236813696574359, -249.2871973460374591 ) ) ;
#5240 = CARTESIAN_POINT ( 'NONE',  ( 29.28595432435684387, -291.0908401502043716, -235.4526725880037077 ) ) ;
#5241 = CARTESIAN_POINT ( 'NONE',  ( -9.761006749027520968, -296.6922007399874133, -340.1605706291933870 ) ) ;
#5242 = CARTESIAN_POINT ( 'NONE',  ( -38.64106608655507102, -286.9767521562553725, -197.1248289421772881 ) ) ;
#5243 = CARTESIAN_POINT ( 'NONE',  ( -41.81048221307512591, -297.1083613095757414, -345.4459798781037421 ) ) ;
#5244 = CARTESIAN_POINT ( 'NONE',  ( 37.98056521063064395, -277.5777847643498717, -273.9401515419625071 ) ) ;
#5245 = VECTOR ( 'NONE', #31256, 1000.000000000000000 ) ;
#5246 = CARTESIAN_POINT ( 'NONE',  ( -87.34940106855336239, -296.5728717160762926, -211.9524152496438489 ) ) ;
#5247 = CARTESIAN_POINT ( 'NONE',  ( 32.20636937398665367, -274.1265022785975702, -295.8286906556134568 ) ) ;
#5248 = CARTESIAN_POINT ( 'NONE',  ( -24.60645761907724349, -278.2957697506427621, -197.0185805737351359 ) ) ;
#5249 = CARTESIAN_POINT ( 'NONE',  ( -36.49292348757258964, -299.3781713783291707, -196.8677687253267550 ) ) ;
#5250 = CARTESIAN_POINT ( 'NONE',  ( -5.344347276814142234, -273.0397253587576074, -200.9725331469751666 ) ) ;
#5251 = CARTESIAN_POINT ( 'NONE',  ( -45.13523733884863276, -296.5779169706398761, -343.5873780670190172 ) ) ;
#5252 = CARTESIAN_POINT ( 'NONE',  ( 140.6539576904058606, 249.5000000000000568, 12.00000000000000000 ) ) ;
#5253 = CARTESIAN_POINT ( 'NONE',  ( -104.0797307080208327, -296.9505903062203060, -300.4621927159616348 ) ) ;
#5254 = PLANE ( 'NONE',  #58017 ) ;
#5256 = CARTESIAN_POINT ( 'NONE',  ( -37.14961190020886761, -298.0546309613013136, -197.3582692470340874 ) ) ;
#5255 = CARTESIAN_POINT ( 'NONE',  ( -90.45744271053995078, -287.8193310567069148, -323.8866247585355609 ) ) ;
#5257 = CARTESIAN_POINT ( 'NONE',  ( 33.85942663172103551, -287.1780478192079613, -240.9063071331173660 ) ) ;
#5258 = CARTESIAN_POINT ( 'NONE',  ( -71.90078118066590207, -289.1632299533132482, -339.1463940846297760 ) ) ;
#5259 = CARTESIAN_POINT ( 'NONE',  ( -112.0190556993653246, -298.3982976316639224, -280.8269497424009273 ) ) ;
#5260 = CARTESIAN_POINT ( 'NONE',  ( -3.530552100319642062, -292.6047140820548975, -337.1349946108709332 ) ) ;
#5261 = CARTESIAN_POINT ( 'NONE',  ( 19.04861993276122334, -280.0368671646253915, -218.1663804704797087 ) ) ;
#5262 = CARTESIAN_POINT ( 'NONE',  ( -69.85430415644619018, -289.1237833571632905, -202.7746430608542312 ) ) ;
#5263 = CARTESIAN_POINT ( 'NONE',  ( -81.46536161355449224, -277.4522125437222826, -209.6502380899620448 ) ) ;
#5264 = DIRECTION ( 'NONE',  ( 0.000000000000000000, 0.000000000000000000, 1.000000000000000000 ) ) ;
#5265 = CARTESIAN_POINT ( 'NONE',  ( 20.66185906647868009, -286.9773011838267962, -315.3560944145764324 ) ) ;
#5266 = CARTESIAN_POINT ( 'NONE',  ( 196.4642207764701141, 42.34395110402748941, 11.30645871156049687 ) ) ;
#5267 = CARTESIAN_POINT ( 'NONE',  ( -31.74690424450655257, -286.9815068649705836, -345.2041627897999092 ) ) ;
#5268 = CARTESIAN_POINT ( 'NONE',  ( -106.9677340600781719, -274.3903420936792372, -246.2173164837208788 ) ) ;
#5269 = CARTESIAN_POINT ( 'NONE',  ( 24.64004677047517688, -283.5747196372540770, -315.0696793122694999 ) ) ;
#5271 = CARTESIAN_POINT ( 'NONE',  ( -10.97576954368039281, -282.6987544827048282, -338.4869961247281367 ) ) ;
#5270 = CARTESIAN_POINT ( 'NONE',  ( -86.37251689046662761, -295.3960015251328173, -213.0701010210297284 ) ) ;
#5272 = CARTESIAN_POINT ( 'NONE',  ( -107.1654792193143209, -296.3033935784346227, -302.8209374198731325 ) ) ;
#5273 = CARTESIAN_POINT ( 'NONE',  ( -19.14332126376245924, -275.7161078297808672, -199.0047371827268989 ) ) ;
#5274 = ADVANCED_FACE ( 'NONE', ( #55032 ), #61675, .T. ) ;
#5275 = CARTESIAN_POINT ( 'NONE',  ( -28.48707960741623779, -282.1645066143585154, -195.8334127119177595 ) ) ;
#5276 = CARTESIAN_POINT ( 'NONE',  ( -62.12130349818226449, -272.6425182354039976, -201.3669346750759814 ) ) ;
#5277 = ORIENTED_EDGE ( 'NONE', *, *, #5180, .T. ) ;
#5278 = FACE_OUTER_BOUND ( 'NONE', #81442, .T. ) ;
#5279 = CARTESIAN_POINT ( 'NONE',  ( -90.85932714116731290, -287.2685433942630766, -218.2512526014591288 ) ) ;
#5280 = CARTESIAN_POINT ( 'NONE',  ( 164.2231345125756263, 275.0000000000000568, 7.500000000000000000 ) ) ;
#5281 = CARTESIAN_POINT ( 'NONE',  ( -72.08107566293803359, -280.9809262143061233, -342.4248175857292154 ) ) ;
#5282 = CARTESIAN_POINT ( 'NONE',  ( 22.50877645201168775, -275.3967288862177725, -318.5698841057868549 ) ) ;
#5283 = CARTESIAN_POINT ( 'NONE',  ( -96.68008155568388418, -288.3042699592049871, -318.1875266655496830 ) ) ;
#5284 = CARTESIAN_POINT ( 'NONE',  ( 1.482886347176642916, -284.0435842339068699, -333.0574373803631261 ) ) ;
#5285 = CARTESIAN_POINT ( 'NONE',  ( 36.49962194794189685, -277.1681676833748611, -271.5780437319207863 ) ) ;
#5286 = CARTESIAN_POINT ( 'NONE',  ( -90.01868687429387705, -285.2038171771376369, -325.7847237581958098 ) ) ;
#5287 = CARTESIAN_POINT ( 'NONE',  ( -64.21496463350074180, -282.2056965375770119, -338.6616169552266342 ) ) ;
#5288 = CARTESIAN_POINT ( 'NONE',  ( -41.17828725710715787, -282.0040053105010998, -195.4593072585497566 ) ) ;
#5289 = CARTESIAN_POINT ( 'NONE',  ( 25.32566527835263415, -275.1259179101189147, -225.5970684731211122 ) ) ;
#5290 = CARTESIAN_POINT ( 'NONE',  ( -5.286710171318011575, -276.4751811931974430, -340.3716716398613471 ) ) ;
#5291 = CARTESIAN_POINT ( 'NONE',  ( -95.04353818618180583, -297.8192248956215167, -317.4110504620380198 ) ) ;
#5292 = AXIS2_PLACEMENT_3D ( 'NONE', #52984, #39682, #88956 ) ;
#5293 = DIRECTION ( 'NONE',  ( -1.000000000000000000, 0.000000000000000000, 0.000000000000000000 ) ) ;
#5294 = DIRECTION ( 'NONE',  ( 0.000000000000000000, 0.000000000000000000, 1.000000000000000000 ) ) ;
#5295 = CARTESIAN_POINT ( 'NONE',  ( -110.0370414881171683, -294.4190859538852010, -291.7538915127541941 ) ) ;
#5296 = CARTESIAN_POINT ( 'NONE',  ( 32.57345518704996579, -275.3409294778575713, -291.6143659916387492 ) ) ;
#5297 = CARTESIAN_POINT ( 'NONE',  ( -107.7188072567710719, -274.1460712722865765, -239.9767597071144678 ) ) ;
#5298 = CARTESIAN_POINT ( 'NONE',  ( -70.45564045160305966, -287.3696726531240984, -204.1545245047784647 ) ) ;
#5299 = CARTESIAN_POINT ( 'NONE',  ( -4.780657072364705940, -296.1512011368319577, -339.3862285684300559 ) ) ;
#5300 = CARTESIAN_POINT ( 'NONE',  ( 34.08680801337862931, -295.1096635732735649, -298.0374064336642164 ) ) ;
#5301 = CARTESIAN_POINT ( 'NONE',  ( -110.7318267556138380, -292.3632559638281236, -285.0524782475109760 ) ) ;
#5302 = CARTESIAN_POINT ( 'NONE',  ( -19.06268687909400938, -278.2876494363108009, -197.7409463991642440 ) ) ;
#5303 = CARTESIAN_POINT ( 'NONE',  ( -107.6156734240441040, -280.1501799898020408, -295.0709707241914543 ) ) ;
#5304 = CARTESIAN_POINT ( 'NONE',  ( -50.75420014284742365, -293.3046590848770165, -343.5828295067826730 ) ) ;
#5305 = CARTESIAN_POINT ( 'NONE',  ( -103.3293793018332138, -285.9203687504344202, -307.6954243731157703 ) ) ;
#5306 = VECTOR ( 'NONE', #67620, 1000.000000000000000 ) ;
#5307 = CARTESIAN_POINT ( 'NONE',  ( -110.1815076175084585, -283.3579237937252060, -279.0815336135114535 ) ) ;
#5308 = CARTESIAN_POINT ( 'NONE',  ( -110.0473503940864930, -271.6917881263019012, -296.1273617737030577 ) ) ;
#5309 = ORIENTED_EDGE ( 'NONE', *, *, #18425, .F. ) ;
#5310 = CARTESIAN_POINT ( 'NONE',  ( -91.53406346403252769, -284.9202847882768310, -221.3452768021823260 ) ) ;
#5311 = VERTEX_POINT ( 'NONE', #19052 ) ;
#5312 = CARTESIAN_POINT ( 'NONE',  ( 38.87396411916250116, -282.5189526487523608, -261.3724883060169759 ) ) ;
#5313 = CARTESIAN_POINT ( 'NONE',  ( -54.22054209415002646, -274.1626177260037025, -199.3175244602573173 ) ) ;
#5314 = CARTESIAN_POINT ( 'NONE',  ( 7.324919880927524218, -285.4406511824274730, -208.0631346806515580 ) ) ;
#5315 = CARTESIAN_POINT ( 'NONE',  ( 36.75474168312183565, -282.2408048821324087, -250.2479611428562976 ) ) ;
#5316 = CLOSED_SHELL ( 'NONE', ( #16904, #77878, #27736, #81055, #54993, #32744, #82438, #11721, #85857, #23548, #86851, #61439, #15694, #44495, #51695, #4491, #81785, #83365, #7003, #77991 ) ) ;
#5317 = CARTESIAN_POINT ( 'NONE',  ( -38.51471153295933902, -278.5867254522245844, -346.6587706291866198 ) ) ;
#5318 = CARTESIAN_POINT ( 'NONE',  ( -39.59259826508326796, -280.6760255355429194, -193.4829674633712386 ) ) ;
#5319 = CARTESIAN_POINT ( 'NONE',  ( 7.399455738971487229, -273.9094976428776818, -326.5171145203363494 ) ) ;
#5320 = CARTESIAN_POINT ( 'NONE',  ( 181.2799904727868352, 253.4939824462867364, -166.7132491217169843 ) ) ;
#5321 = ORIENTED_EDGE ( 'NONE', *, *, #12669, .T. ) ;
#5322 = CARTESIAN_POINT ( 'NONE',  ( -2.071526431276085933, -276.5204772860475373, -204.3607901335707595 ) ) ;
#5323 = CARTESIAN_POINT ( 'NONE',  ( -71.73047451313226475, -195.8125573074262320, -360.1139850430408842 ) ) ;
#5324 = CARTESIAN_POINT ( 'NONE',  ( -82.25794907317636273, -277.4564258351906574, -210.6776309431293157 ) ) ;
#5325 = CARTESIAN_POINT ( 'NONE',  ( 25.64026602020151557, -294.7435763937052116, -227.7568810026740493 ) ) ;
#5326 = CARTESIAN_POINT ( 'NONE',  ( -15.57036931152944348, -294.1115582714140260, -340.1990432870587142 ) ) ;
#5327 = CARTESIAN_POINT ( 'NONE',  ( -47.72887221007668046, -291.4312438399701364, -194.0732959488273650 ) ) ;
#5328 = CARTESIAN_POINT ( 'NONE',  ( 201.0776230153480526, -142.7221692137691775, -8.778910157967986905 ) ) ;
#5330 = CARTESIAN_POINT ( 'NONE',  ( 14.63249618918095329, -286.7051889140808498, -322.7550425499727567 ) ) ;
#5329 = CARTESIAN_POINT ( 'NONE',  ( -113.7485848359758052, -295.1365963688830902, -269.5902350348989103 ) ) ;
#5331 = CARTESIAN_POINT ( 'NONE',  ( -27.97356497270183340, -294.0326162983287759, -196.6677879158840483 ) ) ;
#5332 = CARTESIAN_POINT ( 'NONE',  ( -102.1986019281562506, -285.3981382085561904, -305.0356372421797460 ) ) ;
#5333 = ORIENTED_EDGE ( 'NONE', *, *, #71135, .T. ) ;
#5334 = CARTESIAN_POINT ( 'NONE',  ( -94.54400060558164398, -292.1899173502172857, -219.1681786911219945 ) ) ;
#5335 = CARTESIAN_POINT ( 'NONE',  ( -7.222384578328121307, -283.1384495367122440, -336.9392131542515472 ) ) ;
#5336 = CARTESIAN_POINT ( 'NONE',  ( -70.64916894309862982, -294.2765031386915666, -339.3583148291201042 ) ) ;
#5337 = CARTESIAN_POINT ( 'NONE',  ( -96.46119502493560560, -292.0165304725848614, -221.2587668399353333 ) ) ;
#5338 = EDGE_CURVE ( 'NONE', #44839, #52563, #47502, .T. ) ;
#5339 = CARTESIAN_POINT ( 'NONE',  ( -109.8054730980372824, -290.7160977664470920, -296.3749465954792868 ) ) ;
#5340 = CARTESIAN_POINT ( 'NONE',  ( 2.445237189648779452, -286.7686396996656981, -209.1565460669851575 ) ) ;
#5341 = VERTEX_POINT ( 'NONE', #4832 ) ;
#5342 = CARTESIAN_POINT ( 'NONE',  ( 221.8344101925596306, 35.72494958537217968, -7.000000000000000888 ) ) ;
#5343 = CARTESIAN_POINT ( 'NONE',  ( -61.18008840841613249, -297.2186916809318973, -342.3328296288072465 ) ) ;
#5344 = CARTESIAN_POINT ( 'NONE',  ( -89.26126760057414344, -296.0247453402004680, -214.0963366250190916 ) ) ;
#5345 = EDGE_CURVE ( 'NONE', #87746, #70449, #23319, .T. ) ;
#5346 = CARTESIAN_POINT ( 'NONE',  ( -34.29156781518683772, -279.1501475899522120, -197.1767831543928367 ) ) ;
#5347 = CARTESIAN_POINT ( 'NONE',  ( 39.25667566103889783, -274.9625749795221168, -262.5927961482430533 ) ) ;
#5348 = CARTESIAN_POINT ( 'NONE',  ( -110.4212285597121053, -295.1610837239347802, -260.4848094460849666 ) ) ;
#5349 = CARTESIAN_POINT ( 'NONE',  ( -0.8426005758628622999, -278.4228405349111881, -335.0620155825519646 ) ) ;
#5350 = CARTESIAN_POINT ( 'NONE',  ( 36.32890189270359116, -273.8155789671689035, -279.9082986004372060 ) ) ;
#5351 = CARTESIAN_POINT ( 'NONE',  ( -39.68643072259058613, -296.2872962933840313, -343.7332287316596080 ) ) ;
#5352 = CARTESIAN_POINT ( 'NONE',  ( -110.5216669720627323, -297.6889654293551644, -266.0115748391735337 ) ) ;
#5353 = CARTESIAN_POINT ( 'NONE',  ( 194.5881128153457098, 0.000000000000000000, 21.50000000000000000 ) ) ;
#5354 = CARTESIAN_POINT ( 'NONE',  ( -65.29090283272493878, -297.0115294369232402, -341.2644173104876586 ) ) ;
#5355 = CARTESIAN_POINT ( 'NONE',  ( -48.66797751146319939, -295.9082238656515074, -196.0002937002164742 ) ) ;
#5356 = CARTESIAN_POINT ( 'NONE',  ( -14.82287014040335826, -293.0031986035471050, -200.8140478502934343 ) ) ;
#5357 = CARTESIAN_POINT ( 'NONE',  ( -27.02833669220459711, -274.9827864666995083, -194.1645582188364472 ) ) ;
#5358 = CARTESIAN_POINT ( 'NONE',  ( -98.78156256493859644, -289.6852307859175539, -229.7652793455930009 ) ) ;
#5359 = CARTESIAN_POINT ( 'NONE',  ( 175.2296996224750103, 142.2541816238762920, 0.000000000000000000 ) ) ;
#5360 = CARTESIAN_POINT ( 'NONE',  ( -93.13186485208019860, -273.7692995974663859, -217.3609085561436132 ) ) ;
#5361 = CARTESIAN_POINT ( 'NONE',  ( -109.8249371968531847, -296.7634263136923778, -279.6127325257144207 ) ) ;
#5362 = CARTESIAN_POINT ( 'NONE',  ( -68.02635420380981657, -281.6312122117402623, -201.5221955242890601 ) ) ;
#5363 = CARTESIAN_POINT ( 'NONE',  ( 36.00108747718874014, -280.5140070920198241, -292.3178449648257811 ) ) ;
#5364 = CARTESIAN_POINT ( 'NONE',  ( -59.64338359323848948, -276.6822308723493506, -343.9542406296511672 ) ) ;
#5365 = CARTESIAN_POINT ( 'NONE',  ( -31.11855801764535556, -278.5292702933902547, -194.3635146443127155 ) ) ;
#5366 = CARTESIAN_POINT ( 'NONE',  ( -8.760165897447723893, -280.6790647664868743, -339.9369770354172715 ) ) ;
#5367 = CARTESIAN_POINT ( 'NONE',  ( -3.820204120759785216, -273.0780751921286651, -204.8360230235449819 ) ) ;
#5368 = CARTESIAN_POINT ( 'NONE',  ( -66.06938119186142444, -279.4282279167829302, -339.6548854248234193 ) ) ;
#5369 = DIRECTION ( 'NONE',  ( 0.000000000000000000, 0.000000000000000000, 1.000000000000000000 ) ) ;
#5370 = CARTESIAN_POINT ( 'NONE',  ( -74.94434090351494149, -232.1443419142230766, 25.50000000000000000 ) ) ;
#5371 = CARTESIAN_POINT ( 'NONE',  ( -86.78567027478609930, -295.6157171324484239, -212.5919637838878202 ) ) ;
#5372 = CARTESIAN_POINT ( 'NONE',  ( -81.93038353165945864, -291.4628157562380579, -207.5849337059135564 ) ) ;
#5373 = CARTESIAN_POINT ( 'NONE',  ( 18.53191428103235694, -278.2515910845187364, -320.6612753712871040 ) ) ;
#5374 = CARTESIAN_POINT ( 'NONE',  ( 33.00276351448015077, -273.2143846640282163, -244.3484848610641222 ) ) ;
#5375 = CARTESIAN_POINT ( 'NONE',  ( 175.2296996224750103, 133.0000000000000000, 0.000000000000000000 ) ) ;
#5376 = CARTESIAN_POINT ( 'NONE',  ( -47.04672718844631873, -285.0946683416601672, -345.2952667143387089 ) ) ;
#5377 = B_SPLINE_CURVE_WITH_KNOTS ( 'NONE', 3,
 ( #82823, #54881, #69107, #18916 ),
 .UNSPECIFIED., .F., .F.,
 ( 4, 4 ),
 ( 0.000000000000000000, 0.0006906318969024608651 ),
 .UNSPECIFIED. ) ;
#5378 = CARTESIAN_POINT ( 'NONE',  ( -47.80257052418233599, -229.5268262511776527, 25.50000000000000000 ) ) ;
#5379 = CARTESIAN_POINT ( 'NONE',  ( 14.13724810170774049, -284.7744174194888842, -215.7481882933411725 ) ) ;
#5380 = CIRCLE ( 'NONE', #59782, 2.999999999999999112 ) ;
#5381 = CARTESIAN_POINT ( 'NONE',  ( 206.2573329513795670, 29.95202539821489296, 13.98713712351915994 ) ) ;
#5382 = CARTESIAN_POINT ( 'NONE',  ( 34.45278755785228242, -292.5479999952818844, -285.6752637591023358 ) ) ;
#5383 = CARTESIAN_POINT ( 'NONE',  ( 0.8236945865196418914, -284.7061900439438773, -206.6280435039859640 ) ) ;
#5384 = CARTESIAN_POINT ( 'NONE',  ( -108.4555765497910471, -262.4588243622614527, -317.8183916042563055 ) ) ;
#5385 = CARTESIAN_POINT ( 'NONE',  ( -73.09996504551138230, -293.5259162875414063, -336.3026119318203655 ) ) ;
#5386 = CARTESIAN_POINT ( 'NONE',  ( 17.86340071275525077, -285.3044799336849451, -217.6056316480299131 ) ) ;
#5387 = CARTESIAN_POINT ( 'NONE',  ( -30.20508680632367771, -281.7439312431374674, -196.8560815410151008 ) ) ;
#5388 = CARTESIAN_POINT ( 'NONE',  ( -15.54122839912241361, -287.5331199298364027, -196.8706820252133127 ) ) ;
#5389 = CARTESIAN_POINT ( 'NONE',  ( 17.08460742235845942, -280.5294678211956239, -323.4622253411221777 ) ) ;
#5390 = CARTESIAN_POINT ( 'NONE',  ( 21.17348472762059330, -288.1647967497415266, -314.0280409378009381 ) ) ;
#5391 = CARTESIAN_POINT ( 'NONE',  ( -109.4683650643524686, -280.1692941665662033, -255.6991640077160355 ) ) ;
#5392 = CARTESIAN_POINT ( 'NONE',  ( 9.371802247482049708, -281.5159353667501705, -213.9883327953642436 ) ) ;
#5393 = CARTESIAN_POINT ( 'NONE',  ( -86.69220583825989479, -287.3504050384118500, -213.3452500646500596 ) ) ;
#5394 = ORIENTED_EDGE ( 'NONE', *, *, #33276, .T. ) ;
#5395 = CARTESIAN_POINT ( 'NONE',  ( -70.72712248506790900, -297.4572214226643609, -200.9751426086801303 ) ) ;
#5396 = CARTESIAN_POINT ( 'NONE',  ( -111.3339271812367741, -292.6640637999180967, -260.1280646640802843 ) ) ;
#5397 = CARTESIAN_POINT ( 'NONE',  ( 206.7023069086528722, 36.31764626557887965, 13.94198228246500904 ) ) ;
#5398 = CARTESIAN_POINT ( 'NONE',  ( -19.05039376806008633, -291.3376638359844719, -350.3538533559490702 ) ) ;
#5399 = ORIENTED_EDGE ( 'NONE', *, *, #80495, .F. ) ;
#5400 = CARTESIAN_POINT ( 'NONE',  ( -77.83203036665101138, -271.5094251223428046, -207.0321231828860391 ) ) ;
#5401 = CARTESIAN_POINT ( 'NONE',  ( 196.9298236971690415, 73.03079864117960085, 12.41428257208146668 ) ) ;
#5402 = CARTESIAN_POINT ( 'NONE',  ( -100.9715923828847650, -294.3939081936653679, -312.3812434406018497 ) ) ;
#5403 = CARTESIAN_POINT ( 'NONE',  ( -104.4700245547546444, -272.2906577436394855, -241.2901558669481119 ) ) ;
#5404 = CARTESIAN_POINT ( 'NONE',  ( -20.95653174262839968, -290.3581722686908506, -342.2098062619330676 ) ) ;
#5405 = CARTESIAN_POINT ( 'NONE',  ( 36.14870698110495084, -283.4320157171180767, -279.5622748089360243 ) ) ;
#5406 = CARTESIAN_POINT ( 'NONE',  ( -89.07908564030039145, -291.1882201889321209, -326.5914410473200178 ) ) ;
#5407 = CARTESIAN_POINT ( 'NONE',  ( -38.89327520837697705, -290.3864045160495948, -346.8522343896697748 ) ) ;
#5408 = CARTESIAN_POINT ( 'NONE',  ( -93.02270218098389876, -287.2533497275067020, -220.0391129598299926 ) ) ;
#5409 = CARTESIAN_POINT ( 'NONE',  ( -1.137313172042173637, -280.6857841603659836, -202.4034666866361079 ) ) ;
#5410 = CARTESIAN_POINT ( 'NONE',  ( -76.35998312317518355, -293.6489906156095344, -335.1281645716942990 ) ) ;
#5411 = CARTESIAN_POINT ( 'NONE',  ( -18.92045261105681320, -282.6547958653488308, -345.1800883678939726 ) ) ;
#5412 = CARTESIAN_POINT ( 'NONE',  ( 36.87735890785094028, -277.3924924266790981, -268.8129728632264914 ) ) ;
#5413 = CARTESIAN_POINT ( 'NONE',  ( -69.91165696735023971, -300.1233781216987495, -202.8022627189028810 ) ) ;
#5414 = CARTESIAN_POINT ( 'NONE',  ( 22.70334180902946741, -274.4223787587929451, -316.9500878260288346 ) ) ;
#5415 = DIRECTION ( 'NONE',  ( -0.000000000000000000, 1.000000000000000000, 0.000000000000000000 ) ) ;
#5416 = CARTESIAN_POINT ( 'NONE',  ( 24.17887476714351180, -281.6056657105210661, -309.8648626097793226 ) ) ;
#5417 = CARTESIAN_POINT ( 'NONE',  ( -72.64397219414360052, -278.7140798856932520, -338.3592596393396548 ) ) ;
#5418 = CARTESIAN_POINT ( 'NONE',  ( -64.45284291391246256, -284.7655590847701319, -198.5291267034803013 ) ) ;
#5419 = CARTESIAN_POINT ( 'NONE',  ( -25.26553288692907984, -293.9682054081092701, -197.2874221465583844 ) ) ;
#5420 = CARTESIAN_POINT ( 'NONE',  ( -85.32047880293654885, -275.0018201955659265, -211.1624929118229090 ) ) ;
#5421 = CARTESIAN_POINT ( 'NONE',  ( -69.93698448296969161, -274.9470042999743669, -201.1308603885958348 ) ) ;
#5422 = LINE ( 'NONE', #41357, #59082 ) ;
#5423 = CARTESIAN_POINT ( 'NONE',  ( 35.69880132918699189, -275.4016435397434179, -271.5870845242342853 ) ) ;
#5424 = CARTESIAN_POINT ( 'NONE',  ( -109.7368646091377542, -298.3076993834943096, -289.3581808543477791 ) ) ;
#5425 = CARTESIAN_POINT ( 'NONE',  ( -112.1526875629296711, -282.5090842962747502, -273.6950319864021708 ) ) ;
#5426 = CARTESIAN_POINT ( 'NONE',  ( -40.62726875816204597, -291.6786425977870181, -193.4392316050483771 ) ) ;
#5427 = CARTESIAN_POINT ( 'NONE',  ( 34.44875389110028863, -273.3057524237379425, -249.7317006916813966 ) ) ;
#5428 = CARTESIAN_POINT ( 'NONE',  ( 2.776458437701260440, -290.1239836843585636, -335.2070805235773037 ) ) ;
#5429 = CARTESIAN_POINT ( 'NONE',  ( -91.89402461993891791, -290.1706027301854078, -221.3702116796339965 ) ) ;
#5430 = ORIENTED_EDGE ( 'NONE', *, *, #44800, .T. ) ;
#5431 = CARTESIAN_POINT ( 'NONE',  ( -1.067456681578598188, -291.0987168241476297, -203.1094595924608086 ) ) ;
#5432 = CARTESIAN_POINT ( 'NONE',  ( -109.2968560456548346, -290.3866207179117964, -257.6409832619119697 ) ) ;
#5433 = VERTEX_POINT ( 'NONE', #85313 ) ;
#5434 = CARTESIAN_POINT ( 'NONE',  ( 35.65775334262585972, -288.9286167610696339, -293.8679744847405573 ) ) ;
#5435 = CARTESIAN_POINT ( 'NONE',  ( -69.75349940843321406, -279.9464838182449853, -204.9136165103991516 ) ) ;
#5436 = CARTESIAN_POINT ( 'NONE',  ( -70.68595502335614356, -294.4018871641715123, -339.4382465362657513 ) ) ;
#5437 = CARTESIAN_POINT ( 'NONE',  ( -40.82017651476156317, -286.6610198230948185, -193.4896414072865127 ) ) ;
#5438 = CARTESIAN_POINT ( 'NONE',  ( -104.0242643699765068, -285.3867409809321316, -231.7949971845740720 ) ) ;
#5439 = CARTESIAN_POINT ( 'NONE',  ( -18.72615083281375803, -283.1391653318508475, -341.0219569492464871 ) ) ;
#5440 = CARTESIAN_POINT ( 'NONE',  ( -63.77599425757506424, -182.7598565315317671, -362.4607550793396626 ) ) ;
#5441 = CARTESIAN_POINT ( 'NONE',  ( -108.4164688561979517, -260.9275896293593178, -316.9037050568759923 ) ) ;
#5442 = CARTESIAN_POINT ( 'NONE',  ( -83.63476906808553224, -218.2911303493422395, -349.0134962854843934 ) ) ;
#5443 = CARTESIAN_POINT ( 'NONE',  ( 34.28152331167102318, -274.5520784815808497, -255.3762593438608235 ) ) ;
#5444 = CARTESIAN_POINT ( 'NONE',  ( 32.80819680017828688, -274.7537000723331744, -291.6935245946856980 ) ) ;
#5445 = CARTESIAN_POINT ( 'NONE',  ( -111.9105587548108787, -295.8219239643988772, -289.3619402754126213 ) ) ;
#5446 = CARTESIAN_POINT ( 'NONE',  ( 38.24303543357504509, -274.0868555633581991, -258.4340045478792831 ) ) ;
#5447 = CARTESIAN_POINT ( 'NONE',  ( -79.44974825397535767, -275.2353816569271316, -209.4310739421757717 ) ) ;
#5448 = ORIENTED_EDGE ( 'NONE', *, *, #53477, .T. ) ;
#5449 = CARTESIAN_POINT ( 'NONE',  ( -106.3072007313882068, -297.9276384897456182, -236.6479167282529943 ) ) ;
#5450 = AXIS2_PLACEMENT_3D ( 'NONE', #84225, #35468, #92738 ) ;
#5451 = CARTESIAN_POINT ( 'NONE',  ( 24.29362433334187088, -288.5864708224853530, -309.5921671675813514 ) ) ;
#5452 = CARTESIAN_POINT ( 'NONE',  ( -113.9606668629597124, -297.4360301119655219, -263.8942465129169364 ) ) ;
#5453 = CARTESIAN_POINT ( 'NONE',  ( -84.14279676444506606, -296.1682557354691880, -331.4953327629798991 ) ) ;
#5454 = CARTESIAN_POINT ( 'NONE',  ( 19.34444822530857877, -293.0678533609273586, -224.3448204923146818 ) ) ;
#5455 = ORIENTED_EDGE ( 'NONE', *, *, #35541, .T. ) ;
#5456 = CARTESIAN_POINT ( 'NONE',  ( 23.30912041543534485, -276.8616581992542933, -225.2968065162450557 ) ) ;
#5457 = ADVANCED_FACE ( 'NONE', ( #55509 ), #65740, .F. ) ;
#5458 = CARTESIAN_POINT ( 'NONE',  ( 3.794371498737300730, -280.0973272094233266, -205.2801054081666621 ) ) ;
#5459 = CARTESIAN_POINT ( 'NONE',  ( -18.94630583136317625, -277.7507182464654534, -341.2484787464994156 ) ) ;
#5460 = CARTESIAN_POINT ( 'NONE',  ( -10.72386229093856613, -276.1545851966166651, -199.1330697768378855 ) ) ;
#5461 = CARTESIAN_POINT ( 'NONE',  ( -67.08314674709232861, -275.4602061078032875, -339.5987750625994295 ) ) ;
#5462 = CARTESIAN_POINT ( 'NONE',  ( -33.81423868219317086, -298.7488730663218917, -197.2587812560099394 ) ) ;
#5463 = CARTESIAN_POINT ( 'NONE',  ( -72.42131744404025540, -294.1007116034472233, -335.0654981178685148 ) ) ;
#5464 = CARTESIAN_POINT ( 'NONE',  ( -36.75932130260467545, -280.5516329904406234, -193.4118253768584452 ) ) ;
#5465 = CARTESIAN_POINT ( 'NONE',  ( 31.26249086718059544, -276.0530131352813896, -295.4572700622679804 ) ) ;
#5466 = CARTESIAN_POINT ( 'NONE',  ( -33.73372242345659799, -284.7814962261444975, -193.9393882819498174 ) ) ;
#5467 = CARTESIAN_POINT ( 'NONE',  ( -106.2502911651721433, -274.9410280725825828, -240.6221293452589123 ) ) ;
#5468 = CARTESIAN_POINT ( 'NONE',  ( 197.2116943569230045, 249.5000000000000568, -12.92446933126075592 ) ) ;
#5469 = CARTESIAN_POINT ( 'NONE',  ( 27.80657692643085355, -286.2966790643522472, -236.9581922654245432 ) ) ;
#5470 = CARTESIAN_POINT ( 'NONE',  ( -3.869513343373986114, -278.7397397698162536, -204.3350128375695647 ) ) ;
#5472 = CARTESIAN_POINT ( 'NONE',  ( -85.81768114545829462, -281.8094876236396544, -326.8535374694505435 ) ) ;
#5471 = CARTESIAN_POINT ( 'NONE',  ( -72.39452319863323737, -278.1533155698182895, -205.6566010391548218 ) ) ;
#5473 = CARTESIAN_POINT ( 'NONE',  ( 34.36810695736087240, -289.2670677736219318, -248.2169718605323681 ) ) ;
#5474 = CARTESIAN_POINT ( 'NONE',  ( -87.35494975445554644, -278.9736733063753604, -324.0808105156456236 ) ) ;
#5475 = LINE ( 'NONE', #32930, #77517 ) ;
#5476 = CARTESIAN_POINT ( 'NONE',  ( -73.73139976847886601, -293.5691591426621585, -204.7807061948793717 ) ) ;
#5477 = CARTESIAN_POINT ( 'NONE',  ( -34.35367924942621443, -275.2549317083983169, -346.2890163253703690 ) ) ;
#5478 = CARTESIAN_POINT ( 'NONE',  ( 33.34287402041501025, -276.4494048833050783, -289.0047132877681975 ) ) ;
#5479 = CARTESIAN_POINT ( 'NONE',  ( 37.78819233731191218, -283.5824370664340108, -272.7122202209787361 ) ) ;
#5480 = FACE_OUTER_BOUND ( 'NONE', #18708, .T. ) ;
#5481 = CARTESIAN_POINT ( 'NONE',  ( -45.83908004566023209, -291.0790993861033371, -345.4939320029951091 ) ) ;
#5482 = CARTESIAN_POINT ( 'NONE',  ( -88.63569068191966949, -295.3328101065662281, -215.5740016657954072 ) ) ;
#5483 = CARTESIAN_POINT ( 'NONE',  ( -43.64280885152134459, -285.1717589438429172, -193.7282419513626053 ) ) ;
#5484 = CARTESIAN_POINT ( 'NONE',  ( 7.645911783477549406, -273.3659203075015398, -212.2460747401012497 ) ) ;
#5485 = CARTESIAN_POINT ( 'NONE',  ( -5.490531708281201517, -290.6152415047042155, -203.2921336742650169 ) ) ;
#5486 = CARTESIAN_POINT ( 'NONE',  ( 196.3627624770896034, 41.61148439004283262, 13.79125661931971969 ) ) ;
#5487 = DIRECTION ( 'NONE',  ( -1.000000000000000000, 0.000000000000000000, 0.000000000000000000 ) ) ;
#5488 = CARTESIAN_POINT ( 'NONE',  ( -71.84132664023964310, -290.0844397742574188, -202.2843013960701626 ) ) ;
#5489 = CARTESIAN_POINT ( 'NONE',  ( -98.18041534171183571, -285.5759949885751325, -312.2244383742435048 ) ) ;
#5490 = CARTESIAN_POINT ( 'NONE',  ( -29.54433916542513927, -284.3894837741799506, -194.7755692647185128 ) ) ;
#5491 = CARTESIAN_POINT ( 'NONE',  ( -71.46745531407400165, -287.0173803292636308, -205.1628990541616702 ) ) ;
#5492 = CARTESIAN_POINT ( 'NONE',  ( -39.98997923783336716, -286.8208628645006684, -197.2475874624307437 ) ) ;
#5493 = CARTESIAN_POINT ( 'NONE',  ( -106.8596758165687959, -292.9099816220318644, -241.2809210038930701 ) ) ;
#5494 = CARTESIAN_POINT ( 'NONE',  ( 15.92245980209379397, -274.3848484328967174, -324.0274687671739002 ) ) ;
#5495 = CARTESIAN_POINT ( 'NONE',  ( -2.730813788030802325, -276.9404789673832852, -339.1350159257519863 ) ) ;
#5496 = CARTESIAN_POINT ( 'NONE',  ( 29.63407067054737709, -291.1708336987174448, -235.2689848466014837 ) ) ;
#5497 = CARTESIAN_POINT ( 'NONE',  ( -97.69689608917815349, -279.1919871590289404, -222.5463679518675235 ) ) ;
#5498 = CARTESIAN_POINT ( 'NONE',  ( -34.20745176364884088, -296.9924347345354363, -344.9400915079979768 ) ) ;
#5499 = CARTESIAN_POINT ( 'NONE',  ( -43.54160339317981965, -248.0334966641277106, -474.9586982258124408 ) ) ;
#5500 = CARTESIAN_POINT ( 'NONE',  ( 210.8848006936870263, 293.9636489450776367, -40.00000000000000711 ) ) ;
#5501 = CARTESIAN_POINT ( 'NONE',  ( -106.6443321494666492, -282.9118259216588740, -294.9747467497087428 ) ) ;
#5502 = ADVANCED_FACE ( 'NONE', ( #48375 ), #36974, .T. ) ;
#5503 = CARTESIAN_POINT ( 'NONE',  ( -3.275213607004501259, -278.5018131557751531, -203.5300427465863891 ) ) ;
#5504 = EDGE_CURVE ( 'NONE', #50614, #65076, #6717, .T. ) ;
#5505 = CARTESIAN_POINT ( 'NONE',  ( 152.4536156746142410, 275.0000000000000568, 14.50000000000000000 ) ) ;
#5506 = CARTESIAN_POINT ( 'NONE',  ( -35.52075116320298065, -272.5544647369757740, -194.0631673642092210 ) ) ;
#5507 = CARTESIAN_POINT ( 'NONE',  ( -45.92829389768586879, -276.5123475911731248, -343.0077035009559836 ) ) ;
#5508 = AXIS2_PLACEMENT_3D ( 'NONE', #74702, #17413, #53373 ) ;
#5509 = CARTESIAN_POINT ( 'NONE',  ( 25.02425220122042404, -295.6105815909129433, -309.7150785287620351 ) ) ;
#5510 = CARTESIAN_POINT ( 'NONE',  ( 36.30673496341573525, -280.2026744850689397, -248.9270851843121193 ) ) ;
#5511 = CARTESIAN_POINT ( 'NONE',  ( -4.219553271621838242, -295.5456506989467584, -335.6923256632015864 ) ) ;
#5512 = CARTESIAN_POINT ( 'NONE',  ( -30.61750492614311270, -296.2839782419682706, -346.5719011530021589 ) ) ;
#5513 = CARTESIAN_POINT ( 'NONE',  ( -108.5545752497937002, -272.4318502960808246, -254.2113841215606840 ) ) ;
#5514 = CARTESIAN_POINT ( 'NONE',  ( -109.3217578038006508, -292.8241350142209853, -249.2471933768260897 ) ) ;
#5515 = CARTESIAN_POINT ( 'NONE',  ( -3.491271147477023717, -286.6533402012302076, -201.1862804223633532 ) ) ;
#5516 = CARTESIAN_POINT ( 'NONE',  ( 28.87963451420861816, -273.2055822605782964, -233.4423032827533859 ) ) ;
#5517 = CARTESIAN_POINT ( 'NONE',  ( 32.86400680427562548, -287.7894348986568502, -301.9864040462904313 ) ) ;
#5518 = CARTESIAN_POINT ( 'NONE',  ( -41.15997995227332495, -281.9837402886147970, -195.8140352522186447 ) ) ;
#5519 = CARTESIAN_POINT ( 'NONE',  ( -102.4420922380332115, -284.0654762150477382, -236.8149200678552120 ) ) ;
#5520 = CARTESIAN_POINT ( 'NONE',  ( -111.6801955450985417, -288.6844786863240415, -260.0426056375736152 ) ) ;
#5521 = CARTESIAN_POINT ( 'NONE',  ( 197.2116108777964030, 281.1590520725322335, -110.1526527170710921 ) ) ;
#5522 = CARTESIAN_POINT ( 'NONE',  ( -49.42553807858669046, -285.4017234780982903, -198.2542556404781635 ) ) ;
#5523 = CARTESIAN_POINT ( 'NONE',  ( 155.7883889513938698, 17.75303870060442790, 10.69672886740308648 ) ) ;
#5524 = CARTESIAN_POINT ( 'NONE',  ( 38.43750813057442883, -282.6482423518629048, -282.7042943749214032 ) ) ;
#5525 = CARTESIAN_POINT ( 'NONE',  ( -88.48377956138980949, -290.4142143431329828, -213.1133414004349902 ) ) ;
#5526 = CARTESIAN_POINT ( 'NONE',  ( -113.4133967445942659, -280.2081394517334729, -265.9410062684237346 ) ) ;
#5527 = CARTESIAN_POINT ( 'NONE',  ( -113.8847771688643604, -279.8874608218376352, -268.7613794830327834 ) ) ;
#5528 = CARTESIAN_POINT ( 'NONE',  ( 29.31359241368011581, -281.7877946511563323, -300.2521860480696887 ) ) ;
#5529 = CARTESIAN_POINT ( 'NONE',  ( -21.53673754881911506, -276.2549749414772009, -197.0453365742241374 ) ) ;
#5530 = CARTESIAN_POINT ( 'NONE',  ( -11.05720881478716677, -294.7189562055155534, -342.7925829689958164 ) ) ;
#5531 = CARTESIAN_POINT ( 'NONE',  ( -69.70849848579398156, -289.6440886384245346, -203.0845556857270822 ) ) ;
#5532 = CARTESIAN_POINT ( 'NONE',  ( -83.42806130488330041, -272.1987623064530908, -213.2368865471187291 ) ) ;
#5533 = ORIENTED_EDGE ( 'NONE', *, *, #8883, .F. ) ;
#5534 = CARTESIAN_POINT ( 'NONE',  ( -15.69077336091294050, -284.6899837677090090, -341.5829655140714749 ) ) ;
#5535 = CARTESIAN_POINT ( 'NONE',  ( -88.51969505725719500, -295.4605489573743853, -322.5176916312478284 ) ) ;
#5536 = CARTESIAN_POINT ( 'NONE',  ( 1.531509762563444621, -293.6382648281865499, -204.1916902035282249 ) ) ;
#5537 = CARTESIAN_POINT ( 'NONE',  ( 1.162039982135356198, -283.1750155104984970, -332.5600293800106897 ) ) ;
#5538 = CARTESIAN_POINT ( 'NONE',  ( 11.64478784276426460, -273.7713977941410235, -211.1892083145288268 ) ) ;
#5539 = CARTESIAN_POINT ( 'NONE',  ( -101.6033493867251707, -291.7605700994229778, -228.0310465856279620 ) ) ;
#5540 = CARTESIAN_POINT ( 'NONE',  ( -73.01021708519841980, -283.7246118193895654, -203.4594523454158264 ) ) ;
#5541 = CARTESIAN_POINT ( 'NONE',  ( -89.47404530119399624, -290.0964049248355536, -326.9999993115879988 ) ) ;
#5542 = EDGE_CURVE ( 'NONE', #10842, #84959, #82323, .T. ) ;
#5543 = CARTESIAN_POINT ( 'NONE',  ( 32.68904205201485524, -287.6113037408824198, -249.6341109729900438 ) ) ;
#5544 = CARTESIAN_POINT ( 'NONE',  ( 199.0034008648431154, 66.39839742806377387, 8.059598887640509801 ) ) ;
#5545 = DIRECTION ( 'NONE',  ( -0.000000000000000000, -0.000000000000000000, -1.000000000000000000 ) ) ;
#5546 = CARTESIAN_POINT ( 'NONE',  ( 184.5454089206492370, 260.5126890106757855, -150.9870170413777259 ) ) ;
#5547 = CARTESIAN_POINT ( 'NONE',  ( -70.15427116186016576, -284.9966942577644318, -339.2669782279853052 ) ) ;
#5548 = CARTESIAN_POINT ( 'NONE',  ( -85.33152481854864391, -287.1952119285919025, -330.4860931364850671 ) ) ;
#5549 = ORIENTED_EDGE ( 'NONE', *, *, #15094, .T. ) ;
#5550 = CARTESIAN_POINT ( 'NONE',  ( -4.701833389319127754, -281.5320240312600504, -336.0030647383991322 ) ) ;
#5551 = CARTESIAN_POINT ( 'NONE',  ( -25.77733502521724063, -276.5753990247985712, -346.4663724083969782 ) ) ;
#5552 = CARTESIAN_POINT ( 'NONE',  ( -103.4652757070050484, -280.0867013984362188, -305.3996849660924227 ) ) ;
#5553 = CARTESIAN_POINT ( 'NONE',  ( 195.3697669529573488, 276.2562599343855823, -124.8324474917287006 ) ) ;
#5554 = CARTESIAN_POINT ( 'NONE',  ( 33.01622799889876347, -280.5106917123473522, -300.3016712754254058 ) ) ;
#5555 = CARTESIAN_POINT ( 'NONE',  ( -95.38547903890790280, -283.2216319223433629, -223.4072294020228071 ) ) ;
#5556 = CARTESIAN_POINT ( 'NONE',  ( -105.0445240052205520, -297.8607417579097500, -304.9777072601681880 ) ) ;
#5557 = CARTESIAN_POINT ( 'NONE',  ( 10.96680164365356092, -293.2341867575362926, -215.4823279046650555 ) ) ;
#5558 = ORIENTED_EDGE ( 'NONE', *, *, #18406, .T. ) ;
#5559 = CARTESIAN_POINT ( 'NONE',  ( -106.5022732242845365, -288.9081005424685600, -295.2219024927940723 ) ) ;
#5560 = CARTESIAN_POINT ( 'NONE',  ( -54.10094124125617299, -277.9131764608919752, -345.4652725364228445 ) ) ;
#5561 = CARTESIAN_POINT ( 'NONE',  ( 51.66713944345190157, -299.3636508086932508, -197.3585598630277786 ) ) ;
#5562 = VERTEX_POINT ( 'NONE', #28040 ) ;
#5563 = CARTESIAN_POINT ( 'NONE',  ( -103.9541965870423610, -271.9692864156799601, -232.2510524344049827 ) ) ;
#5564 = CARTESIAN_POINT ( 'NONE',  ( 200.9306832106270804, -324.2391364535881735, 0.000000000000000000 ) ) ;
#5565 = FACE_OUTER_BOUND ( 'NONE', #867, .T. ) ;
#5566 = DIRECTION ( 'NONE',  ( 1.000000000000000000, 0.000000000000000000, 0.000000000000000000 ) ) ;
#5567 = CARTESIAN_POINT ( 'NONE',  ( 19.60080703926609758, -283.2825294796509183, -316.5520791792329760 ) ) ;
#5568 = CARTESIAN_POINT ( 'NONE',  ( -17.28136713122432155, -282.0677492029905693, -197.0702109645048665 ) ) ;
#5569 = CARTESIAN_POINT ( 'NONE',  ( -107.2139281121345391, -283.3210610690902627, -292.2992173708490213 ) ) ;
#5570 = CARTESIAN_POINT ( 'NONE',  ( -5.042114974350710987, -282.3424049903294986, -203.5209931847413145 ) ) ;
#5571 = CARTESIAN_POINT ( 'NONE',  ( 34.56557363288298035, -274.2435064169627026, -286.5445526688300788 ) ) ;
#5572 = CARTESIAN_POINT ( 'NONE',  ( 156.4217629211117355, 119.0463968525363327, -10.00000000000000000 ) ) ;
#5573 = FACE_OUTER_BOUND ( 'NONE', #17555, .T. ) ;
#5574 = CARTESIAN_POINT ( 'NONE',  ( -93.20954401653233390, -278.6324439859234303, -323.1910615350674334 ) ) ;
#5575 = ORIENTED_EDGE ( 'NONE', *, *, #29965, .T. ) ;
#5576 = ORIENTED_EDGE ( 'NONE', *, *, #18516, .T. ) ;
#5577 = CARTESIAN_POINT ( 'NONE',  ( 209.8744251295252354, 28.03846817292548366, 12.09245862095555601 ) ) ;
#5578 = CARTESIAN_POINT ( 'NONE',  ( -51.95856947680374560, -287.7275685084561587, -195.9661374918085812 ) ) ;
#5579 = CARTESIAN_POINT ( 'NONE',  ( 32.78679680666646590, -292.4719532717985544, -249.3395017370283142 ) ) ;
#5580 = CARTESIAN_POINT ( 'NONE',  ( 28.81182572348724591, -287.4122070779985165, -309.5660131331752609 ) ) ;
#5581 = CARTESIAN_POINT ( 'NONE',  ( -57.65122327509429567, -284.0263095083828375, -199.1354727095479404 ) ) ;
#5583 = CARTESIAN_POINT ( 'NONE',  ( -95.76408712385619992, -288.1603795956080489, -315.8216589771979557 ) ) ;
#5582 = CARTESIAN_POINT ( 'NONE',  ( -110.1930058801434313, -283.2629078724136775, -259.9658225330260279 ) ) ;
#5584 = CARTESIAN_POINT ( 'NONE',  ( -109.0561512620158595, -285.9630169080711539, -254.6765096224464173 ) ) ;
#5585 = CARTESIAN_POINT ( 'NONE',  ( 31.18187667383045891, -273.9515086906824308, -300.8491495366205868 ) ) ;
#5586 = CARTESIAN_POINT ( 'NONE',  ( -35.15060753806464788, -284.4790774039164489, -194.1796169645465966 ) ) ;
#5587 = CARTESIAN_POINT ( 'NONE',  ( -81.80590019574881921, -299.4471366300478508, -209.8984327494680997 ) ) ;
#5588 = CARTESIAN_POINT ( 'NONE',  ( -82.16179362472456660, -283.4427157186805175, -209.9539736317233292 ) ) ;
#5589 = CARTESIAN_POINT ( 'NONE',  ( 25.33145975030688390, -281.9723805651395310, -232.3750943571965593 ) ) ;
#5590 = CARTESIAN_POINT ( 'NONE',  ( 36.96916418498377510, -289.4063156126323975, -258.9652657521698416 ) ) ;
#5591 = DIRECTION ( 'NONE',  ( -1.000000000000000000, -1.187938636348916367E-11, 0.000000000000000000 ) ) ;
#5592 = FACE_BOUND ( 'NONE', #39839, .T. ) ;
#5593 = CARTESIAN_POINT ( 'NONE',  ( -55.69637267576413109, -297.2067866202677351, -343.6579132117065569 ) ) ;
#5594 = CARTESIAN_POINT ( 'NONE',  ( -52.19930863203599358, -277.8619052777128218, -196.7943546940425961 ) ) ;
#5595 = CARTESIAN_POINT ( 'NONE',  ( -113.9523537845118426, -289.6670009002696702, -276.9295910252459407 ) ) ;
#5596 = CARTESIAN_POINT ( 'NONE',  ( -34.28826986981983538, -293.4129927498764800, -344.0979268381724978 ) ) ;
#5597 = CARTESIAN_POINT ( 'NONE',  ( -62.46187359309388398, -278.4033222996719132, -201.2406237979824368 ) ) ;
#5598 = CARTESIAN_POINT ( 'NONE',  ( -107.6587733648807017, -270.9506206393151615, -245.9311485109034265 ) ) ;
#5599 = CARTESIAN_POINT ( 'NONE',  ( 23.74187897336652497, -294.3035887487042146, -229.4949970229460234 ) ) ;
#5600 = CARTESIAN_POINT ( 'NONE',  ( 35.77081079830085031, -295.8376638359844719, -253.6410175316879361 ) ) ;
#5601 = CARTESIAN_POINT ( 'NONE',  ( -80.21928799503250218, -295.9632749307266408, -207.1769181385298566 ) ) ;
#5602 = CARTESIAN_POINT ( 'NONE',  ( -76.27365832938465928, -291.1822484104104092, -333.0567561500868692 ) ) ;
#5603 = CARTESIAN_POINT ( 'NONE',  ( 28.60743337927727126, -291.2950960221364767, -232.6161076970519730 ) ) ;
#5604 = CARTESIAN_POINT ( 'NONE',  ( -91.20273039443296170, -292.6927889947307904, -220.1990439280312728 ) ) ;
#5605 = FACE_OUTER_BOUND ( 'NONE', #91771, .T. ) ;
#5606 = CARTESIAN_POINT ( 'NONE',  ( -86.04412536186593741, -292.1595509056815558, -215.6973577332717582 ) ) ;
#5607 = CARTESIAN_POINT ( 'NONE',  ( 9.339199855150265961, 0.000000000000000000, 54.50000000000000711 ) ) ;
#5608 = CARTESIAN_POINT ( 'NONE',  ( -112.7836469434348601, -291.9242462224384553, -257.0749831088918427 ) ) ;
#5610 = CARTESIAN_POINT ( 'NONE',  ( 20.99380109711410114, -292.9358769336175214, -226.4752512735018684 ) ) ;
#5609 = CARTESIAN_POINT ( 'NONE',  ( 26.47219683460998851, -279.0349508923584381, -230.1859362376403340 ) ) ;
#5611 = CARTESIAN_POINT ( 'NONE',  ( 38.79472841750325074, -281.4040070335026940, -258.5155531832975839 ) ) ;
#5612 = CARTESIAN_POINT ( 'NONE',  ( -93.41904383985618665, -283.4987203639658446, -323.1163500267418272 ) ) ;
#5613 = CARTESIAN_POINT ( 'NONE',  ( 15.35681882691578970, -286.3052212947831094, -323.4920367141627935 ) ) ;
#5614 = CARTESIAN_POINT ( 'NONE',  ( 36.75417371208818196, -279.6327569679189082, -265.8150253872286726 ) ) ;
#5615 = EDGE_CURVE ( 'NONE', #39404, #68312, #44530, .T. ) ;
#5616 = CARTESIAN_POINT ( 'NONE',  ( -112.3406650238408844, -282.5570572181266584, -269.9662633438911143 ) ) ;
#5617 = CARTESIAN_POINT ( 'NONE',  ( 5.808273747023926070, -279.1054385773423974, -207.4263302586238069 ) ) ;
#5618 = CARTESIAN_POINT ( 'NONE',  ( -49.28297903664213919, -284.8238338506865830, -194.5520818110061612 ) ) ;
#5619 = CARTESIAN_POINT ( 'NONE',  ( 196.4677825244212102, 42.27466702580179714, 13.19434394796706655 ) ) ;
#5620 = CARTESIAN_POINT ( 'NONE',  ( -17.23398796873227212, -293.9160412805918554, -199.3000649083326152 ) ) ;
#5621 = CARTESIAN_POINT ( 'NONE',  ( -0.3467466184871222379, -275.9593306577713179, -203.4883343111314957 ) ) ;
#5622 = CARTESIAN_POINT ( 'NONE',  ( -93.62504108874649944, -277.5593605828123600, -316.9024582956938048 ) ) ;
#5623 = CARTESIAN_POINT ( 'NONE',  ( -79.59619065119146342, -291.6652474566738533, -205.9269059334205281 ) ) ;
#5624 = CARTESIAN_POINT ( 'NONE',  ( -66.05217311612736353, -281.5047655090019134, -340.2679799701940624 ) ) ;
#5625 = CARTESIAN_POINT ( 'NONE',  ( -88.08500906111720496, -290.3798755850584143, -217.4845594673777214 ) ) ;
#5626 = CARTESIAN_POINT ( 'NONE',  ( -105.9333337881992776, -294.9508387465737655, -239.8982049057893562 ) ) ;
#5627 = ORIENTED_EDGE ( 'NONE', *, *, #81728, .T. ) ;
#5628 = DIRECTION ( 'NONE',  ( 0.000000000000000000, 1.000000000000000000, 0.000000000000000000 ) ) ;
#5629 = CARTESIAN_POINT ( 'NONE',  ( 18.52769258985101075, -292.3914859456656359, -223.2803427217227465 ) ) ;
#5630 = LINE ( 'NONE', #56775, #9676 ) ;
#5631 = CARTESIAN_POINT ( 'NONE',  ( -37.30987171927208834, -277.5523547857346784, -200.3611179825600459 ) ) ;
#5632 = CARTESIAN_POINT ( 'NONE',  ( -108.1626175631348872, -295.2314964713905283, -300.1166098182427504 ) ) ;
#5633 = CARTESIAN_POINT ( 'NONE',  ( -11.90142943120043562, -278.5192682303486436, -198.9400814747437778 ) ) ;
#5634 = CARTESIAN_POINT ( 'NONE',  ( -95.45303081468092898, -286.5437661329399930, -220.5184870140299722 ) ) ;
#5635 = CARTESIAN_POINT ( 'NONE',  ( -30.52916995337177397, -285.9738726731947054, -197.6288951263543936 ) ) ;
#5636 = CARTESIAN_POINT ( 'NONE',  ( 3.534619097436099366, -278.0113891344436183, -331.6786055197911196 ) ) ;
#5637 = CARTESIAN_POINT ( 'NONE',  ( -67.99316172634625843, -293.4766394464046471, -338.4363924853286676 ) ) ;
#5638 = CARTESIAN_POINT ( 'NONE',  ( -109.1636528616686519, -298.5455823196704159, -252.4323348575089199 ) ) ;
#5639 = CARTESIAN_POINT ( 'NONE',  ( -83.26710060335335584, -276.4921310575663256, -327.6802575631335799 ) ) ;
#5640 = VERTEX_POINT ( 'NONE', #5328 ) ;
#5641 = DIRECTION ( 'NONE',  ( -0.000000000000000000, -1.000000000000000000, -0.000000000000000000 ) ) ;
#5642 = CARTESIAN_POINT ( 'NONE',  ( -88.59451888659819474, -295.4144670288345083, -327.8685909876565461 ) ) ;
#5643 = CARTESIAN_POINT ( 'NONE',  ( -91.62643743080401748, -291.7527655932216248, -321.3724185486800593 ) ) ;
#5644 = CARTESIAN_POINT ( 'NONE',  ( 198.7350614680270269, 66.75098366856256860, -10.35296668938369180 ) ) ;
#5645 = CARTESIAN_POINT ( 'NONE',  ( 3.678657312822051662, -289.1357101857873886, -330.9302009553198900 ) ) ;
#5646 = EDGE_LOOP ( 'NONE', ( #23340, #29843, #86455, #72923, #41393 ) ) ;
#5647 = CARTESIAN_POINT ( 'NONE',  ( -28.24096526810764018, -279.2235681044772377, -194.0843210317271144 ) ) ;
#5648 = CARTESIAN_POINT ( 'NONE',  ( -93.60921940953377884, -296.4879261976922180, -322.7950019955405310 ) ) ;
#5649 = CARTESIAN_POINT ( 'NONE',  ( -107.6609930154991588, -288.3279726715115885, -298.5657723172761848 ) ) ;
#5650 = CARTESIAN_POINT ( 'NONE',  ( 99.13515218641353499, -300.0504093806150081, -193.3746630480670206 ) ) ;
#5651 = CARTESIAN_POINT ( 'NONE',  ( 25.81307700534236815, -294.3881600115214496, -307.0157440471986661 ) ) ;
#5652 = DIRECTION ( 'NONE',  ( -1.000000000000000000, -0.000000000000000000, -0.000000000000000000 ) ) ;
#5653 = DIRECTION ( 'NONE',  ( 0.000000000000000000, 0.000000000000000000, 1.000000000000000000 ) ) ;
#5654 = CARTESIAN_POINT ( 'NONE',  ( 28.31710113668617623, -289.5833924468494729, -309.2407986387399887 ) ) ;
#5655 = CARTESIAN_POINT ( 'NONE',  ( 25.18497378105907814, -277.4090924074130839, -220.4570493818173702 ) ) ;
#5656 = CARTESIAN_POINT ( 'NONE',  ( 39.17580220988369888, -281.0028635941001767, -278.5159741764853720 ) ) ;
#5657 = CARTESIAN_POINT ( 'NONE',  ( -110.7737083985673223, -286.3668230328852360, -284.7752981819294291 ) ) ;
#5658 = CARTESIAN_POINT ( 'NONE',  ( 4.869411245364308805, -285.1846773870627203, -206.6048516756858646 ) ) ;
#5659 = CARTESIAN_POINT ( 'NONE',  ( -111.4031604879961890, -288.7289859190711354, -262.8634993035025786 ) ) ;
#5660 = CARTESIAN_POINT ( 'NONE',  ( 20.79825005036669339, -278.0769382762753708, -318.9414810605923662 ) ) ;
#5662 = CARTESIAN_POINT ( 'NONE',  ( 27.87607787754784638, -280.4516509231459622, -237.2256170099288397 ) ) ;
#5661 = CARTESIAN_POINT ( 'NONE',  ( -93.60603105028444304, -277.8925878321043683, -316.8922617546468246 ) ) ;
#5663 = CARTESIAN_POINT ( 'NONE',  ( 18.68681045751782221, -277.3488972570648343, -322.7280780940164391 ) ) ;
#5664 = CARTESIAN_POINT ( 'NONE',  ( -50.85443512913958131, -278.6781054830190669, -194.9594289408277064 ) ) ;
#5665 = CARTESIAN_POINT ( 'NONE',  ( 197.4499846583558735, 287.9957563964159704, -96.69947844503649037 ) ) ;
#5666 = CARTESIAN_POINT ( 'NONE',  ( -36.95299686282403684, -274.9981862233350398, -193.5843832884686435 ) ) ;
#5667 = CONTEXT_DEPENDENT_SHAPE_REPRESENTATION ( #42653, #87535 ) ;
#5668 = CARTESIAN_POINT ( 'NONE',  ( -48.89892632017314611, -299.3331050946438268, -194.7761668995491391 ) ) ;
#5669 = CARTESIAN_POINT ( 'NONE',  ( 35.78497577281001440, -284.2662352645559167, -287.0191576251351080 ) ) ;
#5670 = ORIENTED_EDGE ( 'NONE', *, *, #89476, .T. ) ;
#5671 = CARTESIAN_POINT ( 'NONE',  ( 82.66879183539302289, -297.9920280515540867, -193.4024536127582223 ) ) ;
#5672 = CARTESIAN_POINT ( 'NONE',  ( 33.32358271772303482, -288.3751082412466076, -250.8510212492540745 ) ) ;
#5673 = CARTESIAN_POINT ( 'NONE',  ( 23.87344923371064809, -288.7062910445437751, -225.3424606930140897 ) ) ;
#5674 = CARTESIAN_POINT ( 'NONE',  ( 35.73150017091970909, -286.9456784382553565, -273.7728471660273044 ) ) ;
#5675 = CARTESIAN_POINT ( 'NONE',  ( -114.2935439285235475, -284.0287668933531791, -272.8409890777389251 ) ) ;
#5676 = CARTESIAN_POINT ( 'NONE',  ( -67.61603537093199634, -278.0480659035180224, -203.0427954839507265 ) ) ;
#5677 = CARTESIAN_POINT ( 'NONE',  ( 9.796881287871864075, -288.5696808852056279, -213.0128868019011747 ) ) ;
#5678 = CARTESIAN_POINT ( 'NONE',  ( 20.22968872378977423, -279.3882652074225916, -224.3584774011443699 ) ) ;
#5679 = CARTESIAN_POINT ( 'NONE',  ( -110.7721878770511807, -279.8275744634916009, -273.3954129017844252 ) ) ;
#5680 = CARTESIAN_POINT ( 'NONE',  ( -9.959485904892984465, -277.1770588259588521, -338.1109694485344335 ) ) ;
#5681 = EDGE_CURVE ( 'NONE', #15573, #76413, #49075, .T. ) ;
#5682 = CARTESIAN_POINT ( 'NONE',  ( -80.33053985741152303, -288.4149961440023162, -333.8284271651554036 ) ) ;
#5683 = CARTESIAN_POINT ( 'NONE',  ( -13.46239326642392697, -283.5526043915160699, -343.3949288099326509 ) ) ;
#5684 = CARTESIAN_POINT ( 'NONE',  ( -113.5375302539641496, -284.9063148473331921, -281.4012726969455684 ) ) ;
#5685 = CARTESIAN_POINT ( 'NONE',  ( 33.32404600059935973, -281.9611809040770254, -288.7235424419137644 ) ) ;
#5686 = ORIENTED_EDGE ( 'NONE', *, *, #77753, .T. ) ;
#5687 = ORIENTED_EDGE ( 'NONE', *, *, #23115, .T. ) ;
#5688 = CARTESIAN_POINT ( 'NONE',  ( 195.4101840090182236, 19.73533033507746381, -13.33719194813488507 ) ) ;
#5689 = CARTESIAN_POINT ( 'NONE',  ( -74.10069187148681635, -293.4294371709647749, -204.1109707557360480 ) ) ;
#5690 = CARTESIAN_POINT ( 'NONE',  ( 19.06348109387202427, -291.5292691793140420, -218.6721075036340380 ) ) ;
#5691 = CARTESIAN_POINT ( 'NONE',  ( -24.54357031718447502, -273.2781073344021934, -198.2009966241897132 ) ) ;
#5692 = CARTESIAN_POINT ( 'NONE',  ( 23.08641555477721852, -293.5378020024226657, -317.9401603438001871 ) ) ;
#5693 = CARTESIAN_POINT ( 'NONE',  ( -48.18191685322902629, -287.6723078097360258, -343.3043088307907738 ) ) ;
#5694 = CARTESIAN_POINT ( 'NONE',  ( 35.91385957964418196, -291.6545582059508206, -259.7971705390189072 ) ) ;
#5695 = CARTESIAN_POINT ( 'NONE',  ( -98.43270965734657807, -291.1952627253893979, -311.0659171504086089 ) ) ;
#5696 = DIRECTION ( 'NONE',  ( 0.000000000000000000, 0.000000000000000000, -1.000000000000000000 ) ) ;
#5697 = CARTESIAN_POINT ( 'NONE',  ( -111.8241535989361921, -292.4338905136488052, -279.5842747142044118 ) ) ;
#5698 = CARTESIAN_POINT ( 'NONE',  ( -52.98236629898809724, -289.8520940846919984, -196.7865093995712868 ) ) ;
#5699 = CARTESIAN_POINT ( 'NONE',  ( 18.04964310311467912, -294.8462736330813527, -219.7774443756317169 ) ) ;
#5700 = CARTESIAN_POINT ( 'NONE',  ( -49.47226760900633735, -286.8350919067108293, -198.0857872087619569 ) ) ;
#5701 = CARTESIAN_POINT ( 'NONE',  ( 37.87700061916662264, -295.5513509968073436, -270.2857543416536714 ) ) ;
#5702 = CARTESIAN_POINT ( 'NONE',  ( 207.9682065434784022, 1.060642095945600216, -7.489249145872056701 ) ) ;
#5703 = CARTESIAN_POINT ( 'NONE',  ( 36.59983589094233736, -277.3463855304444223, -255.8333495072104142 ) ) ;
#5704 = CARTESIAN_POINT ( 'NONE',  ( -99.88304356740698609, -295.1557659750702101, -315.0908592908771197 ) ) ;
#5705 = CARTESIAN_POINT ( 'NONE',  ( -46.27922519421891678, -272.1770656965683770, -196.8893910525438571 ) ) ;
#5706 = CARTESIAN_POINT ( 'NONE',  ( -105.7560830810136565, -277.0185169427158485, -241.0219564342388594 ) ) ;
#5707 = CARTESIAN_POINT ( 'NONE',  ( -62.17841503435602135, -274.9268970051939505, -201.2939905102009561 ) ) ;
#5708 = ADVANCED_FACE ( 'NONE', ( #56451 ), #26366, .T. ) ;
#5709 = CARTESIAN_POINT ( 'NONE',  ( 19.60893185760472690, -273.4299810725545399, -219.3399212466285633 ) ) ;
#5710 = CARTESIAN_POINT ( 'NONE',  ( -78.26244330558120055, -297.0394230667206443, -331.5852901726725577 ) ) ;
#5711 = EDGE_CURVE ( 'NONE', #10872, #26346, #46011, .T. ) ;
#5712 = FACE_OUTER_BOUND ( 'NONE', #15203, .T. ) ;
#5713 = CARTESIAN_POINT ( 'NONE',  ( -110.2121295165967041, -297.4480078387508684, -263.2942035712040365 ) ) ;
#5714 = CARTESIAN_POINT ( 'NONE',  ( 200.4644824113734387, 214.9910457053126720, -2.942835885954282471 ) ) ;
#5716 = CARTESIAN_POINT ( 'NONE',  ( -91.12109969885604244, -273.0941141046508278, -220.9789011326918171 ) ) ;
#5715 = CARTESIAN_POINT ( 'NONE',  ( 35.11680370657025918, -285.3050716513362204, -249.4832955014770448 ) ) ;
#5717 = CARTESIAN_POINT ( 'NONE',  ( 0.2837910275786243997, -286.5389369130856494, -203.1648049954682449 ) ) ;
#5718 = CARTESIAN_POINT ( 'NONE',  ( -12.23463671024023469, -288.4010994954074931, -343.1863322452018679 ) ) ;
#5719 = CARTESIAN_POINT ( 'NONE',  ( -100.2411356184922653, -297.9733513908078066, -311.9532453549978754 ) ) ;
#5720 = CARTESIAN_POINT ( 'NONE',  ( -15.07091183603833606, -292.7630281916104309, -341.8581856210194019 ) ) ;
#5721 = CARTESIAN_POINT ( 'NONE',  ( 39.25156628236135248, -280.6724415336311154, -264.2267589533992123 ) ) ;
#5722 = CARTESIAN_POINT ( 'NONE',  ( -114.2704648735229114, -288.0523547857347353, -270.3284710469133074 ) ) ;
#5723 = CARTESIAN_POINT ( 'NONE',  ( 153.0292788520804663, 130.2722548028652625, 11.54371207238994934 ) ) ;
#5724 = CARTESIAN_POINT ( 'NONE',  ( -71.37040974471354104, -288.3068889793354970, -335.4074447466838933 ) ) ;
#5725 = DIRECTION ( 'NONE',  ( 1.000000000000000000, 0.000000000000000000, 0.000000000000000000 ) ) ;
#5726 = CARTESIAN_POINT ( 'NONE',  ( -4.951124841408945265, -286.6255172697171361, -338.0061568715209432 ) ) ;
#5727 = CARTESIAN_POINT ( 'NONE',  ( -58.14964194610149661, -299.3788856748544163, -199.5552568497616335 ) ) ;
#5728 = CARTESIAN_POINT ( 'NONE',  ( -40.99849454269833871, -281.4322804819817065, -194.0248019828148074 ) ) ;
#5730 = CARTESIAN_POINT ( 'NONE',  ( 32.95944695222735277, -281.8120796101092651, -290.0270458577659838 ) ) ;
#5729 = CARTESIAN_POINT ( 'NONE',  ( -88.47333119696713766, -295.3601341879847269, -214.9373793898434712 ) ) ;
#5731 = CARTESIAN_POINT ( 'NONE',  ( -103.1144836723647842, -296.1960357467776817, -310.3978629717748845 ) ) ;
#5732 = CARTESIAN_POINT ( 'NONE',  ( -40.56751366323234009, -299.5310126236279302, -196.7257506761647221 ) ) ;
#5733 = EDGE_CURVE ( 'NONE', #83883, #21738, #35116, .T. ) ;
#5734 = CARTESIAN_POINT ( 'NONE',  ( 19.53237840017119709, -282.8745502570830581, -221.4504962905907064 ) ) ;
#5735 = CARTESIAN_POINT ( 'NONE',  ( -94.84666163405515249, -272.1114295819882045, -224.8923872227141771 ) ) ;
#5736 = ORIENTED_EDGE ( 'NONE', *, *, #24919, .T. ) ;
#5737 = FACE_OUTER_BOUND ( 'NONE', #69469, .T. ) ;
#5738 = CARTESIAN_POINT ( 'NONE',  ( -33.38436722844436133, -284.9820075898539926, -344.9138041418873968 ) ) ;
#5739 = DIRECTION ( 'NONE',  ( 0.000000000000000000, 1.000000000000000000, 0.000000000000000000 ) ) ;
#5740 = CARTESIAN_POINT ( 'NONE',  ( -111.2586520408596868, -282.4809262143061233, -234.7283546768995564 ) ) ;
#5741 = CARTESIAN_POINT ( 'NONE',  ( -14.64716392923073940, -275.9626250096894182, -343.8274285040680525 ) ) ;
#5742 = CARTESIAN_POINT ( 'NONE',  ( 24.84898362760958435, -292.8573758270937901, -232.0379498484602152 ) ) ;
#5743 = CARTESIAN_POINT ( 'NONE',  ( -100.9903167747113315, -285.5672894443194991, -307.5035647269911010 ) ) ;
#5744 = CARTESIAN_POINT ( 'NONE',  ( 36.17321144128678867, -277.0604677543070125, -263.3244181971031139 ) ) ;
#5745 = CARTESIAN_POINT ( 'NONE',  ( -81.20832872910371236, -285.0603891834516048, -332.9900459075452090 ) ) ;
#5746 = CARTESIAN_POINT ( 'NONE',  ( -26.70029019215288812, -281.7088385231738243, -343.0342547923207803 ) ) ;
#5747 = CARTESIAN_POINT ( 'NONE',  ( -21.80428313474043733, -282.2513104832187878, -196.9348965000683904 ) ) ;
#5748 = CARTESIAN_POINT ( 'NONE',  ( -10.34960310997828437, -274.5613809887775005, -198.1904111299019462 ) ) ;
#5749 = CARTESIAN_POINT ( 'NONE',  ( 38.73541738247091359, -275.5383055247751258, -282.5814994750116966 ) ) ;
#5750 = CARTESIAN_POINT ( 'NONE',  ( -91.43719314619438876, -297.7492393989813309, -321.5723146638374033 ) ) ;
#5751 = PLANE ( 'NONE',  #9740 ) ;
#5752 = FACE_BOUND ( 'NONE', #81352, .T. ) ;
#5753 = CARTESIAN_POINT ( 'NONE',  ( -93.74808097261622208, -293.9941146111855801, -320.9633141822506559 ) ) ;
#5754 = VECTOR ( 'NONE', #92574, 1000.000000000000000 ) ;
#5755 = CARTESIAN_POINT ( 'NONE',  ( 28.08282000434283532, -275.5017722808886447, -302.9962290752318950 ) ) ;
#5756 = CARTESIAN_POINT ( 'NONE',  ( -11.27568569241208785, -296.2388330997546291, -342.1337832458915500 ) ) ;
#5757 = CARTESIAN_POINT ( 'NONE',  ( 35.99405036289560655, -295.0385126541833074, -292.6740819260873536 ) ) ;
#5758 = CARTESIAN_POINT ( 'NONE',  ( -89.93181438835244990, -291.7971315196407431, -323.5993402230953961 ) ) ;
#5759 =( REPRESENTATION_RELATIONSHIP ('NONE','NONE', #78428, #42162 ) REPRESENTATION_RELATIONSHIP_WITH_TRANSFORMATION ( #40666 )SHAPE_REPRESENTATION_RELATIONSHIP( ) );
#5760 = CARTESIAN_POINT ( 'NONE',  ( -95.90326972664253447, -275.9099979619981013, -316.9709816389230355 ) ) ;
#5761 = CARTESIAN_POINT ( 'NONE',  ( -111.8328312978207038, -280.4683440362146598, -270.6679211818018302 ) ) ;
#5762 = CARTESIAN_POINT ( 'NONE',  ( -110.6906650645110517, -294.7962657508849702, -257.6629471649252423 ) ) ;
#5763 = CARTESIAN_POINT ( 'NONE',  ( -3.424198218548725414, -284.4696627206279231, -338.1244018102202631 ) ) ;
#5764 = CARTESIAN_POINT ( 'NONE',  ( -107.6474953668672043, -283.7482173354496808, -249.4168986826251455 ) ) ;
#5765 = CARTESIAN_POINT ( 'NONE',  ( 199.0957512885324832, 283.1197628812451512, -111.3260668811493588 ) ) ;
#5766 = VERTEX_POINT ( 'NONE', #42203 ) ;
#5767 = CARTESIAN_POINT ( 'NONE',  ( -93.26856050096415629, -284.8854125089400782, -223.4114238867873041 ) ) ;
#5768 = ORIENTED_EDGE ( 'NONE', *, *, #15154, .F. ) ;
#5769 = CARTESIAN_POINT ( 'NONE',  ( 21.72380857055593140, -281.9715754237286092, -221.4452903483682462 ) ) ;
#5770 = CARTESIAN_POINT ( 'NONE',  ( -93.61754808071229661, -284.0590748799286303, -218.3118881252798360 ) ) ;
#5771 = CARTESIAN_POINT ( 'NONE',  ( -59.24650316674426875, -280.7165931589534580, -196.7880263238149325 ) ) ;
#5772 = CARTESIAN_POINT ( 'NONE',  ( -34.29918604931301473, -278.5346647396338540, -346.6071071368523917 ) ) ;
#5773 = CARTESIAN_POINT ( 'NONE',  ( -38.17713146789083822, -280.6933493872815006, -193.4675887256294970 ) ) ;
#5774 = CARTESIAN_POINT ( 'NONE',  ( -105.5795714935544112, -270.2666405000204009, -254.7536222014695397 ) ) ;
#5775 = CARTESIAN_POINT ( 'NONE',  ( 154.7580071528325334, 206.6321147285761128, -217.3817845441456313 ) ) ;
#5776 = CARTESIAN_POINT ( 'NONE',  ( -66.55167080091212028, -275.6688505014986390, -201.4640495272424516 ) ) ;
#5777 = CARTESIAN_POINT ( 'NONE',  ( -78.43836082823335687, -208.2269359979451906, -356.9560842802424077 ) ) ;
#5778 = CARTESIAN_POINT ( 'NONE',  ( -66.69376542947502173, -277.6858607376447026, -201.7155263566453129 ) ) ;
#5779 = CARTESIAN_POINT ( 'NONE',  ( -22.41507573805834497, -294.0007421626194173, -195.8013359161006974 ) ) ;
#5780 = CARTESIAN_POINT ( 'NONE',  ( -94.85877176721795934, -295.2654161726230200, -315.4796190505793447 ) ) ;
#5781 = CARTESIAN_POINT ( 'NONE',  ( -82.82131920756381760, -289.1634266546830077, -332.4186006212438542 ) ) ;
#5782 = CARTESIAN_POINT ( 'NONE',  ( 175.2296996224750103, 249.5000000000000568, 0.000000000000000000 ) ) ;
#5784 = CARTESIAN_POINT ( 'NONE',  ( -35.89760245871006106, -284.4704337206260902, -196.5752453565859810 ) ) ;
#5783 = CARTESIAN_POINT ( 'NONE',  ( -8.626442225939685571, -293.2585141297187192, -341.2270487516418598 ) ) ;
#5785 = CARTESIAN_POINT ( 'NONE',  ( -14.48827413641327411, -294.2120065649813228, -199.7311923199909245 ) ) ;
#5786 = CARTESIAN_POINT ( 'NONE',  ( 13.63298984349051679, -285.2614928419181410, -217.0714452925102762 ) ) ;
#5787 = CARTESIAN_POINT ( 'NONE',  ( -78.64001308422193404, -284.9366157854417452, -331.1533282075482134 ) ) ;
#5788 = ORIENTED_EDGE ( 'NONE', *, *, #250, .F. ) ;
#5789 = CARTESIAN_POINT ( 'NONE',  ( -105.7997235108398115, -291.9432418997286049, -235.5117711052858169 ) ) ;
#5790 = CARTESIAN_POINT ( 'NONE',  ( 34.54712625196881959, -282.2172714786458982, -283.4690862023936120 ) ) ;
#5791 = CARTESIAN_POINT ( 'NONE',  ( 39.25952395753014201, -292.3106952854265046, -267.4669932054571859 ) ) ;
#5792 = CARTESIAN_POINT ( 'NONE',  ( -20.52177345904916450, -289.6444253021045370, -345.3906608123761544 ) ) ;
#5793 = CARTESIAN_POINT ( 'NONE',  ( -113.0716152599298852, -290.8735520198528093, -284.0188298889467546 ) ) ;
#5794 = CARTESIAN_POINT ( 'NONE',  ( 29.96094601394658241, -287.3378921394774466, -241.9573737839068031 ) ) ;
#5795 = ORIENTED_EDGE ( 'NONE', *, *, #50231, .T. ) ;
#5796 = CARTESIAN_POINT ( 'NONE',  ( 222.4201966301864672, -0.4142135623730941463, 22.50000000000000000 ) ) ;
#5797 = CARTESIAN_POINT ( 'NONE',  ( -111.9273842800553496, -298.5817978326583102, -257.0464192749748804 ) ) ;
#5798 = CARTESIAN_POINT ( 'NONE',  ( -36.53018448292221620, -296.7469447127292597, -193.8544420277347911 ) ) ;
#5799 = CARTESIAN_POINT ( 'NONE',  ( 30.24322696499087826, -280.2337310311822307, -242.1532099189585665 ) ) ;
#5800 = ORIENTED_EDGE ( 'NONE', *, *, #20540, .T. ) ;
#5801 = CARTESIAN_POINT ( 'NONE',  ( -3.457967597231253354, -297.8145302279941120, -193.4666757322721935 ) ) ;
#5802 = CARTESIAN_POINT ( 'NONE',  ( -78.35149933882429707, -294.0945031370173410, -331.6510593981409443 ) ) ;
#5803 = CARTESIAN_POINT ( 'NONE',  ( 34.22771967064979037, -277.5579536409021557, -289.2235718302286500 ) ) ;
#5804 = CARTESIAN_POINT ( 'NONE',  ( -93.83869082295066733, -271.3655235580656608, -222.1859689139305090 ) ) ;
#5805 = CARTESIAN_POINT ( 'NONE',  ( -4.143403643652741053, -295.8094317599079659, -335.8351325582482900 ) ) ;
#5806 = CARTESIAN_POINT ( 'NONE',  ( -106.2731608860714232, -297.2990385937704900, -295.4638574129397739 ) ) ;
#5807 = CARTESIAN_POINT ( 'NONE',  ( 152.4536156746142410, 250.0000000000000568, -14.50000000000000000 ) ) ;
#5808 = CARTESIAN_POINT ( 'NONE',  ( -27.82730623010683857, -296.5335250004055752, -346.0175395129002140 ) ) ;
#5809 = CARTESIAN_POINT ( 'NONE',  ( -40.34097257410225268, -296.0145062489132215, -195.2034221697184648 ) ) ;
#5810 = CARTESIAN_POINT ( 'NONE',  ( -32.15832675795920892, -292.7706406046042957, -197.4305446049828845 ) ) ;
#5811 = CARTESIAN_POINT ( 'NONE',  ( -96.81760244974110208, -274.0096978011514466, -221.6910622589487048 ) ) ;
#5812 = CARTESIAN_POINT ( 'NONE',  ( -110.8329621990606455, -289.1881273338095184, -265.6801956808976115 ) ) ;
#5813 = CARTESIAN_POINT ( 'NONE',  ( 121.3395553409046528, -299.5541904835127980, -195.3611179825600175 ) ) ;
#5814 = CARTESIAN_POINT ( 'NONE',  ( -70.11126143934319543, -274.1243107896996776, -200.7357772458493912 ) ) ;
#5815 = CARTESIAN_POINT ( 'NONE',  ( -97.19827691613841125, -296.3024119178330693, -312.1854853061793165 ) ) ;
#5816 = CARTESIAN_POINT ( 'NONE',  ( -6.918054506879156129, -282.4292894281523445, -201.4065367525154500 ) ) ;
#5817 = CARTESIAN_POINT ( 'NONE',  ( 31.58450669542373745, -279.8069066511179130, -237.0356233251795572 ) ) ;
#5818 = CARTESIAN_POINT ( 'NONE',  ( -4.046500103412615346, -275.9731549710980403, -339.6918461529121487 ) ) ;
#5819 = CARTESIAN_POINT ( 'NONE',  ( 34.57945288242659387, -279.6293744593503448, -245.0282495480993532 ) ) ;
#5820 = CARTESIAN_POINT ( 'NONE',  ( -3.735904834450111345, -280.6097109895972039, -337.6114148401288730 ) ) ;
#5821 = EDGE_CURVE ( 'NONE', #78077, #60755, #80771, .T. ) ;
#5822 = CARTESIAN_POINT ( 'NONE',  ( -63.49933604404081677, -272.2792023331933819, -201.5641396797239793 ) ) ;
#5823 = CARTESIAN_POINT ( 'NONE',  ( -112.0611173911752303, -280.6427900891960689, -263.3147681650081040 ) ) ;
#5824 = CARTESIAN_POINT ( 'NONE',  ( 213.7238915819278589, 32.98517505407394168, 10.50000000000000000 ) ) ;
#5825 = VECTOR ( 'NONE', #37864, 1000.000000000000000 ) ;
#5826 = CARTESIAN_POINT ( 'NONE',  ( 170.2305261370685798, 275.5000000000000568, -24.90909090909090295 ) ) ;
#5827 = CARTESIAN_POINT ( 'NONE',  ( 96.97712259441328797, -297.9515605777340284, -194.4139984393089549 ) ) ;
#5828 = CARTESIAN_POINT ( 'NONE',  ( 22.68073234451026465, -290.9516883036625927, -224.7798666402447054 ) ) ;
#5829 = CARTESIAN_POINT ( 'NONE',  ( -70.89771341143497807, -291.6215903590082235, -201.0574819125283454 ) ) ;
#5830 = CARTESIAN_POINT ( 'NONE',  ( -37.10650145541197986, -279.0493349585280498, -345.5401692336875499 ) ) ;
#5831 = CARTESIAN_POINT ( 'NONE',  ( -26.98959127535904301, -272.1834772614915892, -196.0266959755703340 ) ) ;
#5832 = DIRECTION ( 'NONE',  ( 0.000000000000000000, 9.656854691831248164E-17, -1.000000000000000000 ) ) ;
#5833 = CARTESIAN_POINT ( 'NONE',  ( 29.80881533814829609, -283.9273444942072047, -305.0039017601280307 ) ) ;
#5834 = CARTESIAN_POINT ( 'NONE',  ( 9.339199855150265961, -232.1443419142230766, 25.50000000000000000 ) ) ;
#5835 = CARTESIAN_POINT ( 'NONE',  ( 18.42569466378405352, -286.2509335325852362, -320.5297634117886787 ) ) ;
#5836 = CARTESIAN_POINT ( 'NONE',  ( 175.2296996224750103, 154.6894116713782807, 24.16304133878946558 ) ) ;
#5837 = CARTESIAN_POINT ( 'NONE',  ( -18.13127116356609037, -293.5938725927802011, -341.1995956816894022 ) ) ;
#5838 = CARTESIAN_POINT ( 'NONE',  ( 34.22629246734285147, -285.4354960076999532, -250.6408766576362837 ) ) ;
#5839 = DIRECTION ( 'NONE',  ( 3.794040663998540091E-16, -1.000000000000000000, -4.956352788505168198E-16 ) ) ;
#5840 = CARTESIAN_POINT ( 'NONE',  ( 32.43722319485794259, -291.9115183176212440, -297.9967698098740243 ) ) ;
#5841 = CARTESIAN_POINT ( 'NONE',  ( -47.18625929612417735, -281.6549466116007920, -346.0300839222187506 ) ) ;
#5842 = CARTESIAN_POINT ( 'NONE',  ( -43.84163656708467016, -281.5689117503197849, -196.7971289869299198 ) ) ;
#5843 = CARTESIAN_POINT ( 'NONE',  ( -107.5682853823894902, -286.1508145804614855, -239.6304621266478989 ) ) ;
#5844 = CARTESIAN_POINT ( 'NONE',  ( 37.14769176420034569, -279.9822424444057560, -285.3712649446937348 ) ) ;
#5845 = CARTESIAN_POINT ( 'NONE',  ( 34.52168923811392176, -287.7214239878546209, -283.1928469698248705 ) ) ;
#5846 = CARTESIAN_POINT ( 'NONE',  ( -101.3330633903045737, -280.4711055189549711, -234.0227038217660152 ) ) ;
#5847 = CARTESIAN_POINT ( 'NONE',  ( -102.3039594605032931, -279.8129579991354490, -236.5980959320195609 ) ) ;
#5848 = ADVANCED_FACE ( 'NONE', ( #13362 ), #64197, .T. ) ;
#5849 = CARTESIAN_POINT ( 'NONE',  ( -18.61567453809499639, -288.2719225488984875, -197.3158088079621564 ) ) ;
#5850 = ORIENTED_EDGE ( 'NONE', *, *, #39899, .T. ) ;
#5851 = CARTESIAN_POINT ( 'NONE',  ( -9.108184373951473844, -298.2298170564640714, -193.3618857822629593 ) ) ;
#5852 = CARTESIAN_POINT ( 'NONE',  ( -99.68690915034417799, -293.0898461000305133, -229.2193848998570900 ) ) ;
#5853 = CARTESIAN_POINT ( 'NONE',  ( 222.8344101925596306, 0.000000000000000000, 22.50000000000000000 ) ) ;
#5854 = CARTESIAN_POINT ( 'NONE',  ( -115.3430155898818299, -299.2662352645559167, -252.5904736702033517 ) ) ;
#5855 = VERTEX_POINT ( 'NONE', #93342 ) ;
#5856 = CARTESIAN_POINT ( 'NONE',  ( -3.362946426965163216, -272.4995135873649588, -203.2984767044623027 ) ) ;
#5857 = CARTESIAN_POINT ( 'NONE',  ( -25.05707791679039431, -293.2980154564169197, -345.6178675202841077 ) ) ;
#5858 = CARTESIAN_POINT ( 'NONE',  ( -72.87132862955478174, -297.0754529053523925, -206.5204260980227673 ) ) ;
#5859 = CARTESIAN_POINT ( 'NONE',  ( 22.53624336083535695, -289.6671109006661595, -313.3185345365367311 ) ) ;
#5860 = PRODUCT_DEFINITION_SHAPE ( 'NONE', 'NONE',  #93717 ) ;
#5861 = CARTESIAN_POINT ( 'NONE',  ( 7.742074953156449446, -282.4370734769851765, -211.5985254147447279 ) ) ;
#5862 = CARTESIAN_POINT ( 'NONE',  ( -77.80883846843350682, -291.0092274865546642, -335.2380841106740945 ) ) ;
#5863 = CARTESIAN_POINT ( 'NONE',  ( -113.1796150786164503, -291.9992784467313527, -259.8776398959319636 ) ) ;
#5864 = CARTESIAN_POINT ( 'NONE',  ( -35.92042454816522934, -288.0701400924353948, -195.3745816696648490 ) ) ;
#5865 = CARTESIAN_POINT ( 'NONE',  ( -103.4126861797397368, -279.2356109739591261, -230.7147441718757364 ) ) ;
#5866 = CARTESIAN_POINT ( 'NONE',  ( -1.412850710840422686, -292.6594512925507274, -336.8470096827380758 ) ) ;
#5867 = CARTESIAN_POINT ( 'NONE',  ( 21.06748726530683413, -280.7080599864149235, -220.1677005407295837 ) ) ;
#5868 = CARTESIAN_POINT ( 'NONE',  ( 32.43070515813587917, -277.7464761711309507, -295.8617034362296181 ) ) ;
#5869 = EDGE_CURVE ( 'NONE', #11817, #84307, #30898, .T. ) ;
#5870 = CARTESIAN_POINT ( 'NONE',  ( -110.4542110544635705, -298.8376638359844719, -287.0812184334320705 ) ) ;
#5871 = CARTESIAN_POINT ( 'NONE',  ( 26.09706842815266725, -273.2346856866873850, -228.5341331829797298 ) ) ;
#5872 = CARTESIAN_POINT ( 'NONE',  ( 154.1415209985679269, 20.37991841447901820, -11.45812909362559040 ) ) ;
#5873 = CARTESIAN_POINT ( 'NONE',  ( 28.20350686436677279, -281.4981943882946780, -302.7530596194822579 ) ) ;
#5874 = CARTESIAN_POINT ( 'NONE',  ( -54.02971886978359350, -278.4667498916023192, -345.1785584520411021 ) ) ;
#5875 = CARTESIAN_POINT ( 'NONE',  ( -109.6177798865284672, -274.0454297395746721, -256.7689657923062327 ) ) ;
#5876 = CARTESIAN_POINT ( 'NONE',  ( -113.9161884942815277, -283.6875017427759076, -264.2549829255597160 ) ) ;
#5877 = CARTESIAN_POINT ( 'NONE',  ( -91.51597573476546188, -293.0276038846615734, -219.9129978082602292 ) ) ;
#5878 = CARTESIAN_POINT ( 'NONE',  ( -49.61072543368067045, -275.4984689368752129, -195.1020761104337851 ) ) ;
#5879 = CARTESIAN_POINT ( 'NONE',  ( -106.4052874089918106, -274.2920130612158118, -237.4442654095895193 ) ) ;
#5880 = DIRECTION ( 'NONE',  ( -0.000000000000000000, 1.000000000000000000, -0.000000000000000000 ) ) ;
#5881 = CARTESIAN_POINT ( 'NONE',  ( 20.02114368815130163, -276.0225754703945995, -315.5310451171347381 ) ) ;
#5882 = CARTESIAN_POINT ( 'NONE',  ( -104.3999815358387906, -298.1117102159607839, -303.6928239167373818 ) ) ;
#5883 = CARTESIAN_POINT ( 'NONE',  ( -110.5180462890020578, -282.3496828256400590, -286.0825592521257477 ) ) ;
#5884 = CARTESIAN_POINT ( 'NONE',  ( -61.67787143112253290, -291.4112298820096498, -197.2741960514575226 ) ) ;
#5885 = CARTESIAN_POINT ( 'NONE',  ( 31.70568001355369958, -273.1989561112062574, -241.8649895559216532 ) ) ;
#5886 = CARTESIAN_POINT ( 'NONE',  ( 19.04611703627797326, -289.8562758818808902, -321.6334080570705396 ) ) ;
#5887 = CARTESIAN_POINT ( 'NONE',  ( -109.9309595453163411, -289.3366708692947213, -280.6994902012481816 ) ) ;
#5888 = ORIENTED_EDGE ( 'NONE', *, *, #89138, .T. ) ;
#5889 = CARTESIAN_POINT ( 'NONE',  ( -111.7393844530081850, -289.3464831604720189, -252.9372589780034559 ) ) ;
#5890 = CARTESIAN_POINT ( 'NONE',  ( -87.94218381655042549, -290.9877484713275066, -217.6445101868062579 ) ) ;
#5891 = ORIENTED_EDGE ( 'NONE', *, *, #8888, .F. ) ;
#5892 = CARTESIAN_POINT ( 'NONE',  ( 39.04545297181316954, -288.5390541985246955, -262.9733086454263571 ) ) ;
#5893 = CARTESIAN_POINT ( 'NONE',  ( -93.10909541348289054, -279.5553360123302014, -223.2028849580876511 ) ) ;
#5894 = CARTESIAN_POINT ( 'NONE',  ( -81.70414139475033721, -294.5605846921813509, -332.9836907621987621 ) ) ;
#5895 = CARTESIAN_POINT ( 'NONE',  ( -66.52986655384275139, -284.0759175334835618, -341.5185463276025075 ) ) ;
#5896 = CARTESIAN_POINT ( 'NONE',  ( -104.3965106526863735, -284.3934798537279676, -308.2764333612271912 ) ) ;
#5898 = CARTESIAN_POINT ( 'NONE',  ( -16.12230466580236765, -283.1033664215912609, -340.2311741076330236 ) ) ;
#5897 = AXIS2_PLACEMENT_3D ( 'NONE', #26191, #47014, #11523 ) ;
#5899 = CARTESIAN_POINT ( 'NONE',  ( 121.5737172192837647, 149.6818241901583519, -263.5908535195870854 ) ) ;
#5900 = CARTESIAN_POINT ( 'NONE',  ( 200.5336724191271287, 293.3464715333668664, -82.97196496506106200 ) ) ;
#5901 = CARTESIAN_POINT ( 'NONE',  ( 201.2091503359040416, 293.0224724744892910, -53.99999999998772893 ) ) ;
#5902 = CARTESIAN_POINT ( 'NONE',  ( 20.14300298717034465, -275.3865259312892704, -315.6373465373062004 ) ) ;
#5903 = CARTESIAN_POINT ( 'NONE',  ( 25.54805180592470393, -273.9553379912273385, -232.5917511904098660 ) ) ;
#5904 = CARTESIAN_POINT ( 'NONE',  ( -53.28262368708350039, -294.7588242118001176, -345.6845620427292261 ) ) ;
#5905 = CARTESIAN_POINT ( 'NONE',  ( -37.97421885051181079, -140.6615534827124065, -361.4716249991672612 ) ) ;
#5906 = CARTESIAN_POINT ( 'NONE',  ( 28.08953652310458793, -273.7149588171571963, -230.6106996128995377 ) ) ;
#5907 = CARTESIAN_POINT ( 'NONE',  ( -52.91698336635150213, -299.7109788148400185, -197.7254607410615108 ) ) ;
#5908 = CARTESIAN_POINT ( 'NONE',  ( -41.62458576998787407, -293.0767583622085226, -197.1271626203962626 ) ) ;
#5909 = ORIENTED_EDGE ( 'NONE', *, *, #27071, .F. ) ;
#5910 = CARTESIAN_POINT ( 'NONE',  ( -110.5717227983794970, -297.2026739782708091, -293.4308178788953114 ) ) ;
#5911 = CARTESIAN_POINT ( 'NONE',  ( -3.332142614293172933, -289.0830067836944863, -335.0804222139351509 ) ) ;
#5912 = CARTESIAN_POINT ( 'NONE',  ( -113.6157304054386401, -297.4714964996462641, -261.0642838139588662 ) ) ;
#5913 = CARTESIAN_POINT ( 'NONE',  ( -95.53084320546444985, -296.3639744853335856, -320.6955051478072392 ) ) ;
#5914 = CARTESIAN_POINT ( 'NONE',  ( 29.85491414142531497, -293.3343197721284241, -241.7078647926716712 ) ) ;
#5915 = VERTEX_POINT ( 'NONE', #42675 ) ;
#5916 = CARTESIAN_POINT ( 'NONE',  ( 38.19072379062034628, -277.4462914734339734, -268.3197625022576176 ) ) ;
#5917 = EDGE_CURVE ( 'NONE', #86306, #83027, #68684, .T. ) ;
#5918 = ORIENTED_EDGE ( 'NONE', *, *, #33819, .F. ) ;
#5919 = CARTESIAN_POINT ( 'NONE',  ( 6.154632182364051296, -280.1330478315038022, -206.8977744003737200 ) ) ;
#5920 = CARTESIAN_POINT ( 'NONE',  ( -0.4380277963570491928, -275.4969204518833976, -207.0888539788068385 ) ) ;
#5921 = CARTESIAN_POINT ( 'NONE',  ( -21.58705511561383261, -276.0116050854931018, -196.0256273214094449 ) ) ;
#5922 = CARTESIAN_POINT ( 'NONE',  ( -95.79486251683916009, -275.9200123858412894, -317.9379783407196101 ) ) ;
#5923 = CARTESIAN_POINT ( 'NONE',  ( -37.15767395580831334, -298.7059386433933241, -197.2563104522588162 ) ) ;
#5924 = CARTESIAN_POINT ( 'NONE',  ( -66.30160080640023068, -294.0136355706548557, -338.0124230023276368 ) ) ;
#5925 = DIRECTION ( 'NONE',  ( 0.000000000000000000, 0.000000000000000000, 1.000000000000000000 ) ) ;
#5926 = CARTESIAN_POINT ( 'NONE',  ( -94.91990408976175786, -279.7364432972652821, -219.3289973929232133 ) ) ;
#5927 = CARTESIAN_POINT ( 'NONE',  ( -21.65095256143696290, -277.0121800002983150, -341.7068723450335028 ) ) ;
#5928 = CARTESIAN_POINT ( 'NONE',  ( 2.498593096772880884, -285.2593198525837579, -205.0461173462174713 ) ) ;
#5929 = CARTESIAN_POINT ( 'NONE',  ( -77.25115969597118237, -299.5185044677735959, -206.6644660885268934 ) ) ;
#5930 = CARTESIAN_POINT ( 'NONE',  ( 82.66436015057398379, -298.3400917633185827, -197.5716692144941362 ) ) ;
#5931 = CARTESIAN_POINT ( 'NONE',  ( 35.61206425292357380, -286.8301847085243708, -276.5050500214535418 ) ) ;
#5932 = CARTESIAN_POINT ( 'NONE',  ( -21.96225826316446827, -278.4916138296314330, -197.9107010581973896 ) ) ;
#5934 = CARTESIAN_POINT ( 'NONE',  ( -110.1332356122260592, -282.4296763044688987, -286.0007928923134273 ) ) ;
#5933 = CARTESIAN_POINT ( 'NONE',  ( -102.6706824402684077, -277.5852116543040893, -236.3755129093389371 ) ) ;
#5935 = CARTESIAN_POINT ( 'NONE',  ( -57.90628777537927618, -287.7868294318164430, -198.1823433619638308 ) ) ;
#5936 = CARTESIAN_POINT ( 'NONE',  ( 18.62106700892852729, -277.4288014158954070, -317.8511085088505297 ) ) ;
#5937 = DIRECTION ( 'NONE',  ( 0.000000000000000000, 0.000000000000000000, 1.000000000000000000 ) ) ;
#5938 = CARTESIAN_POINT ( 'NONE',  ( -95.91793325527721947, -293.1963925842221101, -223.5228263150655152 ) ) ;
#5939 = CARTESIAN_POINT ( 'NONE',  ( -20.37447151732715867, -275.0771153282910291, -344.4832379296491354 ) ) ;
#5940 = CARTESIAN_POINT ( 'NONE',  ( 7.386746795288989809, -275.3321910576300979, -212.5401987261823251 ) ) ;
#5941 = CARTESIAN_POINT ( 'NONE',  ( 36.62615812048505859, -283.7245304329682085, -283.8037696818990412 ) ) ;
#5942 = CARTESIAN_POINT ( 'NONE',  ( 154.5625123364532101, 250.5000000000000568, -13.15740740740742254 ) ) ;
#5943 = CARTESIAN_POINT ( 'NONE',  ( 38.16662097048998703, -289.5227957866670181, -274.3225937122457481 ) ) ;
#5944 = CARTESIAN_POINT ( 'NONE',  ( -9.808272363124412863, -292.6925230793752348, -340.1792265857679922 ) ) ;
#5945 = CARTESIAN_POINT ( 'NONE',  ( 208.3180124865313587, 30.15554586770298329, 14.31509665898690287 ) ) ;
#5946 = CARTESIAN_POINT ( 'NONE',  ( 31.58660314724305707, -273.8992607641877726, -244.8634223043338238 ) ) ;
#5947 = CARTESIAN_POINT ( 'NONE',  ( 35.93699067301943728, -291.5366098952956690, -258.4029661927262964 ) ) ;
#5948 = CARTESIAN_POINT ( 'NONE',  ( 207.9738562182569979, 296.4636489450776367, -53.99999999999996447 ) ) ;
#5949 = DIRECTION ( 'NONE',  ( 0.000000000000000000, 0.000000000000000000, 1.000000000000000000 ) ) ;
#5950 = CARTESIAN_POINT ( 'NONE',  ( -81.51314198400530131, -289.9429385321560062, -208.1390039435764834 ) ) ;
#5951 = CARTESIAN_POINT ( 'NONE',  ( 36.15847101141952891, -286.0365693578910964, -289.6406111922293007 ) ) ;
#5952 = CARTESIAN_POINT ( 'NONE',  ( -90.09784014928001739, -286.7140129219131950, -218.9833481387612721 ) ) ;
#5953 = CARTESIAN_POINT ( 'NONE',  ( -98.24714543452139992, -285.9164405738245023, -229.8255970284060936 ) ) ;
#5954 = CARTESIAN_POINT ( 'NONE',  ( -112.7440084987078279, -292.5208747485262961, -271.2353873984615689 ) ) ;
#5955 = CARTESIAN_POINT ( 'NONE',  ( 33.38267531793234610, -273.2891149986369328, -243.7645596713856264 ) ) ;
#5956 = CARTESIAN_POINT ( 'NONE',  ( 3.493883597693932419, -276.8526407094437900, -335.6787470154824291 ) ) ;
#5957 = CARTESIAN_POINT ( 'NONE',  ( -111.5067524685816664, -288.8170458532259204, -255.8418640012977221 ) ) ;
#5958 = CARTESIAN_POINT ( 'NONE',  ( 16.95522598451886154, -276.3046930662062550, -325.0326752986218821 ) ) ;
#5959 = CARTESIAN_POINT ( 'NONE',  ( -98.51724811578361596, -297.9487570645957817, -313.1325936664433129 ) ) ;
#5960 = DIRECTION ( 'NONE',  ( 0.000000000000000000, -0.000000000000000000, 1.000000000000000000 ) ) ;
#5961 = DIRECTION ( 'NONE',  ( 0.000000000000000000, 1.000000000000000000, -0.000000000000000000 ) ) ;
#5962 = CARTESIAN_POINT ( 'NONE',  ( -97.75182001462053449, -283.8164844320434099, -228.4836425946084830 ) ) ;
#5963 = CARTESIAN_POINT ( 'NONE',  ( 5.074684711517985392, -278.6254773587518798, -208.5076545095119513 ) ) ;
#5964 = CARTESIAN_POINT ( 'NONE',  ( 211.1232656141943949, 1.000000000000000888, 7.000000000000000000 ) ) ;
#5965 = CARTESIAN_POINT ( 'NONE',  ( 37.49854503773154590, -274.2199196149044838, -285.2488800054418334 ) ) ;
#5966 = CARTESIAN_POINT ( 'NONE',  ( -16.35953576138010845, -276.1224003591457290, -340.4402045645200019 ) ) ;
#5967 = CARTESIAN_POINT ( 'NONE',  ( 29.02732323551024507, -295.5030334922710722, -302.5079214175981406 ) ) ;
#5968 = CARTESIAN_POINT ( 'NONE',  ( 6.020844782299992204, -279.5458182110612597, -207.1062192951671079 ) ) ;
#5969 = CARTESIAN_POINT ( 'NONE',  ( 17.26398336829361568, -295.1894305148285298, -319.1819527188986285 ) ) ;
#5970 = EDGE_CURVE ( 'NONE', #54214, #85888, #50249, .T. ) ;
#5971 = CARTESIAN_POINT ( 'NONE',  ( -65.40690521778019217, -296.7266210566795053, -341.5485748630854914 ) ) ;
#5972 = CARTESIAN_POINT ( 'NONE',  ( -109.9063062625910874, -272.3263847655838390, -262.2084850772610025 ) ) ;
#5973 = CARTESIAN_POINT ( 'NONE',  ( -111.6860408655634842, -292.6843288238685545, -260.0795071766720525 ) ) ;
#5974 = CARTESIAN_POINT ( 'NONE',  ( -104.0415186784035200, -285.2201666703302863, -231.7825687038794626 ) ) ;
#5975 = CARTESIAN_POINT ( 'NONE',  ( -10.75844407506960110, -272.5346119203353510, -199.3571753994172582 ) ) ;
#5976 = CARTESIAN_POINT ( 'NONE',  ( 0.2856448581120792918, -286.3722837850887117, -203.1658430544205487 ) ) ;
#5977 = CARTESIAN_POINT ( 'NONE',  ( -102.2543164025909732, -281.0256360975375287, -233.5073658163543939 ) ) ;
#5978 = ADVANCED_FACE ( 'NONE', ( #85767 ), #32451, .T. ) ;
#5979 = CARTESIAN_POINT ( 'NONE',  ( -2.062546817588094328, -285.5898173759450742, -206.1264164768845433 ) ) ;
#5980 = CARTESIAN_POINT ( 'NONE',  ( -51.33771324277528691, -287.2309533507367973, -344.0436278660727680 ) ) ;
#5981 = CARTESIAN_POINT ( 'NONE',  ( -110.2140734402150315, -271.0703965937372004, -283.6296548450457635 ) ) ;
#5982 = CARTESIAN_POINT ( 'NONE',  ( -37.27452594576047318, -285.5606305738032802, -197.2871612464168720 ) ) ;
#5983 = CARTESIAN_POINT ( 'NONE',  ( -34.47571799833898609, -283.9581991348520660, -347.0723059537602921 ) ) ;
#5984 = CARTESIAN_POINT ( 'NONE',  ( -73.31281617031996234, -290.6457803915457703, -202.5310819535010012 ) ) ;
#5985 = CARTESIAN_POINT ( 'NONE',  ( -113.4320613315310311, -280.1006389850841174, -274.4473565415793246 ) ) ;
#5986 = CARTESIAN_POINT ( 'NONE',  ( -110.0860468285261504, -280.1692626991464294, -246.4956362764479820 ) ) ;
#5987 = CARTESIAN_POINT ( 'NONE',  ( 13.33662947264594933, -280.6182732636815444, -217.7482428526018339 ) ) ;
#5988 = CARTESIAN_POINT ( 'NONE',  ( 36.68530665664987822, -277.7109644365514782, -282.7172801949819814 ) ) ;
#5989 = CARTESIAN_POINT ( 'NONE',  ( -95.58149718973983511, -295.8717068608051477, -320.7310101624807430 ) ) ;
#5990 = CARTESIAN_POINT ( 'NONE',  ( -99.49386711827017393, -288.0108085991494704, -311.7239071073950072 ) ) ;
#5991 = CARTESIAN_POINT ( 'NONE',  ( -108.1305717749185646, -295.7236991369195493, -251.2559772775269096 ) ) ;
#5992 = ORIENTED_EDGE ( 'NONE', *, *, #89368, .F. ) ;
#5993 = CARTESIAN_POINT ( 'NONE',  ( 22.17568282459027529, -284.0881698145445853, -315.0923159870245627 ) ) ;
#5994 = CARTESIAN_POINT ( 'NONE',  ( -68.53022372016609154, -295.1402955790632632, -336.4003295392051314 ) ) ;
#5995 = CARTESIAN_POINT ( 'NONE',  ( 37.75640112553596595, -294.4357669153371262, -254.7479280267220929 ) ) ;
#5996 = CARTESIAN_POINT ( 'NONE',  ( -7.203884436192401708, -283.2974898235943897, -336.9751873970264455 ) ) ;
#5997 = CARTESIAN_POINT ( 'NONE',  ( -27.01626463977208203, -273.2389828234658466, -194.2407382155091398 ) ) ;
#5998 = CARTESIAN_POINT ( 'NONE',  ( -110.6821137467765084, -290.9106764461627108, -293.6541972034444257 ) ) ;
#5999 = CARTESIAN_POINT ( 'NONE',  ( -23.98007752674210380, -284.3605149886851677, -195.7304757717481607 ) ) ;
#6000 = CARTESIAN_POINT ( 'NONE',  ( -94.69838580893468816, -291.5820447233759865, -219.0195665913088590 ) ) ;
#6001 = CARTESIAN_POINT ( 'NONE',  ( 23.54934965867307639, -287.3253151340538238, -229.9661372154001242 ) ) ;
#6002 = DIRECTION ( 'NONE',  ( 0.000000000000000000, 0.000000000000000000, 1.000000000000000000 ) ) ;
#6003 = CYLINDRICAL_SURFACE ( 'NONE', #90095, 4.025000000000000355 ) ;
#6004 = CARTESIAN_POINT ( 'NONE',  ( -88.43586288902518788, -229.5806346048500473, -344.3981502665915286 ) ) ;
#6005 = CARTESIAN_POINT ( 'NONE',  ( -73.92639662551032131, -285.0487258973328721, -337.3847428240234763 ) ) ;
#6006 = CARTESIAN_POINT ( 'NONE',  ( 35.78497577281001440, -290.8380690714490129, -253.7030783399848985 ) ) ;
#6007 = EDGE_LOOP ( 'NONE', ( #87173, #92982 ) ) ;
#6008 = CARTESIAN_POINT ( 'NONE',  ( -83.62228263375395443, -278.3204874543079654, -213.4418079053755548 ) ) ;
#6009 = CARTESIAN_POINT ( 'NONE',  ( -39.96648372379942060, -276.7509731606716059, -347.3082744206993766 ) ) ;
#6010 = CARTESIAN_POINT ( 'NONE',  ( -51.60601112674886792, -279.2352042535546275, -343.8223857041643328 ) ) ;
#6011 = CARTESIAN_POINT ( 'NONE',  ( 169.3709080288175528, 229.8928499549132880, -190.9150157918655282 ) ) ;
#6012 = CARTESIAN_POINT ( 'NONE',  ( -17.13024629461648374, -278.8828484576725373, -196.6718825045445271 ) ) ;
#6013 = CARTESIAN_POINT ( 'NONE',  ( -46.91130203267351106, -283.9502742395509927, -196.2803571052962184 ) ) ;
#6014 = CARTESIAN_POINT ( 'NONE',  ( -110.6089248337608950, -298.0565533206940927, -290.5077752547692285 ) ) ;
#6015 = CARTESIAN_POINT ( 'NONE',  ( 3.856251671994097574, -294.9729584840727057, -330.6994740175380798 ) ) ;
#6016 = ORIENTED_EDGE ( 'NONE', *, *, #53259, .F. ) ;
#6017 = CARTESIAN_POINT ( 'NONE',  ( -60.39789375266617100, -290.4317752692833778, -200.5248081682064765 ) ) ;
#6018 = CARTESIAN_POINT ( 'NONE',  ( -21.38404973707247692, -274.9030555115559196, -195.1370116052208630 ) ) ;
#6019 = CARTESIAN_POINT ( 'NONE',  ( -109.8857675254993609, -272.6596122241019771, -262.2150584787953562 ) ) ;
#6020 = VERTEX_POINT ( 'NONE', #49786 ) ;
#6021 = CARTESIAN_POINT ( 'NONE',  ( 200.8419735307467420, 26.78103457774642138, 10.49999999999999822 ) ) ;
#6022 = DIRECTION ( 'NONE',  ( 1.000000000000000000, 0.000000000000000000, 0.000000000000000000 ) ) ;
#6023 = CONICAL_SURFACE ( 'NONE', #34740, 24.00000000000001066, 0.7446590313522313265 ) ;
#6024 = LINE ( 'NONE', #86004, #72995 ) ;
#6025 = CARTESIAN_POINT ( 'NONE',  ( 34.05833804426701050, -282.4134863947147664, -253.7400282558174354 ) ) ;
#6026 = CARTESIAN_POINT ( 'NONE',  ( -90.36730959580737021, -281.0746793626499311, -215.8611060414256144 ) ) ;
#6027 = CARTESIAN_POINT ( 'NONE',  ( -40.25568207211312455, -282.1484228624309480, -343.5384174535101920 ) ) ;
#6028 = CARTESIAN_POINT ( 'NONE',  ( 30.08483914091539191, -282.9990922065770178, -239.1811731680289768 ) ) ;
#6029 = CARTESIAN_POINT ( 'NONE',  ( 10.09572021311817736, -274.8639928247811213, -326.7561434895976618 ) ) ;
#6030 = EDGE_CURVE ( 'NONE', #93585, #33595, #3656, .T. ) ;
#6031 = CARTESIAN_POINT ( 'NONE',  ( 154.1415209985679269, 20.37991841447902175, 11.45812909362559040 ) ) ;
#6032 = EDGE_CURVE ( 'NONE', #1911, #61737, #79312, .T. ) ;
#6033 = LINE ( 'NONE', #79407, #63830 ) ;
#6034 = CARTESIAN_POINT ( 'NONE',  ( -108.5030311645493555, -278.9860634965922372, -299.3477318790779123 ) ) ;
#6035 = EDGE_LOOP ( 'NONE', ( #27895, #41391, #35244, #60184, #63409, #9138, #53254, #34317, #76879, #47970, #45596, #27943, #60385, #84376, #89602, #36500, #49848, #71353, #50593, #74484, #24603, #56583 ) ) ;
#6036 = ORIENTED_EDGE ( 'NONE', *, *, #73376, .F. ) ;
#6037 = LINE ( 'NONE', #56714, #26275 ) ;
#6038 = CARTESIAN_POINT ( 'NONE',  ( -112.6961097755201422, -286.5364693665569575, -270.0150740228486370 ) ) ;
#6039 = CARTESIAN_POINT ( 'NONE',  ( 34.10971757953186057, -292.5415648980221022, -254.5774852944237523 ) ) ;
#6040 = CARTESIAN_POINT ( 'NONE',  ( 24.05581056322921185, -287.5180993374442551, -316.6607774614274149 ) ) ;
#6041 = CARTESIAN_POINT ( 'NONE',  ( -106.5039957381839599, -283.1390750320503571, -244.0067847931236713 ) ) ;
#6043 = CARTESIAN_POINT ( 'NONE',  ( -31.81779088451380844, -287.2214873955384178, -344.2193569050722886 ) ) ;
#6042 = CARTESIAN_POINT ( 'NONE',  ( -70.22960506001793135, -284.1847746285217795, -204.5157583719768013 ) ) ;
#6044 = CARTESIAN_POINT ( 'NONE',  ( -1.042353637751539219, -283.7638682205783311, -334.1536563359283036 ) ) ;
#6045 = CARTESIAN_POINT ( 'NONE',  ( -2.215051817335441431, -272.5169823324737308, -204.0955973121915292 ) ) ;
#6046 = CARTESIAN_POINT ( 'NONE',  ( -57.52422196158602929, -284.1958601810950427, -196.8277348213053983 ) ) ;
#6047 = CARTESIAN_POINT ( 'NONE',  ( -98.31096105726601309, -299.1465021697725888, -226.6833218814015538 ) ) ;
#6048 = CARTESIAN_POINT ( 'NONE',  ( -57.24536142066678224, -283.7958924575103765, -197.8234864103609141 ) ) ;
#6049 = CARTESIAN_POINT ( 'NONE',  ( 0.5113351721018359886, -281.5109392116309550, -207.6082718563130811 ) ) ;
#6050 = CARTESIAN_POINT ( 'NONE',  ( 20.65888604817430263, -288.8942117181810545, -222.5493994004961564 ) ) ;
#6051 = CARTESIAN_POINT ( 'NONE',  ( 196.6877655503061533, 293.9636489450775230, -7.999911143031724237 ) ) ;
#6052 = PLANE ( 'NONE',  #74600 ) ;
#6053 = CARTESIAN_POINT ( 'NONE',  ( 12.31342757672488197, -294.6573769579096620, -213.4077819255724933 ) ) ;
#6054 = CARTESIAN_POINT ( 'NONE',  ( -62.48363449053908170, -275.3789563292572211, -341.0766793583003960 ) ) ;
#6055 = CARTESIAN_POINT ( 'NONE',  ( -98.21405665386636485, -290.3765817901110040, -223.4493740493912242 ) ) ;
#6056 = CARTESIAN_POINT ( 'NONE',  ( 10.79812279102936401, -292.7731343243028732, -326.2985639600900072 ) ) ;
#6057 = CARTESIAN_POINT ( 'NONE',  ( -95.99527464800895871, -277.8551197509483472, -226.0570361621963684 ) ) ;
#6058 = CARTESIAN_POINT ( 'NONE',  ( -69.77618293275435235, -295.7600024742189930, -203.5863487265986294 ) ) ;
#6059 = CARTESIAN_POINT ( 'NONE',  ( -84.15596269872959567, -292.7077342042797454, -213.7071834629577722 ) ) ;
#6060 = CARTESIAN_POINT ( 'NONE',  ( -106.6662871844225293, -287.4805209788416391, -237.0123917617630696 ) ) ;
#6061 = CARTESIAN_POINT ( 'NONE',  ( -96.79387123168692142, -295.6789657453386440, -222.5265373234953188 ) ) ;
#6062 = CARTESIAN_POINT ( 'NONE',  ( -91.16237061436491729, -291.4327915439585581, -320.9310281449119771 ) ) ;
#6063 = CARTESIAN_POINT ( 'NONE',  ( -39.16461470641952047, -290.2694682189896298, -194.3834529505225532 ) ) ;
#6064 = CARTESIAN_POINT ( 'NONE',  ( -84.21822483988832175, -292.8178147669369196, -213.6339961942476577 ) ) ;
#6065 = DIRECTION ( 'NONE',  ( 0.5877852522924681411, 0.000000000000000000, -0.8090169943749512260 ) ) ;
#6066 = CARTESIAN_POINT ( 'NONE',  ( -110.4075655545769195, -291.4158735341030706, -265.7355749416362301 ) ) ;
#6067 = DIRECTION ( 'NONE',  ( -0.000000000000000000, -1.000000000000000000, -0.000000000000000000 ) ) ;
#6068 = CARTESIAN_POINT ( 'NONE',  ( -100.3452413808355033, -291.1787881130031792, -313.9336151381815512 ) ) ;
#6070 = CARTESIAN_POINT ( 'NONE',  ( 35.70798575139937014, -293.5574130684050260, -270.7599229830289005 ) ) ;
#6069 = CARTESIAN_POINT ( 'NONE',  ( 36.80257838763506584, -279.7451208784507344, -283.8875015688768144 ) ) ;
#6071 = CARTESIAN_POINT ( 'NONE',  ( -7.536989558263370803, -280.4322196772617417, -199.3490738489731200 ) ) ;
#6072 = CARTESIAN_POINT ( 'NONE',  ( -0.3893175335183487462, -282.2414310786630836, -337.9057920514401872 ) ) ;
#6073 = CARTESIAN_POINT ( 'NONE',  ( -12.70781070355129039, -286.7309927970715080, -341.0236958950612802 ) ) ;
#6074 = CARTESIAN_POINT ( 'NONE',  ( 36.92364100776275393, -279.6685868693510315, -268.5771397648979359 ) ) ;
#6075 = CARTESIAN_POINT ( 'NONE',  ( -31.02620414692890449, -284.1317716819260681, -195.6145403548395052 ) ) ;
#6076 = DIRECTION ( 'NONE',  ( -1.000000000000000000, 0.000000000000000000, 0.000000000000000000 ) ) ;
#6077 = CARTESIAN_POINT ( 'NONE',  ( -53.59375983348104455, -278.3273073072952002, -195.7511693299308320 ) ) ;
#6078 = CARTESIAN_POINT ( 'NONE',  ( -70.91844213813423892, -284.5398077948256628, -201.4111730416956902 ) ) ;
#6079 = CARTESIAN_POINT ( 'NONE',  ( 35.76383957032597749, -276.4069825415440960, -274.3111788450280528 ) ) ;
#6080 = CARTESIAN_POINT ( 'NONE',  ( 195.2884072777227686, 40.74925082751602190, 14.92164996664659427 ) ) ;
#6081 = CARTESIAN_POINT ( 'NONE',  ( 7.142413368725160971, -294.2698835450690922, -211.4747523324210192 ) ) ;
#6082 = CARTESIAN_POINT ( 'NONE',  ( -4.098985192281886292, -275.9071668662159595, -201.5460815532364904 ) ) ;
#6083 = CARTESIAN_POINT ( 'NONE',  ( -109.0648539953097753, -278.0372349821024613, -284.1340162663009323 ) ) ;
#6084 = CARTESIAN_POINT ( 'NONE',  ( -109.4745867473442615, -291.0612731992603699, -243.2676167652135177 ) ) ;
#6085 = CARTESIAN_POINT ( 'NONE',  ( -87.38645428948795768, -281.8231106743042460, -327.0422776791623392 ) ) ;
#6087 = CARTESIAN_POINT ( 'NONE',  ( -41.59455453792438817, -291.0561612959225499, -197.1994036284999368 ) ) ;
#6086 = TOROIDAL_SURFACE ( 'NONE', #68125, 1.000000000000000000, 0.5000000000000000000 ) ;
#6088 = CARTESIAN_POINT ( 'NONE',  ( 29.11800313306291699, -292.0124013372352465, -305.1189730405533851 ) ) ;
#6089 = ORIENTED_EDGE ( 'NONE', *, *, #8182, .F. ) ;
#6090 = CARTESIAN_POINT ( 'NONE',  ( 150.7110049404237770, 21.00000000139189638, 5.101169899789431916 ) ) ;
#6091 = CARTESIAN_POINT ( 'NONE',  ( -34.84890870758367498, -291.5919605982918483, -197.3421174912564027 ) ) ;
#6092 = FACE_OUTER_BOUND ( 'NONE', #24257, .T. ) ;
#6093 = CIRCLE ( 'NONE', #13669, 5.000000000000004441 ) ;
#6094 = CARTESIAN_POINT ( 'NONE',  ( -105.5937364680635966, -299.2662352645559167, -254.8156830097664738 ) ) ;
#6095 = CARTESIAN_POINT ( 'NONE',  ( -110.5849994635594697, -295.9025738146879689, -247.2015414032112233 ) ) ;
#6096 = CARTESIAN_POINT ( 'NONE',  ( -111.0120537506639380, -285.6070266184644311, -291.0003347949233330 ) ) ;
#6097 = CARTESIAN_POINT ( 'NONE',  ( 33.38909083593797789, -287.1464931707760115, -252.2508900825876026 ) ) ;
#6098 = CARTESIAN_POINT ( 'NONE',  ( 36.39287900440442058, -277.0881741381935512, -271.5772722800994643 ) ) ;
#6099 = CARTESIAN_POINT ( 'NONE',  ( -109.9037581196022870, -294.3456727388120839, -287.9249344330636973 ) ) ;
#6100 = CARTESIAN_POINT ( 'NONE',  ( -76.17085491830529520, -297.3385052082472839, -333.4309437484569685 ) ) ;
#6101 = EDGE_CURVE ( 'NONE', #78927, #88979, #86695, .T. ) ;
#6102 = CARTESIAN_POINT ( 'NONE',  ( 20.32495631621481991, -274.9843479026411615, -315.7871597573177951 ) ) ;
#6103 = ORIENTED_EDGE ( 'NONE', *, *, #8199, .F. ) ;
#6104 = DIRECTION ( 'NONE',  ( 0.000000000000000000, -1.000000000000000000, 0.000000000000000000 ) ) ;
#6105 = CARTESIAN_POINT ( 'NONE',  ( -108.8673779565948792, -296.5815716677780074, -241.7605266901245500 ) ) ;
#6106 = CARTESIAN_POINT ( 'NONE',  ( 34.77770760792697757, -289.2329897729304662, -251.8677942383068000 ) ) ;
#6107 = CARTESIAN_POINT ( 'NONE',  ( -52.18709021055299502, -295.8620628868436029, -196.7927256169245993 ) ) ;
#6108 = CARTESIAN_POINT ( 'NONE',  ( 17.90801334263261069, -288.8854616061919955, -318.3050898869007597 ) ) ;
#6109 = EDGE_LOOP ( 'NONE', ( #76397, #25919, #56935, #9258 ) ) ;
#6110 = CARTESIAN_POINT ( 'NONE',  ( -82.09194440340202448, -278.5169816781325380, -207.9893627591955010 ) ) ;
#6111 = CARTESIAN_POINT ( 'NONE',  ( -99.01566137253699651, -297.8155031830853545, -224.4083719213211054 ) ) ;
#6112 = CARTESIAN_POINT ( 'NONE',  ( -106.1288864628091204, -289.1060797715368835, -238.4772942746835724 ) ) ;
#6113 = CARTESIAN_POINT ( 'NONE',  ( -114.2887788053904217, -296.9307258127167870, -266.7405081365514548 ) ) ;
#6114 = CARTESIAN_POINT ( 'NONE',  ( 34.73412790656426097, -293.7299528060083276, -258.5713172227330574 ) ) ;
#6115 = DIRECTION ( 'NONE',  ( 0.000000000000000000, 0.000000000000000000, 1.000000000000000000 ) ) ;
#6116 = PLANE ( 'NONE',  #93147 ) ;
#6117 = CYLINDRICAL_SURFACE ( 'NONE', #3810, 1.000000000000000888 ) ;
#6118 = CARTESIAN_POINT ( 'NONE',  ( 34.42704087534821866, -289.4043550773267270, -296.4370661045614384 ) ) ;
#6119 = CARTESIAN_POINT ( 'NONE',  ( -111.2869819898779866, -275.4805209788415823, -234.7871824221999191 ) ) ;
#6120 = VERTEX_POINT ( 'NONE', #23707 ) ;
#6121 = CARTESIAN_POINT ( 'NONE',  ( 39.08244059342509047, -280.7881470642360000, -261.3701320586211523 ) ) ;
#6122 = CARTESIAN_POINT ( 'NONE',  ( 13.17253473191948743, -284.3442213114847164, -325.5728966228734294 ) ) ;
#6123 = CARTESIAN_POINT ( 'NONE',  ( -7.555937486864927166, -285.0096507889122677, -199.9385999065484327 ) ) ;
#6124 = CARTESIAN_POINT ( 'NONE',  ( -107.3958357662211540, -288.3032179906163037, -295.5351577177019067 ) ) ;
#6125 = CARTESIAN_POINT ( 'NONE',  ( 36.04826454221141319, -277.6519314244757197, -289.1818132139968043 ) ) ;
#6126 = ORIENTED_EDGE ( 'NONE', *, *, #53259, .T. ) ;
#6128 = CARTESIAN_POINT ( 'NONE',  ( 34.43590914722005891, -280.7173963942254886, -256.4435106977344958 ) ) ;
#6127 = CARTESIAN_POINT ( 'NONE',  ( -103.1310101955112373, -278.1227559085914436, -302.1129792847488034 ) ) ;
#6129 = CARTESIAN_POINT ( 'NONE',  ( -34.28957869236049305, -278.0942853629294973, -346.9912495575085245 ) ) ;
#6130 = CARTESIAN_POINT ( 'NONE',  ( -40.97413401564302404, -278.8023573981167260, -193.8312331652753642 ) ) ;
#6131 = CARTESIAN_POINT ( 'NONE',  ( 159.2118730347355040, 219.5970318917149768, -203.3186411165585810 ) ) ;
#6132 = CARTESIAN_POINT ( 'NONE',  ( -111.5937896373990412, -273.7403149086202916, -250.6781500681430259 ) ) ;
#6133 = CARTESIAN_POINT ( 'NONE',  ( -113.6483667957982107, -274.0720294864290167, -270.3804296936822880 ) ) ;
#6134 = CARTESIAN_POINT ( 'NONE',  ( -110.4542110544635705, -292.8376638359844719, -287.0812184334320705 ) ) ;
#6135 = DIRECTION ( 'NONE',  ( -1.000000000000000000, -0.000000000000000000, -0.000000000000000000 ) ) ;
#6136 = CARTESIAN_POINT ( 'NONE',  ( 20.61025189801298652, -289.2616779655754726, -315.2790799315228583 ) ) ;
#6137 = CARTESIAN_POINT ( 'NONE',  ( -93.19039151972846469, -287.0238133388053257, -218.7582787028780729 ) ) ;
#6138 = CARTESIAN_POINT ( 'NONE',  ( 35.37663929389177753, -286.8022121870467913, -262.8820953351711864 ) ) ;
#6139 = CARTESIAN_POINT ( 'NONE',  ( -74.25197882986223874, -283.0365817738089618, -337.9272917728421817 ) ) ;
#6140 = CARTESIAN_POINT ( 'NONE',  ( -32.89466816449868958, -278.5089819398108375, -196.6952213770649394 ) ) ;
#6141 = CARTESIAN_POINT ( 'NONE',  ( 13.97661457833849141, -288.6414862554391334, -216.6497881114142103 ) ) ;
#6142 = CARTESIAN_POINT ( 'NONE',  ( 34.74745710294403978, -279.8314344876043265, -255.0083958591818885 ) ) ;
#6143 = ADVANCED_FACE ( 'NONE', ( #29889 ), #55095, .T. ) ;
#6144 = CARTESIAN_POINT ( 'NONE',  ( -8.530013592997137906, -277.9821581966813824, -337.9848874139491954 ) ) ;
#6145 = CARTESIAN_POINT ( 'NONE',  ( 22.32747080595033751, -275.4562334121121125, -228.1781247950915485 ) ) ;
#6146 = CARTESIAN_POINT ( 'NONE',  ( 34.69380407767113894, -286.6795964428744128, -296.5709700656075256 ) ) ;
#6147 = CARTESIAN_POINT ( 'NONE',  ( 6.840533778072469318, -283.2709493226794280, -333.2918303956634531 ) ) ;
#6148 = CARTESIAN_POINT ( 'NONE',  ( -94.34933860692810015, -284.3418476194091795, -322.0493705473210753 ) ) ;
#6149 = CARTESIAN_POINT ( 'NONE',  ( 3.391980919436260233, -282.6546167578878794, -331.0008682391191996 ) ) ;
#6150 = EDGE_LOOP ( 'NONE', ( #6583, #24016, #50242, #18562, #3814, #73236 ) ) ;
#6151 = VERTEX_POINT ( 'NONE', #51181 ) ;
#6152 = CARTESIAN_POINT ( 'NONE',  ( 156.6308165671946142, 214.7033826592484900, 16.75079304138620273 ) ) ;
#6153 = CARTESIAN_POINT ( 'NONE',  ( -75.02837810709432631, -291.4090589529651538, -336.0879753833191330 ) ) ;
#6154 = CARTESIAN_POINT ( 'NONE',  ( -50.46519167494317770, -290.5727599478697130, -194.9882300109461255 ) ) ;
#6155 = CARTESIAN_POINT ( 'NONE',  ( -40.51476382051683345, -297.2084334667812868, -197.2559056900744281 ) ) ;
#6156 = CARTESIAN_POINT ( 'NONE',  ( -4.553535239038832394, -293.9800174437330043, -339.9330909725131846 ) ) ;
#6158 = EDGE_CURVE ( 'NONE', #17753, #50862, #48627, .T. ) ;
#6157 = CIRCLE ( 'NONE', #21289, 5.000000000000004441 ) ;
#6159 = CARTESIAN_POINT ( 'NONE',  ( -37.28675259310060852, -287.5313286789786389, -344.0544333888452115 ) ) ;
#6160 = CARTESIAN_POINT ( 'NONE',  ( -9.323374709152744799, -290.6632045607491364, -201.8014872502685364 ) ) ;
#6161 = CARTESIAN_POINT ( 'NONE',  ( 3.850075219107168767, -289.6892835545980347, -331.1708110788648582 ) ) ;
#6162 = CARTESIAN_POINT ( 'NONE',  ( 199.4392256788250677, 65.82574266882504332, -7.741079165001071516 ) ) ;
#6163 = CARTESIAN_POINT ( 'NONE',  ( -102.8751189456563679, -293.0377465666505259, -233.8868576847403347 ) ) ;
#6164 = CARTESIAN_POINT ( 'NONE',  ( -100.1379850857831570, -289.1094240273696414, -228.9560795584055199 ) ) ;
#6165 = AXIS2_PLACEMENT_3D ( 'NONE', #26689, #76877, #12478 ) ;
#6166 = CARTESIAN_POINT ( 'NONE',  ( -56.43403404432657311, -293.8064119183956677, -197.7789372747151049 ) ) ;
#6167 = CARTESIAN_POINT ( 'NONE',  ( -44.05784911650182778, -286.9064072226856865, -197.4344302004051315 ) ) ;
#6168 = CARTESIAN_POINT ( 'NONE',  ( -19.83899551537457384, -294.2766665352193058, -197.2071013247608278 ) ) ;
#6169 = CARTESIAN_POINT ( 'NONE',  ( 198.5086862847412306, 68.69963673584575758, -12.80442219784223923 ) ) ;
#6170 = AXIS2_PLACEMENT_3D ( 'NONE', #6343, #77369, #64142 ) ;
#6171 = CARTESIAN_POINT ( 'NONE',  ( 153.3662726500193116, 20.33089334036130680, -12.12590166673910907 ) ) ;
#6172 = CARTESIAN_POINT ( 'NONE',  ( -38.36100491794313427, -276.0193209134464496, -195.0128079504726770 ) ) ;
#6173 = CARTESIAN_POINT ( 'NONE',  ( -114.1478250495710682, -295.7947949219372390, -266.7326872174685946 ) ) ;
#6174 = CARTESIAN_POINT ( 'NONE',  ( 35.84702391920586706, -273.6475459290978733, -259.2582025667841776 ) ) ;
#6175 = CARTESIAN_POINT ( 'NONE',  ( -111.5933069882814266, -276.7004617299519396, -265.0683800930034977 ) ) ;
#6176 = CARTESIAN_POINT ( 'NONE',  ( -37.16513218877542357, -299.3695919249173585, -196.8650551490323721 ) ) ;
#6177 = CARTESIAN_POINT ( 'NONE',  ( 9.166183792013789855, -273.2516035846269915, -209.7342013153218261 ) ) ;
#6178 = CARTESIAN_POINT ( 'NONE',  ( -109.9412787060566501, -297.8200282176399014, -282.3892561632160891 ) ) ;
#6179 = CARTESIAN_POINT ( 'NONE',  ( 192.9623460957494956, 250.0000000000000568, 16.90571646082667812 ) ) ;
#6180 = CARTESIAN_POINT ( 'NONE',  ( -86.21573634893285032, -298.1559647525178320, -215.9191276624551392 ) ) ;
#6181 = FACE_OUTER_BOUND ( 'NONE', #9022, .T. ) ;
#6183 = CARTESIAN_POINT ( 'NONE',  ( 8.928578900605470992, -298.6472714677322529, -197.3611204045932084 ) ) ;
#6182 = CARTESIAN_POINT ( 'NONE',  ( -10.55455361439076434, -284.4198379758917667, -199.8721810464378450 ) ) ;
#6184 = CARTESIAN_POINT ( 'NONE',  ( -54.96460918990257483, -285.8315914952464141, -195.4049102596583225 ) ) ;
#6185 = CARTESIAN_POINT ( 'NONE',  ( -108.7804172452479889, -289.8548615205696137, -299.0360894403287375 ) ) ;
#6186 = CARTESIAN_POINT ( 'NONE',  ( -95.23130678774714397, -297.8687555266120057, -318.6222370427543638 ) ) ;
#6187 = CARTESIAN_POINT ( 'NONE',  ( -39.77350657260084432, -293.0825783079234270, -345.1676751913112184 ) ) ;
#6188 = CARTESIAN_POINT ( 'NONE',  ( -19.78316589113467572, -279.4693761617219252, -195.5010015131282728 ) ) ;
#6189 = CARTESIAN_POINT ( 'NONE',  ( -85.33152481854862970, -287.1952119285919025, -330.4860931364851808 ) ) ;
#6190 = CYLINDRICAL_SURFACE ( 'NONE', #46878, 20.00000000000000355 ) ;
#6191 = CARTESIAN_POINT ( 'NONE',  ( -74.93237634285625859, -288.3597150576446211, -333.4161239805175114 ) ) ;
#6192 = CARTESIAN_POINT ( 'NONE',  ( 140.6539576904058606, 275.0000000000000568, 12.50000000000000000 ) ) ;
#6193 = CARTESIAN_POINT ( 'NONE',  ( -90.08517449047870684, -287.7974552631008009, -323.6820947145538980 ) ) ;
#6194 = CARTESIAN_POINT ( 'NONE',  ( -69.62569380259114382, -299.2199864273650292, -203.9970903007093170 ) ) ;
#6195 = CARTESIAN_POINT ( 'NONE',  ( -69.72926855144149272, -281.0593605385857359, -201.1395278911332696 ) ) ;
#6197 = CARTESIAN_POINT ( 'NONE',  ( -8.494241580696364480, -282.6637061493995020, -337.4194816321220287 ) ) ;
#6196 = CARTESIAN_POINT ( 'NONE',  ( -95.26367600118032897, -293.9096116816541553, -318.5833846459750021 ) ) ;
#6198 = CARTESIAN_POINT ( 'NONE',  ( -101.6270970665464972, -296.1604316727464266, -312.8413572493814740 ) ) ;
#6199 = CARTESIAN_POINT ( 'NONE',  ( -47.38622948753410213, -299.4424650463605531, -197.3038362871796210 ) ) ;
#6200 = CARTESIAN_POINT ( 'NONE',  ( 38.26126521051239138, -285.6471918085137531, -271.5534346435341604 ) ) ;
#6201 = CARTESIAN_POINT ( 'NONE',  ( 21.29529204304514423, -282.9092808645379478, -223.5785050336387485 ) ) ;
#6202 = CARTESIAN_POINT ( 'NONE',  ( -98.93767660563467814, -295.0633222878150832, -310.0689894473713935 ) ) ;
#6203 = ORIENTED_EDGE ( 'NONE', *, *, #55527, .T. ) ;
#6204 = CARTESIAN_POINT ( 'NONE',  ( 188.3531807883583440, 45.29379214021909661, 10.50000000000000000 ) ) ;
#6205 = CARTESIAN_POINT ( 'NONE',  ( 1.988922335289990295, -284.5032803419713332, -333.8639702252353345 ) ) ;
#6206 = DIRECTION ( 'NONE',  ( -0.000000000000000000, 1.000000000000000000, -0.000000000000000000 ) ) ;
#6207 = CARTESIAN_POINT ( 'NONE',  ( -114.2704648735229114, -294.0523547857347353, -270.3284710469133074 ) ) ;
#6208 = CARTESIAN_POINT ( 'NONE',  ( 20.69156538813412638, -275.4315121769824373, -320.7427095709945206 ) ) ;
#6209 = CARTESIAN_POINT ( 'NONE',  ( 33.64826364582375362, -293.1603887243161921, -253.2952121250226583 ) ) ;
#6210 = CARTESIAN_POINT ( 'NONE',  ( 27.05541097175026977, -282.5869969911775570, -234.5320818124958748 ) ) ;
#6211 = CARTESIAN_POINT ( 'NONE',  ( 23.70272951159275721, -276.5814809697065471, -228.8653593763626475 ) ) ;
#6212 = CARTESIAN_POINT ( 'NONE',  ( -44.34697730798828985, -284.5642481091381910, -346.5030432885454843 ) ) ;
#6213 = CARTESIAN_POINT ( 'NONE',  ( 34.15062801828890571, -280.1291092432218193, -253.7485467657982667 ) ) ;
#6214 = CARTESIAN_POINT ( 'NONE',  ( -97.68747563109087650, -279.9444796993178102, -314.9178802858327231 ) ) ;
#6215 = CARTESIAN_POINT ( 'NONE',  ( -29.05963080537725673, -298.1531627655757006, -193.3611175197906675 ) ) ;
#6216 = CARTESIAN_POINT ( 'NONE',  ( -1.469611089725223030, -276.4231416782081965, -338.4947604255356737 ) ) ;
#6217 = CARTESIAN_POINT ( 'NONE',  ( 34.84841348972083352, -295.7073786055452729, -288.5243141987052695 ) ) ;
#6218 = DIRECTION ( 'NONE',  ( 1.000000000000000000, 0.000000000000000000, 0.000000000000000000 ) ) ;
#6219 = FACE_OUTER_BOUND ( 'NONE', #40685, .T. ) ;
#6220 = CARTESIAN_POINT ( 'NONE',  ( -70.29244374219243241, -293.6212690641950758, -338.5996887388874939 ) ) ;
#6221 = CARTESIAN_POINT ( 'NONE',  ( 32.12227694818199097, -274.7576483826667300, -247.5544670511909828 ) ) ;
#6222 = CARTESIAN_POINT ( 'NONE',  ( 1.433940854225105976, -296.0639419691735270, -336.0814148394127301 ) ) ;
#6223 = CARTESIAN_POINT ( 'NONE',  ( 38.82956646151796321, -294.6490386022434222, -261.7552039642083628 ) ) ;
#6224 = CARTESIAN_POINT ( 'NONE',  ( 28.65913949725213783, -290.0225726966471598, -305.7406909415886958 ) ) ;
#6225 = CARTESIAN_POINT ( 'NONE',  ( -62.42781681643405989, -275.3789563287456303, -340.9195147435644913 ) ) ;
#6226 = CARTESIAN_POINT ( 'NONE',  ( -101.8181059383946661, -279.9708147026288998, -307.6681781409585597 ) ) ;
#6227 = CARTESIAN_POINT ( 'NONE',  ( -94.19777017212925330, -293.9621944795661079, -318.4298221417039940 ) ) ;
#6228 = CARTESIAN_POINT ( 'NONE',  ( 30.89847546074621931, -282.9819856178899045, -237.3226623909828277 ) ) ;
#6229 = CARTESIAN_POINT ( 'NONE',  ( -101.2541012418021467, -283.9629919314676272, -234.3484708155934300 ) ) ;
#6230 = CARTESIAN_POINT ( 'NONE',  ( 162.9801456899701293, 218.5183769072534119, -204.3598628306621094 ) ) ;
#6231 = ORIENTED_EDGE ( 'NONE', *, *, #93048, .F. ) ;
#6232 = CARTESIAN_POINT ( 'NONE',  ( -105.5831853876918700, -284.5657052422345146, -244.3767539095219092 ) ) ;
#6233 = EDGE_LOOP ( 'NONE', ( #29746, #4621, #92950, #76082, #91360 ) ) ;
#6234 = CARTESIAN_POINT ( 'NONE',  ( 39.22152015582132378, -282.6979308047666564, -275.6259240221770597 ) ) ;
#6235 = CARTESIAN_POINT ( 'NONE',  ( -105.0737947278021949, -283.8127741602531273, -234.4652986057015482 ) ) ;
#6236 = CARTESIAN_POINT ( 'NONE',  ( -104.5932386789552595, -279.9742764360261162, -233.3469210455023415 ) ) ;
#6237 = EDGE_CURVE ( 'NONE', #42461, #78803, #9730, .T. ) ;
#6238 = CARTESIAN_POINT ( 'NONE',  ( -111.8035546382335355, -279.8617966131459980, -287.0386471357826963 ) ) ;
#6239 = CARTESIAN_POINT ( 'NONE',  ( -102.0172624299486870, -298.6233781216987495, -301.5434626090942061 ) ) ;
#6240 = CARTESIAN_POINT ( 'NONE',  ( 6.552877139890185276, -58.82689968973230066, -354.7915936803940440 ) ) ;
#6241 = CARTESIAN_POINT ( 'NONE',  ( -43.66173072863657723, -275.9724079497053708, -195.7431512892062244 ) ) ;
#6242 = CARTESIAN_POINT ( 'NONE',  ( -40.04897441879919739, -139.4172891678365147, -364.6093070308725146 ) ) ;
#6243 = CARTESIAN_POINT ( 'NONE',  ( -86.54999248270378587, -277.3845387750056943, -214.2327760912575059 ) ) ;
#6244 = CARTESIAN_POINT ( 'NONE',  ( -47.62869337901483391, -293.6833694503192760, -195.0209006136624055 ) ) ;
#6245 = CARTESIAN_POINT ( 'NONE',  ( 20.26834423938420215, -292.2671166490576411, -225.3411227970795494 ) ) ;
#6246 = CARTESIAN_POINT ( 'NONE',  ( -107.6776610608314968, -289.6600801961170646, -301.6751773711759483 ) ) ;
#6247 = DIRECTION ( 'NONE',  ( -0.000000000000000000, -0.000000000000000000, -1.000000000000000000 ) ) ;
#6249 = CARTESIAN_POINT ( 'NONE',  ( -88.23158215116959013, -283.7248238893824919, -216.9133834972275281 ) ) ;
#6248 = CARTESIAN_POINT ( 'NONE',  ( 31.68984879413996936, -292.5513641340801883, -303.2449169963102804 ) ) ;
#6250 = CARTESIAN_POINT ( 'NONE',  ( -25.23052456769790197, -294.0684639767140425, -197.0681748386716663 ) ) ;
#6251 = CARTESIAN_POINT ( 'NONE',  ( 17.41867432603079280, -285.3323989892099348, -221.0268684639362959 ) ) ;
#6252 = CARTESIAN_POINT ( 'NONE',  ( -48.38637779903434222, -284.5108580119427302, -343.0196245194444487 ) ) ;
#6253 = ORIENTED_EDGE ( 'NONE', *, *, #81207, .T. ) ;
#6254 = CARTESIAN_POINT ( 'NONE',  ( -104.4102421220612626, -291.9790085570930387, -233.0163608248011542 ) ) ;
#6255 = CARTESIAN_POINT ( 'NONE',  ( 21.06287138854959551, -282.6605938335546284, -314.2782001541225441 ) ) ;
#6256 = CARTESIAN_POINT ( 'NONE',  ( 21.96940025529735863, -293.0014218570613593, -318.8605875491716120 ) ) ;
#6257 = CARTESIAN_POINT ( 'NONE',  ( 7.847822175835530878, -289.2554568675022324, -332.5722591529842020 ) ) ;
#6258 = CARTESIAN_POINT ( 'NONE',  ( -41.75075935475646816, -289.5986145386717681, -347.1863540663700292 ) ) ;
#6259 = CARTESIAN_POINT ( 'NONE',  ( 34.75955622041164617, -287.8705284256029699, -281.8604621962559804 ) ) ;
#6260 = VERTEX_POINT ( 'NONE', #88559 ) ;
#6261 = CARTESIAN_POINT ( 'NONE',  ( -53.01028712946499155, -297.1112087489473197, -344.5417064347121254 ) ) ;
#6262 = CARTESIAN_POINT ( 'NONE',  ( -103.4154014400012613, -295.7432781014155694, -231.6877970420247266 ) ) ;
#6263 = EDGE_CURVE ( 'NONE', #88883, #86547, #65618, .T. ) ;
#6264 = CARTESIAN_POINT ( 'NONE',  ( -97.84996783214617722, -277.0387620476395796, -311.6183353842870360 ) ) ;
#6265 = CARTESIAN_POINT ( 'NONE',  ( -83.53813120887681976, -272.9455414199836696, -208.7687025647727808 ) ) ;
#6266 = CARTESIAN_POINT ( 'NONE',  ( -92.72440893625083902, -294.3446140339749491, -318.9765817632398921 ) ) ;
#6267 = CARTESIAN_POINT ( 'NONE',  ( 36.59802255558142292, -277.2563129351966040, -266.0580193050591333 ) ) ;
#6268 = CARTESIAN_POINT ( 'NONE',  ( -68.78455360860226619, -271.7739958817561501, -203.0997926502641349 ) ) ;
#6269 = CARTESIAN_POINT ( 'NONE',  ( -82.59261759771673894, -296.8910101619217130, -328.2141840206216443 ) ) ;
#6270 = CARTESIAN_POINT ( 'NONE',  ( -58.48430324165660465, -296.4117015425314321, -340.5552516868115731 ) ) ;
#6271 = DIRECTION ( 'NONE',  ( -1.000000000000000000, 0.000000000000000000, 0.000000000000000000 ) ) ;
#6272 = CARTESIAN_POINT ( 'NONE',  ( -41.87735862997656255, -296.7083938070172735, -346.4778624229456341 ) ) ;
#6273 = CARTESIAN_POINT ( 'NONE',  ( -110.1981243275524776, -294.3143545430784229, -288.9055788577369412 ) ) ;
#6274 = CARTESIAN_POINT ( 'NONE',  ( -34.77200720577003068, -298.7349428432619902, -193.4627744701153063 ) ) ;
#6275 = CARTESIAN_POINT ( 'NONE',  ( -110.7116589345665574, -289.0444136629508307, -276.6624422077042027 ) ) ;
#6276 = CARTESIAN_POINT ( 'NONE',  ( -90.68200146038972775, -275.2960776682443793, -217.6371869676937365 ) ) ;
#6277 = CARTESIAN_POINT ( 'NONE',  ( -96.89243378546807151, -273.6992627285809476, -221.6246768237465972 ) ) ;
#6278 = CARTESIAN_POINT ( 'NONE',  ( -109.7577688912325442, -297.0141879662068618, -260.5981190934437564 ) ) ;
#6279 = CARTESIAN_POINT ( 'NONE',  ( -56.17057519999156767, -281.7908150504746914, -197.3423624808561954 ) ) ;
#6280 = CARTESIAN_POINT ( 'NONE',  ( -1.352514652375625293, -279.2041695886023831, -202.8475874680449920 ) ) ;
#6281 = ORIENTED_EDGE ( 'NONE', *, *, #9083, .F. ) ;
#6282 = CARTESIAN_POINT ( 'NONE',  ( -13.46147542462112234, -282.0985928901151851, -343.4572714688465567 ) ) ;
#6283 = CARTESIAN_POINT ( 'NONE',  ( 32.92326280345081102, -275.3000388853212712, -301.6044816060531844 ) ) ;
#6284 = CARTESIAN_POINT ( 'NONE',  ( 33.83292856169706653, -280.3001911706344913, -297.5753173070963271 ) ) ;
#6285 = CARTESIAN_POINT ( 'NONE',  ( -4.436608332239877051, -278.4845707366590091, -202.7652633982403358 ) ) ;
#6286 = CARTESIAN_POINT ( 'NONE',  ( -16.45619101152840713, -272.9019854118938042, -199.7447425639570611 ) ) ;
#6287 = CARTESIAN_POINT ( 'NONE',  ( 15.88758394768271742, -276.8059586878206915, -217.4524412971409504 ) ) ;
#6288 = CARTESIAN_POINT ( 'NONE',  ( 185.0172044724083946, 250.0000000000000568, 22.46007009812148425 ) ) ;
#6289 = CARTESIAN_POINT ( 'NONE',  ( 154.5625123364532101, 250.0000000000000568, 13.15740740740740655 ) ) ;
#6290 = CARTESIAN_POINT ( 'NONE',  ( -101.4492966493872643, -295.3338736476267741, -229.5666320672262088 ) ) ;
#6291 = CARTESIAN_POINT ( 'NONE',  ( -28.02685870437271731, -290.1898058533752192, -195.5313156700128161 ) ) ;
#6292 = AXIS2_PLACEMENT_3D ( 'NONE', #11680, #40530, #67591 ) ;
#6293 = CARTESIAN_POINT ( 'NONE',  ( -39.21169192941987092, -292.0293247714836866, -193.3707930653487779 ) ) ;
#6294 = CARTESIAN_POINT ( 'NONE',  ( 4.863448004814641124, -278.4835506810384800, -332.5604258201134371 ) ) ;
#6295 = CARTESIAN_POINT ( 'NONE',  ( 12.90482552054991494, -272.7529408077393214, -214.6109427262394433 ) ) ;
#6296 = CARTESIAN_POINT ( 'NONE',  ( 193.4805245855986584, 250.1588552167598039, 16.89623126087845861 ) ) ;
#6297 = CARTESIAN_POINT ( 'NONE',  ( -41.46562291945573975, -285.0237180993015045, -345.8598487995611208 ) ) ;
#6298 = LINE ( 'NONE', #48902, #80414 ) ;
#6299 = CIRCLE ( 'NONE', #4790, 7.500000000000012434 ) ;
#6300 = CARTESIAN_POINT ( 'NONE',  ( -30.47579335792610067, -284.1386902370635994, -195.6246995904763537 ) ) ;
#6301 = DIRECTION ( 'NONE',  ( 0.000000000000000000, 0.000000000000000000, 1.000000000000000000 ) ) ;
#6302 = CARTESIAN_POINT ( 'NONE',  ( 24.75504968184727517, -292.8858231087979789, -309.5861391591930101 ) ) ;
#6303 = CARTESIAN_POINT ( 'NONE',  ( 7.694784159547886304, -284.8135216979944744, -211.2827605389728660 ) ) ;
#6304 = DIRECTION ( 'NONE',  ( 1.000000000000000000, 0.000000000000000000, -0.000000000000000000 ) ) ;
#6305 = CARTESIAN_POINT ( 'NONE',  ( -81.34832271378733992, -293.6504158052019307, -331.0934636854557311 ) ) ;
#6306 = CARTESIAN_POINT ( 'NONE',  ( -113.6620627366040566, -283.0011575231761753, -272.8075153160856416 ) ) ;
#6307 = CARTESIAN_POINT ( 'NONE',  ( -94.57370232682005451, -280.8046222277030779, -223.7677886117756998 ) ) ;
#6308 = CARTESIAN_POINT ( 'NONE',  ( -68.35414295259512585, -286.8588275941886536, -200.3022776908047149 ) ) ;
#6309 = CARTESIAN_POINT ( 'NONE',  ( 18.43182106296206868, -279.0797130265393093, -218.7540608304223611 ) ) ;
#6310 = CARTESIAN_POINT ( 'NONE',  ( 23.53406431666785181, -286.9920877096481036, -229.9813714228226615 ) ) ;
#6311 = CARTESIAN_POINT ( 'NONE',  ( -64.53412166755546764, -278.8393573761998709, -338.7961243743629893 ) ) ;
#6312 = CARTESIAN_POINT ( 'NONE',  ( -105.6687549706312268, -279.7051851485769021, -244.0654836626166002 ) ) ;
#6313 = CARTESIAN_POINT ( 'NONE',  ( -92.72830435243361080, -287.2435288401311482, -219.1893038560930336 ) ) ;
#6314 = EDGE_LOOP ( 'NONE', ( #19635, #51769, #6625, #41760 ) ) ;
#6315 = CARTESIAN_POINT ( 'NONE',  ( -100.7494579649421809, -296.9624811853774986, -226.6520661668976970 ) ) ;
#6316 = CARTESIAN_POINT ( 'NONE',  ( -61.77001590052017832, -291.3510959274530592, -340.8955364608238483 ) ) ;
#6317 = LINE ( 'NONE', #22371, #30712 ) ;
#6318 = CARTESIAN_POINT ( 'NONE',  ( -99.90806341382572953, -281.6948066931272479, -220.5068182859052968 ) ) ;
#6319 = EDGE_LOOP ( 'NONE', ( #54530, #85626, #35666, #19153 ) ) ;
#6320 = CARTESIAN_POINT ( 'NONE',  ( 16.78750067991459005, -272.8198321972170106, -218.1321975868983714 ) ) ;
#6321 = CARTESIAN_POINT ( 'NONE',  ( 28.86934481696277999, -292.4482019360023628, -308.1842068824824423 ) ) ;
#6322 = CARTESIAN_POINT ( 'NONE',  ( -68.06769175122421700, -297.1451674423810232, -204.0609288307133227 ) ) ;
#6323 = CARTESIAN_POINT ( 'NONE',  ( 36.14489191360531350, -289.1527651609409872, -276.5201938796278114 ) ) ;
#6324 = CARTESIAN_POINT ( 'NONE',  ( -3.909623003421586862, -282.2594526982080083, -204.3146934355341386 ) ) ;
#6325 = CARTESIAN_POINT ( 'NONE',  ( -26.21231425154518391, -290.3383924064307848, -345.9570375926600718 ) ) ;
#6326 = CARTESIAN_POINT ( 'NONE',  ( -59.86600736562991187, -290.6532265288823851, -343.4771480662135446 ) ) ;
#6327 = CARTESIAN_POINT ( 'NONE',  ( -110.9372650422978239, -286.3668230351922830, -284.8073450568668363 ) ) ;
#6328 = CARTESIAN_POINT ( 'NONE',  ( -112.4022064887643069, -278.9336063995078803, -253.1878716552984940 ) ) ;
#6329 = ORIENTED_EDGE ( 'NONE', *, *, #19750, .F. ) ;
#6330 = CARTESIAN_POINT ( 'NONE',  ( -14.24588526452056314, -292.8347719327491632, -342.3048288401560058 ) ) ;
#6331 = CARTESIAN_POINT ( 'NONE',  ( -1.133560081756077365, -280.3524779540862824, -202.4054662756805669 ) ) ;
#6332 = CARTESIAN_POINT ( 'NONE',  ( -79.57696797711281533, -275.3356402232845994, -209.2491131851420221 ) ) ;
#6333 = CARTESIAN_POINT ( 'NONE',  ( 30.89617123739170168, -283.8376638359844719, -254.7536222014695397 ) ) ;
#6334 = CARTESIAN_POINT ( 'NONE',  ( 37.73002525306241495, -273.6419601848323850, -258.5208129215013741 ) ) ;
#6335 = CARTESIAN_POINT ( 'NONE',  ( 175.2296996224750103, 149.6461846693799487, 24.00000000000001066 ) ) ;
#6336 = CARTESIAN_POINT ( 'NONE',  ( 35.41424597613864478, -280.9647754071460213, -263.1515018985282950 ) ) ;
#6337 = CARTESIAN_POINT ( 'NONE',  ( -113.3252823047819078, -279.8845142694431161, -260.2356444982568178 ) ) ;
#6338 = CARTESIAN_POINT ( 'NONE',  ( -89.60455371904160415, -274.6112016343289497, -218.6906466064376673 ) ) ;
#6339 = CARTESIAN_POINT ( 'NONE',  ( -68.39455665404544504, -284.7128468580357321, -200.1432233888308474 ) ) ;
#6340 = CARTESIAN_POINT ( 'NONE',  ( -98.94179838893420253, -291.7502386729644286, -311.4134617236118743 ) ) ;
#6341 = CARTESIAN_POINT ( 'NONE',  ( -41.17314852266008529, -275.6049439593288639, -194.2057856069723698 ) ) ;
#6342 = CARTESIAN_POINT ( 'NONE',  ( -113.8491716523808606, -273.9029761287944211, -267.5287256790753077 ) ) ;
#6343 = CARTESIAN_POINT ( 'NONE',  ( 140.6539576904058606, 250.5000000000000568, 10.50000000000000000 ) ) ;
#6344 = CARTESIAN_POINT ( 'NONE',  ( -109.9600571257703621, -298.7855627628606499, -252.2364317070156972 ) ) ;
#6345 = CARTESIAN_POINT ( 'NONE',  ( -109.8763797858160132, -282.3150227144888049, -288.7662443556450285 ) ) ;
#6346 = CARTESIAN_POINT ( 'NONE',  ( -64.37740095122899220, -291.3756458193047365, -198.2298954611370618 ) ) ;
#6347 = CARTESIAN_POINT ( 'NONE',  ( 18.53315906116852574, -272.8799483769689687, -220.7885683032928625 ) ) ;
#6348 = CARTESIAN_POINT ( 'NONE',  ( 15.72728003122717944, -288.3886207526388148, -215.6790938879539681 ) ) ;
#6349 = CARTESIAN_POINT ( 'NONE',  ( -106.3280840637525841, -289.1435652046810674, -295.1624265110764895 ) ) ;
#6350 = ORIENTED_EDGE ( 'NONE', *, *, #86805, .T. ) ;
#6351 = CARTESIAN_POINT ( 'NONE',  ( -105.4704622536337268, -289.5770984406296407, -235.6456915098612228 ) ) ;
#6352 = CARTESIAN_POINT ( 'NONE',  ( -98.31485524360265060, -290.7770457921772049, -230.0901575075713481 ) ) ;
#6353 = VERTEX_POINT ( 'NONE', #87161 ) ;
#6354 = CARTESIAN_POINT ( 'NONE',  ( 37.71812022522413343, -288.4334691967059712, -254.5649487843805616 ) ) ;
#6355 = CARTESIAN_POINT ( 'NONE',  ( -45.90636683028166232, -277.4968833149300735, -342.9288870741538062 ) ) ;
#6356 = CARTESIAN_POINT ( 'NONE',  ( -36.29252458990619346, -293.9596585521684347, -347.0578816674728273 ) ) ;
#6357 = CARTESIAN_POINT ( 'NONE',  ( -37.30596059985554547, -283.7030888800183561, -347.2722252779598762 ) ) ;
#6358 = ADVANCED_FACE ( 'NONE', ( #87615 ), #52116, .F. ) ;
#6359 = CARTESIAN_POINT ( 'NONE',  ( -49.34561905264056492, -286.2365589357607405, -194.2702331627579895 ) ) ;
#6360 = CARTESIAN_POINT ( 'NONE',  ( -38.88127076147136307, -283.4052399362169012, -343.3785247585709044 ) ) ;
#6361 = CARTESIAN_POINT ( 'NONE',  ( 193.9776679813659825, 279.2223312090847571, -125.8845065936893519 ) ) ;
#6362 = TOROIDAL_SURFACE ( 'NONE', #4781, 24.50000000000001066, 0.5000000000000000000 ) ;
#6363 = CARTESIAN_POINT ( 'NONE',  ( 120.2832162277302928, 149.7717564229777452, -262.6457934689295257 ) ) ;
#6364 = CARTESIAN_POINT ( 'NONE',  ( -70.99751101762201699, -195.4794272351117854, -356.7654148836441550 ) ) ;
#6365 = CIRCLE ( 'NONE', #32022, 3.589950628481164419 ) ;
#6366 = CARTESIAN_POINT ( 'NONE',  ( -110.0450955006309073, -271.8569090480607429, -262.1868884703152389 ) ) ;
#6367 = CARTESIAN_POINT ( 'NONE',  ( -27.23401272400323947, -273.1038180833474485, -197.7010456017354727 ) ) ;
#6368 = CARTESIAN_POINT ( 'NONE',  ( -44.79590847252431018, -294.6516264851212554, -346.9909908257032498 ) ) ;
#6369 = CARTESIAN_POINT ( 'NONE',  ( 185.6221890035897957, 260.3163244210543894, -151.2547347512914087 ) ) ;
#6370 = CARTESIAN_POINT ( 'NONE',  ( -32.69570777663797401, -272.7943540709913464, -193.9823982106830726 ) ) ;
#6371 = CARTESIAN_POINT ( 'NONE',  ( -110.3527260578513420, -298.2374949657886418, -283.8573451078446510 ) ) ;
#6372 = CARTESIAN_POINT ( 'NONE',  ( -106.8687973730433214, -291.9392068475891051, -247.1187252012099975 ) ) ;
#6373 = VERTEX_POINT ( 'NONE', #81450 ) ;
#6374 = CARTESIAN_POINT ( 'NONE',  ( -101.4252126843175574, -296.9348787030529593, -312.7197856971699252 ) ) ;
#6375 = AXIS2_PLACEMENT_3D ( 'NONE', #50306, #36106, #87209 ) ;
#6376 = CARTESIAN_POINT ( 'NONE',  ( 20.40996426792068874, -288.6744489616175429, -315.1332895037521098 ) ) ;
#6377 = CARTESIAN_POINT ( 'NONE',  ( 26.38355116495089092, -294.9218142523610027, -313.2942190597748322 ) ) ;
#6378 = CARTESIAN_POINT ( 'NONE',  ( -68.19574210533816938, -295.9389810308233564, -340.8420018948996812 ) ) ;
#6379 = CARTESIAN_POINT ( 'NONE',  ( 20.99252186944289278, -293.1025300162912686, -226.4735508539140483 ) ) ;
#6380 = VERTEX_POINT ( 'NONE', #8098 ) ;
#6381 = CARTESIAN_POINT ( 'NONE',  ( 10.84814376549343073, -276.6323434020482068, -212.0947518564657628 ) ) ;
#6382 = EDGE_CURVE ( 'NONE', #74598, #307, #2242, .T. ) ;
#6383 = ORIENTED_EDGE ( 'NONE', *, *, #23960, .T. ) ;
#6384 = CARTESIAN_POINT ( 'NONE',  ( -100.1950907265145219, -278.6474338818921410, -225.9879482334482077 ) ) ;
#6385 = CARTESIAN_POINT ( 'NONE',  ( 35.25216680377810974, -276.3662346058220010, -260.6895652641109109 ) ) ;
#6386 = CARTESIAN_POINT ( 'NONE',  ( 8.876014119766217902, -276.4365044255048929, -210.0461372479127249 ) ) ;
#6387 = CARTESIAN_POINT ( 'NONE',  ( 15.77750456023545311, -274.3251199324144523, -323.8825923905679360 ) ) ;
#6388 = CARTESIAN_POINT ( 'NONE',  ( -109.3777171770042003, -297.3674176332897332, -257.9230748851302906 ) ) ;
#6389 = CARTESIAN_POINT ( 'NONE',  ( -107.4360443860469587, -294.8301362287202778, -292.9350903186063420 ) ) ;
#6390 = CARTESIAN_POINT ( 'NONE',  ( 184.7149167944524493, 8.542400036368780647, 13.00000000000000178 ) ) ;
#6391 = CARTESIAN_POINT ( 'NONE',  ( -111.3795896698812129, -278.7820147490118643, -291.2876039639390910 ) ) ;
#6392 = CARTESIAN_POINT ( 'NONE',  ( -32.41843851904511808, -277.1551741134557574, -343.2448779112194757 ) ) ;
#6393 = CARTESIAN_POINT ( 'NONE',  ( 7.270050870308891966, -285.3305706223928269, -208.1420976282661286 ) ) ;
#6394 = CARTESIAN_POINT ( 'NONE',  ( -90.36086187770479228, -299.3040049418938793, -217.0788797345456658 ) ) ;
#6395 = DIRECTION ( 'NONE',  ( -0.000000000000000000, -1.000000000000000000, -0.000000000000000000 ) ) ;
#6396 = CARTESIAN_POINT ( 'NONE',  ( 10.21247993001296095, -287.5739136560483757, -326.0266720910582308 ) ) ;
#6397 = CARTESIAN_POINT ( 'NONE',  ( -60.02314603951818128, -277.9941401691420424, -199.8547827550420664 ) ) ;
#6398 = CARTESIAN_POINT ( 'NONE',  ( -69.98546011304092929, -278.1882153518149039, -204.3944536736410953 ) ) ;
#6399 = CARTESIAN_POINT ( 'NONE',  ( -96.28254124675709136, -287.1892794189643041, -223.9621247545893823 ) ) ;
#6400 = CARTESIAN_POINT ( 'NONE',  ( -45.93946161100708991, -278.3685373940209615, -343.3037808704696658 ) ) ;
#6401 = DIRECTION ( 'NONE',  ( 0.000000000000000000, -0.2502735790305607444, 0.9681751575201843485 ) ) ;
#6402 = CARTESIAN_POINT ( 'NONE',  ( -99.64763134665689392, -276.2093950354652065, -313.8576115120782788 ) ) ;
#6403 = CARTESIAN_POINT ( 'NONE',  ( 0.6583803595884690774, -275.2248800559200390, -207.9120463234600322 ) ) ;
#6404 = CARTESIAN_POINT ( 'NONE',  ( 37.06030502173798880, -283.6893232537964309, -281.0555116736185823 ) ) ;
#6405 = CARTESIAN_POINT ( 'NONE',  ( 208.4306832106271088, -74.55766379199613425, 7.500000000000013323 ) ) ;
#6406 = CARTESIAN_POINT ( 'NONE',  ( -2.443645688494237245, -290.5142534318678145, -337.3793244423686701 ) ) ;
#6407 = CARTESIAN_POINT ( 'NONE',  ( -39.96265140076453548, -290.0190892058981831, -195.3943436893948729 ) ) ;
#6408 = CARTESIAN_POINT ( 'NONE',  ( 11.63197158325052172, -282.8906705383787994, 52.50000000000000711 ) ) ;
#6409 = CARTESIAN_POINT ( 'NONE',  ( -64.73716579658461967, -272.3716022403888815, -202.1512734879954110 ) ) ;
#6410 = CARTESIAN_POINT ( 'NONE',  ( 34.85450400292089057, -291.4669269607801994, -253.0274554578853099 ) ) ;
#6411 = CARTESIAN_POINT ( 'NONE',  ( 125.5584997210034572, 149.0310057319917405, -265.9501514013184078 ) ) ;
#6412 = DIRECTION ( 'NONE',  ( 0.000000000000000000, -1.000000000000000000, 0.000000000000000000 ) ) ;
#6413 = CARTESIAN_POINT ( 'NONE',  ( -34.71029200711424068, -287.4995322846278327, -346.6224020364168155 ) ) ;
#6414 = CARTESIAN_POINT ( 'NONE',  ( -71.76416114868720797, -285.1152112257479985, -335.6415483885547246 ) ) ;
#6415 = CARTESIAN_POINT ( 'NONE',  ( 30.52691738745054550, -285.3464304731541006, -236.1876667690419822 ) ) ;
#6416 = CARTESIAN_POINT ( 'NONE',  ( -95.57164275853696722, -285.3487231044622945, -315.3777781046228483 ) ) ;
#6417 = CARTESIAN_POINT ( 'NONE',  ( -78.45895826735632284, -284.4243568622601401, -330.8753544044073465 ) ) ;
#6418 = CARTESIAN_POINT ( 'NONE',  ( -25.30945435920438769, -294.1847050145924527, -195.9727327191242807 ) ) ;
#6419 = CARTESIAN_POINT ( 'NONE',  ( 38.26621618836384897, -273.6424438104039041, -271.1808900032881979 ) ) ;
#6420 = VECTOR ( 'NONE', #13501, 1000.000000000000000 ) ;
#6421 = CARTESIAN_POINT ( 'NONE',  ( -55.33279510528596035, -274.1600756565751453, -195.5141755402892443 ) ) ;
#6422 = AXIS2_PLACEMENT_3D ( 'NONE', #32622, #90344, #54377 ) ;
#6423 = CARTESIAN_POINT ( 'NONE',  ( -106.4249218411305549, -288.2325030944798527, -301.0974593380055921 ) ) ;
#6424 = CARTESIAN_POINT ( 'NONE',  ( -62.40599122933164011, -277.3692701495346000, -343.2238910260608122 ) ) ;
#6425 = CARTESIAN_POINT ( 'NONE',  ( 11.38383135535448254, -296.3525786689033339, -326.9090567730179373 ) ) ;
#6426 = CARTESIAN_POINT ( 'NONE',  ( 152.4536156746142410, 249.5000000000000568, 14.50000000000000000 ) ) ;
#6427 = CARTESIAN_POINT ( 'NONE',  ( -97.94846578770459189, -282.6611630872141063, -312.0198232531813005 ) ) ;
#6428 = CIRCLE ( 'NONE', #20006, 0.5000000000000004441 ) ;
#6429 = CARTESIAN_POINT ( 'NONE',  ( -96.11335332297561251, -277.1921505493837117, -223.7682705236798597 ) ) ;
#6430 = CARTESIAN_POINT ( 'NONE',  ( 219.8344101925596021, 35.72494958537217968, -7.000000000000000888 ) ) ;
#6431 = CARTESIAN_POINT ( 'NONE',  ( -71.07868559826272303, -272.0948510084914460, -201.9175385404270173 ) ) ;
#6432 = CARTESIAN_POINT ( 'NONE',  ( -108.8662258347256824, -277.7017663279243607, -285.4652528791221471 ) ) ;
#6433 = CIRCLE ( 'NONE', #56319, 1.000000000000000888 ) ;
#6434 = CARTESIAN_POINT ( 'NONE',  ( -4.005868003585892900, -296.1244270264804754, -336.0976216752981145 ) ) ;
#6435 = CARTESIAN_POINT ( 'NONE',  ( -1.268629040287204024, -279.4396341413352616, -202.6837506229804831 ) ) ;
#6436 = CARTESIAN_POINT ( 'NONE',  ( 35.76874303303664959, -294.4267036498310404, -265.2881402944820479 ) ) ;
#6437 = CARTESIAN_POINT ( 'NONE',  ( -19.38665920633425799, -296.1411593032297560, -344.7857749897622170 ) ) ;
#6438 = CARTESIAN_POINT ( 'NONE',  ( -100.7340143359106577, -272.7165427928381973, -234.0171802570863804 ) ) ;
#6439 = CARTESIAN_POINT ( 'NONE',  ( -96.51316919855044318, -291.9200719114670619, -316.4658879937258575 ) ) ;
#6440 = CARTESIAN_POINT ( 'NONE',  ( -57.75797785678248886, -285.9623842389826223, -196.0617384996037060 ) ) ;
#6441 = CARTESIAN_POINT ( 'NONE',  ( -73.33680312742842489, -271.7199786854134231, -203.6345357088191861 ) ) ;
#6442 = CARTESIAN_POINT ( 'NONE',  ( 39.64009771593815401, -287.3645348205320147, -268.6869599293588067 ) ) ;
#6443 = CARTESIAN_POINT ( 'NONE',  ( -108.0098986598259785, -280.8463087524490334, -246.1636644110311067 ) ) ;
#6444 = EDGE_CURVE ( 'NONE', #79467, #85305, #12868, .T. ) ;
#6445 = CARTESIAN_POINT ( 'NONE',  ( -71.27663862723254340, -284.6512386791011409, -205.4625170904564300 ) ) ;
#6446 = CARTESIAN_POINT ( 'NONE',  ( -23.70134904317697888, -286.8778148163198694, -344.1630038626366286 ) ) ;
#6447 = CARTESIAN_POINT ( 'NONE',  ( 117.8046289747227320, 148.0164379187816053, -257.9426961570557069 ) ) ;
#6448 = CARTESIAN_POINT ( 'NONE',  ( 16.94053583275968577, -286.3600077972337203, -221.4402168874307222 ) ) ;
#6449 = CARTESIAN_POINT ( 'NONE',  ( 29.56273004993958864, -282.9844407478719859, -308.1074613971295548 ) ) ;
#6450 = CARTESIAN_POINT ( 'NONE',  ( -112.3380454106139723, -289.4053982281808999, -286.7430717223928696 ) ) ;
#6451 = CARTESIAN_POINT ( 'NONE',  ( -53.60976510433307851, -281.4470555692896028, -195.8639101480814020 ) ) ;
#6452 = CARTESIAN_POINT ( 'NONE',  ( -94.60388262250833691, -280.5591372041472482, -219.6231565594009112 ) ) ;
#6453 = CARTESIAN_POINT ( 'NONE',  ( 20.17965966133159483, -282.0190265935351590, -315.3087894741240120 ) ) ;
#6454 = CARTESIAN_POINT ( 'NONE',  ( 37.58354874936826207, -277.4962935480174337, -265.9979052796920200 ) ) ;
#6455 = CARTESIAN_POINT ( 'NONE',  ( -44.79562445103660906, -295.1438942955880975, -347.0528897455528750 ) ) ;
#6456 = CARTESIAN_POINT ( 'NONE',  ( -10.14786510462004010, -286.7156592088262528, -339.9315967635010907 ) ) ;
#6457 = CARTESIAN_POINT ( 'NONE',  ( 3.812560456761368677, -296.1086018564839719, -334.5541116968458937 ) ) ;
#6458 = CARTESIAN_POINT ( 'NONE',  ( -101.7454054937444567, -294.9965075280497899, -305.3809524760209797 ) ) ;
#6459 = ORIENTED_EDGE ( 'NONE', *, *, #12627, .T. ) ;
#6460 = VERTEX_POINT ( 'NONE', #28955 ) ;
#6461 = CARTESIAN_POINT ( 'NONE',  ( 35.05627616331315011, -283.6970158355071590, -287.7315179273286390 ) ) ;
#6462 = CARTESIAN_POINT ( 'NONE',  ( -109.2959700491762760, -296.3828823077925563, -257.9244573800945091 ) ) ;
#6463 = CARTESIAN_POINT ( 'NONE',  ( 38.51284071453761015, -294.7736513591875109, -281.6563002893304315 ) ) ;
#6464 = CARTESIAN_POINT ( 'NONE',  ( -29.42538135728312909, -283.6007878141642209, -343.0837265835177732 ) ) ;
#6465 = CARTESIAN_POINT ( 'NONE',  ( -44.01033522066330050, -273.0286825488211093, -193.8334704915201883 ) ) ;
#6466 = CARTESIAN_POINT ( 'NONE',  ( 10.17148705544911103, -289.0681354844280122, -330.8921587932057946 ) ) ;
#6467 = CARTESIAN_POINT ( 'NONE',  ( -105.8981936611681789, -282.2718806229563029, -302.6149963885009697 ) ) ;
#6468 = CARTESIAN_POINT ( 'NONE',  ( -97.27093951715011144, -290.2373663458233750, -318.6957797608142187 ) ) ;
#6469 = CARTESIAN_POINT ( 'NONE',  ( 34.54325119434125213, -288.0546513150305259, -283.1923790351183925 ) ) ;
#6470 = CARTESIAN_POINT ( 'NONE',  ( 52.66432107828247666, -260.8771019122912094, -430.6442049081568939 ) ) ;
#6471 = FACE_OUTER_BOUND ( 'NONE', #34561, .T. ) ;
#6472 = CARTESIAN_POINT ( 'NONE',  ( -82.51230583331636126, -218.8770980360667693, -348.9302519833477731 ) ) ;
#6473 = CARTESIAN_POINT ( 'NONE',  ( 39.58706461736021254, -273.0523547857348490, -270.3937649182068981 ) ) ;
#6474 = CARTESIAN_POINT ( 'NONE',  ( -103.5115380187420584, -278.1715385815084005, -239.0306326137186375 ) ) ;
#6475 = VERTEX_POINT ( 'NONE', #15211 ) ;
#6476 = CARTESIAN_POINT ( 'NONE',  ( -35.64190526219495325, -278.9942678978713957, -197.0592586586642483 ) ) ;
#6477 = CARTESIAN_POINT ( 'NONE',  ( 28.48666950001588205, -274.6966934687411026, -230.3546945851999226 ) ) ;
#6478 = CARTESIAN_POINT ( 'NONE',  ( -64.98731406889790208, -279.4141527825871663, -339.9556852273502159 ) ) ;
#6479 = CARTESIAN_POINT ( 'NONE',  ( -29.06568833929538798, -125.6893641773768877, -361.8808603065265856 ) ) ;
#6480 = CARTESIAN_POINT ( 'NONE',  ( -112.6526487677783166, -277.2896839759220597, -257.4434050069697264 ) ) ;
#6481 = CARTESIAN_POINT ( 'NONE',  ( -83.83854698117650628, -281.7138610158831398, -328.8217258226717377 ) ) ;
#6482 = CARTESIAN_POINT ( 'NONE',  ( -98.29321305435765055, -298.9240519474489020, -224.9644325659491813 ) ) ;
#6483 = CARTESIAN_POINT ( 'NONE',  ( 30.64512757076958849, -294.4036246806608119, -297.2536289764103685 ) ) ;
#6484 = EDGE_LOOP ( 'NONE', ( #33767, #26856, #40529, #61563, #76682, #33936, #28025, #52477 ) ) ;
#6485 = CARTESIAN_POINT ( 'NONE',  ( -93.80805598178397986, -289.9001162951274750, -223.3011317145225121 ) ) ;
#6486 = CARTESIAN_POINT ( 'NONE',  ( 36.48565114859932379, -275.9313006778426711, -248.6615087708247529 ) ) ;
#6487 = CARTESIAN_POINT ( 'NONE',  ( -110.3417001280813849, -272.5880843968022873, -267.6372586758525927 ) ) ;
#6488 = VERTEX_POINT ( 'NONE', #51636 ) ;
#6489 = CARTESIAN_POINT ( 'NONE',  ( 221.8344101925596306, -43.55766379199612004, -22.50000000000000000 ) ) ;
#6490 = CIRCLE ( 'NONE', #36684, 1.000000000000000888 ) ;
#6491 = CARTESIAN_POINT ( 'NONE',  ( 208.6208076322478746, 32.98517505407394168, 10.00000000000000000 ) ) ;
#6492 = VECTOR ( 'NONE', #33731, 1000.000000000000000 ) ;
#6493 = CARTESIAN_POINT ( 'NONE',  ( 26.72232934394043014, -282.1466173397262764, -234.7236910181440237 ) ) ;
#6494 = CARTESIAN_POINT ( 'NONE',  ( 18.40135289542600106, -282.5994273224870312, -218.7211523205825188 ) ) ;
#6495 = CARTESIAN_POINT ( 'NONE',  ( -108.6571634405473645, -283.3911927967691327, -287.0746750277188539 ) ) ;
#6496 = CARTESIAN_POINT ( 'NONE',  ( 14.17553149012710634, -282.6450427156368619, -216.8400868703600395 ) ) ;
#6497 = CARTESIAN_POINT ( 'NONE',  ( 16.08735612131448889, -274.7568267279347083, -321.1158586555979468 ) ) ;
#6499 = CARTESIAN_POINT ( 'NONE',  ( 209.6851631783452490, 27.99050452776153008, 13.95111757441321920 ) ) ;
#6498 = AXIS2_PLACEMENT_3D ( 'NONE', #25153, #17593, #46443 ) ;
#6500 = DIRECTION ( 'NONE',  ( 0.000000000000000000, 0.000000000000000000, 1.000000000000000000 ) ) ;
#6501 = CIRCLE ( 'NONE', #18502, 7.500000000000012434 ) ;
#6502 = CARTESIAN_POINT ( 'NONE',  ( -89.09579538521494158, -278.5611536762490914, -327.1561216729629678 ) ) ;
#6503 = EDGE_CURVE ( 'NONE', #67510, #7995, #59704, .T. ) ;
#6504 = CARTESIAN_POINT ( 'NONE',  ( 209.7513585654923816, 282.2246705312486483, -40.00000000000000711 ) ) ;
#6505 = ORIENTED_EDGE ( 'NONE', *, *, #60912, .F. ) ;
#6506 = CARTESIAN_POINT ( 'NONE',  ( 183.0442525570908288, 275.0000000000000568, 20.22542485937379908 ) ) ;
#6507 = CARTESIAN_POINT ( 'NONE',  ( -110.7629702859770049, -286.7488097006516909, -253.3986919732841159 ) ) ;
#6508 = CARTESIAN_POINT ( 'NONE',  ( 35.80294670404060042, -292.7907103614479638, -273.5060859757203389 ) ) ;
#6509 = EDGE_CURVE ( 'NONE', #13368, #48695, #44542, .T. ) ;
#6510 = CARTESIAN_POINT ( 'NONE',  ( 19.54324741911989349, -287.6050977731702574, -322.1244776297479575 ) ) ;
#6511 = CARTESIAN_POINT ( 'NONE',  ( -33.15928537565051215, -284.3452565886557295, -196.4155367775724699 ) ) ;
#6513 = CARTESIAN_POINT ( 'NONE',  ( -97.39374860989762794, -288.1952892120093566, -313.6245608417328867 ) ) ;
#6512 = CARTESIAN_POINT ( 'NONE',  ( -75.00622501962587307, -284.1144807241320223, -207.1411964243589807 ) ) ;
#6514 = CARTESIAN_POINT ( 'NONE',  ( -33.45996125047639680, -284.2073162824495967, -343.6681147690134139 ) ) ;
#6515 = CARTESIAN_POINT ( 'NONE',  ( -35.54547121304181445, -272.0745038785823340, -195.3698374586679734 ) ) ;
#6516 = CARTESIAN_POINT ( 'NONE',  ( -110.3474330995260999, -282.6746769152262004, -292.2377169337230498 ) ) ;
#6517 = CARTESIAN_POINT ( 'NONE',  ( -73.61611860142298269, -297.5333320825926648, -336.0635182075294551 ) ) ;
#6518 = CARTESIAN_POINT ( 'NONE',  ( -40.70824095597872372, -284.0098745121070465, -195.2189231717056828 ) ) ;
#6519 = CARTESIAN_POINT ( 'NONE',  ( -105.4823552742332851, -279.1356499873536450, -297.1987699638935396 ) ) ;
#6520 = CARTESIAN_POINT ( 'NONE',  ( 0.5743636803178351347, -288.5564003807857034, -205.4431388171454387 ) ) ;
#6521 = CARTESIAN_POINT ( 'NONE',  ( 196.9274440531671360, 292.2264140707667366, -7.812896314794627983 ) ) ;
#6522 = CARTESIAN_POINT ( 'NONE',  ( 129.8975571001389540, -299.5541904835127980, -201.2022030660758389 ) ) ;
#6523 = CARTESIAN_POINT ( 'NONE',  ( 33.11769049971713486, -295.8246267347387857, -297.6519308754502049 ) ) ;
#6524 = AXIS2_PLACEMENT_3D ( 'NONE', #29864, #87591, #80499 ) ;
#6525 = CIRCLE ( 'NONE', #50302, 1.000000000000000888 ) ;
#6526 = CARTESIAN_POINT ( 'NONE',  ( -67.63316614681787087, -275.4494358090855144, -338.9718149474385882 ) ) ;
#6527 = CARTESIAN_POINT ( 'NONE',  ( -112.7116143465756437, -289.5611102020022827, -285.3789357411529295 ) ) ;
#6528 = CARTESIAN_POINT ( 'NONE',  ( -78.41168134439851656, -294.0145096028305716, -331.7392226573571747 ) ) ;
#6529 = CARTESIAN_POINT ( 'NONE',  ( -67.49339956153842479, -278.3329741898783141, -203.3241532024158573 ) ) ;
#6530 = CARTESIAN_POINT ( 'NONE',  ( -47.41733740621171478, -296.0624716098051863, -196.7607795853814423 ) ) ;
#6531 = CARTESIAN_POINT ( 'NONE',  ( -2.218387250261451449, -293.8424804235529564, -205.7899047976282816 ) ) ;
#6532 = CARTESIAN_POINT ( 'NONE',  ( -106.6379572354042153, -280.6233781216988064, -303.7686719486574134 ) ) ;
#6533 = CARTESIAN_POINT ( 'NONE',  ( -6.099435426505046109, -293.1288594594918209, -339.9788502848842313 ) ) ;
#6534 = CARTESIAN_POINT ( 'NONE',  ( 8.492553830895174016, -290.0124198531250954, -328.2028120882733333 ) ) ;
#6535 = CARTESIAN_POINT ( 'NONE',  ( 24.00972035802857718, -291.1888897783472885, -225.5283484969783956 ) ) ;
#6536 = CARTESIAN_POINT ( 'NONE',  ( -31.80908460157409223, -290.4063869104180071, -343.7931086499631874 ) ) ;
#6537 = DIRECTION ( 'NONE',  ( 0.000000000000000000, 0.000000000000000000, 1.000000000000000000 ) ) ;
#6538 = CARTESIAN_POINT ( 'NONE',  ( -92.52680752193022329, -290.6709314837173679, -318.4701931679086897 ) ) ;
#6539 = CARTESIAN_POINT ( 'NONE',  ( 188.7399167944524550, 8.542400036368780647, 10.00000000000000000 ) ) ;
#6540 = CARTESIAN_POINT ( 'NONE',  ( -110.3984837575261224, -291.4642496548331678, -293.5715511321573672 ) ) ;
#6542 = CARTESIAN_POINT ( 'NONE',  ( 34.32437576633277132, -293.7354040298964719, -284.2526105552130957 ) ) ;
#6541 = CARTESIAN_POINT ( 'NONE',  ( 36.25357655829716919, -279.7799331761949588, -286.6114207950956256 ) ) ;
#6543 = CARTESIAN_POINT ( 'NONE',  ( -48.11878132662029373, -279.9187897701352199, -194.0651950902481246 ) ) ;
#6544 = CARTESIAN_POINT ( 'NONE',  ( 11.47591344234680477, -282.0633261890745871, -329.9497106719672956 ) ) ;
#6545 = CARTESIAN_POINT ( 'NONE',  ( -4.911389980194055482, -284.4789127216827183, -202.7209562927560000 ) ) ;
#6546 = CARTESIAN_POINT ( 'NONE',  ( 20.29633185581394983, -280.3429185512247273, -317.1649348857197310 ) ) ;
#6547 = CARTESIAN_POINT ( 'NONE',  ( -84.24188727825426781, -283.4068543108936638, -211.8344309851138121 ) ) ;
#6548 = CARTESIAN_POINT ( 'NONE',  ( -68.37268570619971797, -278.1317639748304487, -200.6347005949525624 ) ) ;
#6549 = CARTESIAN_POINT ( 'NONE',  ( 37.42138855115708651, -286.2572660653249272, -253.2155686856430918 ) ) ;
#6550 = CARTESIAN_POINT ( 'NONE',  ( -34.04360771932221041, -274.8975283699658121, -197.2740171113412089 ) ) ;
#6551 = CARTESIAN_POINT ( 'NONE',  ( 196.0677363144156402, 41.33745432255098251, 14.18591286744891633 ) ) ;
#6552 = CARTESIAN_POINT ( 'NONE',  ( -86.47668379385717685, -292.9567183766341145, -215.2269578464480446 ) ) ;
#6553 = CARTESIAN_POINT ( 'NONE',  ( -5.377410422757828101, -275.8898087487230555, -200.9572961958038775 ) ) ;
#6554 = CARTESIAN_POINT ( 'NONE',  ( -107.1380903662694379, -277.9326703360477495, -291.9909291711151695 ) ) ;
#6555 = CARTESIAN_POINT ( 'NONE',  ( -97.46489713158233315, -291.3632090535338648, -222.2549729840611406 ) ) ;
#6556 = VECTOR ( 'NONE', #54357, 1000.000000000000000 ) ;
#6557 = CARTESIAN_POINT ( 'NONE',  ( 38.17975426672617800, -279.6627535129732109, -272.7744396278453678 ) ) ;
#6558 = CARTESIAN_POINT ( 'NONE',  ( -84.26466945018242427, -291.2603840285428873, -209.2428341877914022 ) ) ;
#6559 = CARTESIAN_POINT ( 'NONE',  ( -79.65691922584757378, -290.5235712626206919, -210.5258054354374906 ) ) ;
#6560 = CIRCLE ( 'NONE', #14137, 6.499999999999977796 ) ;
#6561 = CARTESIAN_POINT ( 'NONE',  ( 12.05883123497936893, -292.3655376327747035, -326.8621103334050986 ) ) ;
#6562 = ORIENTED_EDGE ( 'NONE', *, *, #85946, .T. ) ;
#6563 = CARTESIAN_POINT ( 'NONE',  ( 140.6539576904058606, 275.0000000000000568, -10.49999999999999822 ) ) ;
#6564 = AXIS2_PLACEMENT_3D ( 'NONE', #82409, #17556, #46408 ) ;
#6565 = CARTESIAN_POINT ( 'NONE',  ( 24.90358327567604846, -292.5317611427775546, -232.0091707885733854 ) ) ;
#6566 = DIRECTION ( 'NONE',  ( -0.000000000000000000, 1.000000000000000000, -0.000000000000000000 ) ) ;
#6567 = CARTESIAN_POINT ( 'NONE',  ( -67.74223827176246004, -274.9809262143061233, -333.4151289067050357 ) ) ;
#6568 = CARTESIAN_POINT ( 'NONE',  ( -114.1025628679917645, -295.6205387770629045, -269.5928968527447296 ) ) ;
#6569 = EDGE_CURVE ( 'NONE', #13227, #55526, #85443, .T. ) ;
#6570 = CARTESIAN_POINT ( 'NONE',  ( -113.4117338338399605, -285.7645654467869463, -278.5249555656179155 ) ) ;
#6571 = CARTESIAN_POINT ( 'NONE',  ( -37.27874143033333354, -285.8862449826743273, -197.3487066273611958 ) ) ;
#6572 = AXIS2_PLACEMENT_3D ( 'NONE', #54618, #75936, #26693 ) ;
#6573 = CARTESIAN_POINT ( 'NONE',  ( 34.26479472108430002, -277.3004929461735060, -287.8274800447115354 ) ) ;
#6574 = CARTESIAN_POINT ( 'NONE',  ( -35.63778818994382647, -293.0508104871523187, -344.9992501454398166 ) ) ;
#6575 = CARTESIAN_POINT ( 'NONE',  ( -66.43104666926203095, -297.1985343367881001, -338.4183287162916827 ) ) ;
#6576 = CARTESIAN_POINT ( 'NONE',  ( 35.74802914649394125, -274.4351054550053846, -277.0709599166363546 ) ) ;
#6577 = ORIENTED_EDGE ( 'NONE', *, *, #73794, .F. ) ;
#6578 = DIRECTION ( 'NONE',  ( 0.000000000000000000, 0.000000000000000000, -1.000000000000000000 ) ) ;
#6579 = CARTESIAN_POINT ( 'NONE',  ( -109.4192376298144609, -295.8751840822670260, -297.5406420609234033 ) ) ;
#6580 = CARTESIAN_POINT ( 'NONE',  ( -5.147955647059831996, -290.5451969658647045, -337.4794986122409455 ) ) ;
#6581 = CARTESIAN_POINT ( 'NONE',  ( -70.45673859265708927, -295.6154843447001213, -203.0537799537354147 ) ) ;
#6582 = CARTESIAN_POINT ( 'NONE',  ( 8.049715046464978485, -289.0638573547333863, -327.6630559626719332 ) ) ;
#6583 = ORIENTED_EDGE ( 'NONE', *, *, #91723, .T. ) ;
#6584 = CARTESIAN_POINT ( 'NONE',  ( -17.04263941731080934, -279.3667908485597877, -196.3289064352503885 ) ) ;
#6585 = CARTESIAN_POINT ( 'NONE',  ( -4.538476584350812360, -295.2826329961549732, -339.9259923751421297 ) ) ;
#6586 = CARTESIAN_POINT ( 'NONE',  ( -88.67231831860898694, -287.9030610804585990, -326.0878899559325532 ) ) ;
#6587 = CARTESIAN_POINT ( 'NONE',  ( -65.59178689926186223, -295.7448866879855700, -341.9831347632746770 ) ) ;
#6588 = CARTESIAN_POINT ( 'NONE',  ( 17.99122801174845421, -294.5640015850973441, -318.0284220055924607 ) ) ;
#6589 = CARTESIAN_POINT ( 'NONE',  ( 198.7877904355241014, 66.56388957926334626, -9.416941149845250436 ) ) ;
#6590 = CIRCLE ( 'NONE', #11085, 7.500000000000012434 ) ;
#6591 = FACE_OUTER_BOUND ( 'NONE', #50586, .T. ) ;
#6592 = DIRECTION ( 'NONE',  ( 0.000000000000000000, 0.000000000000000000, -1.000000000000000000 ) ) ;
#6593 = CARTESIAN_POINT ( 'NONE',  ( -38.88655491756519211, -290.5913193115104605, -346.6521474590123830 ) ) ;
#6594 = CARTESIAN_POINT ( 'NONE',  ( -111.2586520408596868, -294.4809262143061801, -234.7283546768995564 ) ) ;
#6595 = CARTESIAN_POINT ( 'NONE',  ( -74.95083019618745368, -278.9133656202303087, -203.2875306161356832 ) ) ;
#6596 = CARTESIAN_POINT ( 'NONE',  ( -33.37417773616327565, -285.0022726105054858, -345.1020945705409986 ) ) ;
#6597 = CARTESIAN_POINT ( 'NONE',  ( -35.14683484195653307, -284.6539052169579804, -193.9688316563729984 ) ) ;
#6598 = CARTESIAN_POINT ( 'NONE',  ( -71.86183079828371945, -287.5919262509218584, -336.3275854164556904 ) ) ;
#6599 = CARTESIAN_POINT ( 'NONE',  ( 29.46527736692121380, -277.8832283038901210, -306.2089579011853857 ) ) ;
#6600 = AXIS2_PLACEMENT_3D ( 'NONE', #46808, #33548, #3272 ) ;
#6601 = ORIENTED_EDGE ( 'NONE', *, *, #65063, .F. ) ;
#6603 = CARTESIAN_POINT ( 'NONE',  ( -108.9854890862335424, -278.0929445793325385, -255.7703834221395880 ) ) ;
#6602 = CARTESIAN_POINT ( 'NONE',  ( -105.5142875194777332, -278.9024818493712132, -244.1140122844505811 ) ) ;
#6604 = CARTESIAN_POINT ( 'NONE',  ( -0.2072120995418920142, -275.6137855762760296, -203.2453493493229928 ) ) ;
#6605 = CARTESIAN_POINT ( 'NONE',  ( -108.1397975735866055, -277.7207934531446085, -241.1098254350427226 ) ) ;
#6606 = CARTESIAN_POINT ( 'NONE',  ( -107.6144582921256045, -259.8900720772599016, -316.0350854841208275 ) ) ;
#6607 = CARTESIAN_POINT ( 'NONE',  ( -105.4058824157608285, -273.9540124396383476, -234.7484878119597624 ) ) ;
#6608 = CARTESIAN_POINT ( 'NONE',  ( -84.86424733187504899, -298.8364794797370223, -210.5262301783543535 ) ) ;
#6609 = CARTESIAN_POINT ( 'NONE',  ( -85.33152481854864391, -281.9090924074130839, -210.2361428286349110 ) ) ;
#6610 = DIRECTION ( 'NONE',  ( 0.000000000000000000, 0.000000000000000000, 1.000000000000000000 ) ) ;
#6611 = CARTESIAN_POINT ( 'NONE',  ( -30.51613812302811723, -287.2200231353003232, -197.3194357045243805 ) ) ;
#6612 = CARTESIAN_POINT ( 'NONE',  ( -3.955078835683296656, -288.2465432557098097, -202.0876632292296051 ) ) ;
#6613 = CARTESIAN_POINT ( 'NONE',  ( 31.49259726753807342, -287.2279810332042302, -294.9727447088218923 ) ) ;
#6614 = CARTESIAN_POINT ( 'NONE',  ( -108.9688924601785658, -284.4178006332363680, -242.1258312062719824 ) ) ;
#6615 = CARTESIAN_POINT ( 'NONE',  ( 32.74269016030901724, -279.6465110759282311, -247.0780914409574507 ) ) ;
#6616 = CARTESIAN_POINT ( 'NONE',  ( -65.58474050235567177, -287.5394273996338370, -201.6536694010913777 ) ) ;
#6617 = CARTESIAN_POINT ( 'NONE',  ( 22.68942733861521432, -279.4405852020823318, -227.6180309575036631 ) ) ;
#6618 = CARTESIAN_POINT ( 'NONE',  ( -36.44345521342935967, -278.3558744321240965, -343.8613323765147811 ) ) ;
#6619 = CARTESIAN_POINT ( 'NONE',  ( 33.89235839777776249, -275.8298007282705839, -254.0664438122052786 ) ) ;
#6620 = CARTESIAN_POINT ( 'NONE',  ( -20.59821986002108574, -287.6368400893687181, -345.1661836310428271 ) ) ;
#6621 = CARTESIAN_POINT ( 'NONE',  ( 24.98231923505507979, -282.9523804796303352, -315.3264808893650297 ) ) ;
#6622 = CARTESIAN_POINT ( 'NONE',  ( -100.9491547924593959, -285.6168232319852791, -226.9816782593109963 ) ) ;
#6623 = CARTESIAN_POINT ( 'NONE',  ( 13.33357447749409985, -280.9515796475541833, -217.7453004786957536 ) ) ;
#6624 = ORIENTED_EDGE ( 'NONE', *, *, #34302, .F. ) ;
#6625 = ORIENTED_EDGE ( 'NONE', *, *, #39536, .F. ) ;
#6626 = PLANE ( 'NONE',  #89647 ) ;
#6627 = CARTESIAN_POINT ( 'NONE',  ( 19.65950247315573307, -290.0989604033294995, -320.2922761551112103 ) ) ;
#6628 = AXIS2_PLACEMENT_3D ( 'NONE', #41896, #20617, #63257 ) ;
#6629 = CARTESIAN_POINT ( 'NONE',  ( -112.4376616308706929, -289.4219280805659196, -255.6678028095986690 ) ) ;
#6630 = CARTESIAN_POINT ( 'NONE',  ( -78.97902877870349414, -272.5344233526247422, -210.0521894456521466 ) ) ;
#6631 = CARTESIAN_POINT ( 'NONE',  ( 11.12762384311921515, -293.7499935276551355, -330.1292918364587194 ) ) ;
#6632 = CARTESIAN_POINT ( 'NONE',  ( -110.6607769990965977, -289.1289535525201586, -262.9435227937988770 ) ) ;
#6633 = CARTESIAN_POINT ( 'NONE',  ( 33.60681202856758887, -291.5147991502217906, -249.1063127810191702 ) ) ;
#6634 = CARTESIAN_POINT ( 'NONE',  ( -5.606931943497451165, -289.8302344199476011, -336.5429507958160116 ) ) ;
#6635 = CARTESIAN_POINT ( 'NONE',  ( -54.49178911615187815, -288.3376638359845856, -195.3683826091709363 ) ) ;
#6636 = TOROIDAL_SURFACE ( 'NONE', #30813, 24.00000000000000355, 1.000000000000000000 ) ;
#6637 = CARTESIAN_POINT ( 'NONE',  ( -0.2471318021208591398, -290.5593828569722064, -335.6041203877783232 ) ) ;
#6638 = CARTESIAN_POINT ( 'NONE',  ( -68.83131466645507146, -289.6390286043416609, -202.0944082800476167 ) ) ;
#6639 = CARTESIAN_POINT ( 'NONE',  ( -95.33902107660433956, -293.2081158090055055, -222.7880995410212108 ) ) ;
#6640 = CARTESIAN_POINT ( 'NONE',  ( -87.07987596438424305, -284.7063310625655390, -324.1847639097438787 ) ) ;
#6641 = CARTESIAN_POINT ( 'NONE',  ( 19.89742046132858633, -294.8791675456744201, -221.6207126353536125 ) ) ;
#6642 = CARTESIAN_POINT ( 'NONE',  ( 197.9445473535714939, 71.72765703697457695, -10.67027600767165652 ) ) ;
#6643 = CARTESIAN_POINT ( 'NONE',  ( 154.5625123364532101, 276.0000000000000568, -13.15740740740742254 ) ) ;
#6644 = CIRCLE ( 'NONE', #42844, 4.025000000000000355 ) ;
#6645 = CARTESIAN_POINT ( 'NONE',  ( -91.99693719222734956, -275.2566046300505036, -218.4653892081879007 ) ) ;
#6646 = CARTESIAN_POINT ( 'NONE',  ( -1.181068500683291056, -281.7562840504023143, -333.9615145806608894 ) ) ;
#6647 = CARTESIAN_POINT ( 'NONE',  ( -34.80369346456757285, -281.0201362912669083, -345.3309444503383361 ) ) ;
#6648 = CARTESIAN_POINT ( 'NONE',  ( -112.7282654981038377, -295.9364926349201710, -255.4266029986495425 ) ) ;
#6649 = CARTESIAN_POINT ( 'NONE',  ( 30.01745664834820104, -273.3826950467091592, -239.5659295888317786 ) ) ;
#6650 = CARTESIAN_POINT ( 'NONE',  ( -110.2936654037478093, -276.8244089385058260, -255.4875862541763922 ) ) ;
#6651 = CARTESIAN_POINT ( 'NONE',  ( -109.6241325977257901, -297.6923411541915812, -283.7158304978031538 ) ) ;
#6652 = CIRCLE ( 'NONE', #82249, 0.9999999999999756861 ) ;
#6653 = VECTOR ( 'NONE', #77496, 1000.000000000000000 ) ;
#6654 = CARTESIAN_POINT ( 'NONE',  ( -103.2881996614228086, -297.5369145434791562, -303.1325174747352094 ) ) ;
#6655 = LINE ( 'NONE', #36448, #79231 ) ;
#6656 = CARTESIAN_POINT ( 'NONE',  ( -92.87363088870235117, -298.0317174063097241, -222.7098557073385621 ) ) ;
#6657 = CARTESIAN_POINT ( 'NONE',  ( 208.4306832106270804, -125.2391364535880882, -7.500000000000012434 ) ) ;
#6659 = CARTESIAN_POINT ( 'NONE',  ( -93.77702672893708780, -273.0415946126373683, -224.0376431982256804 ) ) ;
#6658 = CARTESIAN_POINT ( 'NONE',  ( -13.20614202235572776, -284.3842513691508884, -198.9756738344607356 ) ) ;
#6660 = AXIS2_PLACEMENT_3D ( 'NONE', #61021, #83697, #41053 ) ;
#6661 = CARTESIAN_POINT ( 'NONE',  ( -71.06623095477689844, -285.6193044007573008, -201.1393293570176297 ) ) ;
#6662 = CARTESIAN_POINT ( 'NONE',  ( 30.34207597361525544, -287.6946251363839906, -307.1420669386396298 ) ) ;
#6663 = CARTESIAN_POINT ( 'NONE',  ( -112.5896905899195843, -298.4694656633264458, -275.2581577672503954 ) ) ;
#6664 = CARTESIAN_POINT ( 'NONE',  ( 29.12632607952265573, -291.0959216673146557, -235.9804560406519158 ) ) ;
#6665 = CARTESIAN_POINT ( 'NONE',  ( -17.02482706760614661, -279.5051879767985383, -196.2572483867477331 ) ) ;
#6666 = CARTESIAN_POINT ( 'NONE',  ( -69.91165696735023971, -286.9809262143061801, -337.9199732462171255 ) ) ;
#6667 = CARTESIAN_POINT ( 'NONE',  ( 222.4201966301864957, -0.4142135623730890392, -22.50000000000000000 ) ) ;
#6668 = AXIS2_PLACEMENT_3D ( 'NONE', #19350, #48212, #77115 ) ;
#6669 = CARTESIAN_POINT ( 'NONE',  ( -10.59103117119208370, -285.2039481218492938, -201.9989092317847224 ) ) ;
#6670 = CARTESIAN_POINT ( 'NONE',  ( 198.7989590516236547, 65.26577858576978031, -10.60668493626651454 ) ) ;
#6671 = CARTESIAN_POINT ( 'NONE',  ( -96.54461299498061067, -287.9203992070815730, -316.4255057361012291 ) ) ;
#6672 = CARTESIAN_POINT ( 'NONE',  ( -93.45417681046285452, -274.7455148904640509, -222.5703260860421722 ) ) ;
#6673 = CARTESIAN_POINT ( 'NONE',  ( -77.20076106695164242, -280.9545562995942873, -205.1088946031197224 ) ) ;
#6675 = CARTESIAN_POINT ( 'NONE',  ( 33.76038918893654994, -281.3339898320557495, -253.8234973932851801 ) ) ;
#6674 = CARTESIAN_POINT ( 'NONE',  ( -101.7236804649435840, -294.0498093946732752, -309.5193535032951218 ) ) ;
#6676 = CARTESIAN_POINT ( 'NONE',  ( -99.09371044264601380, -297.3308483736353196, -224.3424893930035466 ) ) ;
#6677 = CARTESIAN_POINT ( 'NONE',  ( -68.35680922567161133, -299.1573103713457726, -203.4984573578359175 ) ) ;
#6678 = CARTESIAN_POINT ( 'NONE',  ( 13.30024417629429756, -284.8332986952365786, -214.2132067574345058 ) ) ;
#6679 = CARTESIAN_POINT ( 'NONE',  ( 13.77899791739798196, -282.7684531203459528, -215.4114174452151929 ) ) ;
#6680 = CARTESIAN_POINT ( 'NONE',  ( -103.9275401027235830, -296.0222580210623846, -239.7475550269165581 ) ) ;
#6681 = ORIENTED_EDGE ( 'NONE', *, *, #40020, .F. ) ;
#6682 = DIRECTION ( 'NONE',  ( -0.000000000000000000, 1.000000000000000000, -0.000000000000000000 ) ) ;
#6683 = CARTESIAN_POINT ( 'NONE',  ( -59.41090076414670307, -285.3190492716215090, -341.7232149109100305 ) ) ;
#6684 = DIRECTION ( 'NONE',  ( 0.9951408606192333473, 1.205805641958531838E-17, 0.09846150276129089773 ) ) ;
#6685 = CARTESIAN_POINT ( 'NONE',  ( -110.4683760289727132, -287.8380690714490129, -287.0191576251351080 ) ) ;
#6686 = CARTESIAN_POINT ( 'NONE',  ( 37.07979331617996621, -274.9891136004775376, -289.4817909455644553 ) ) ;
#6687 = EDGE_CURVE ( 'NONE', #77289, #81908, #71811, .T. ) ;
#6688 = EDGE_CURVE ( 'NONE', #19742, #26019, #57841, .T. ) ;
#6689 = CARTESIAN_POINT ( 'NONE',  ( -0.08912516867963633793, -292.3961869890320600, -207.5817769267703454 ) ) ;
#6690 = CARTESIAN_POINT ( 'NONE',  ( 7.549496466245935622, -282.1970928417822506, -211.8543871336078155 ) ) ;
#6691 = CARTESIAN_POINT ( 'NONE',  ( 29.89137663140893864, -277.5579937415433847, -300.7938931191723100 ) ) ;
#6692 = CARTESIAN_POINT ( 'NONE',  ( -55.54409579114047801, -284.7072420986251586, -344.5721621971557056 ) ) ;
#6693 = CARTESIAN_POINT ( 'NONE',  ( 8.027426942944480004, -281.2113236907149485, -328.1215350966822371 ) ) ;
#6694 = CARTESIAN_POINT ( 'NONE',  ( -109.5506168704054204, -280.8136479806623811, -250.0434573790394381 ) ) ;
#6695 = CARTESIAN_POINT ( 'NONE',  ( -43.28975629721916363, -297.9791363799269561, -193.5379876853039889 ) ) ;
#6696 = CARTESIAN_POINT ( 'NONE',  ( 8.239354767634775811, -276.2813582099733480, -332.4865172601004701 ) ) ;
#6697 = CARTESIAN_POINT ( 'NONE',  ( 20.44854402476903488, -294.8210435425579590, -223.4197359779784904 ) ) ;
#6698 = FACE_OUTER_BOUND ( 'NONE', #91473, .T. ) ;
#6699 = CARTESIAN_POINT ( 'NONE',  ( 82.64890176555634582, -299.5541904835127980, -192.9651424135224147 ) ) ;
#6700 = CARTESIAN_POINT ( 'NONE',  ( -110.7773829546874538, -294.4540764799666590, -289.0550716743179009 ) ) ;
#6701 = CARTESIAN_POINT ( 'NONE',  ( -68.30295365371935645, -273.1418429257196863, -204.1704551858708214 ) ) ;
#6702 = CIRCLE ( 'NONE', #39905, 0.5000000000000004441 ) ;
#6703 = CARTESIAN_POINT ( 'NONE',  ( -16.67587515589574565, -296.3101544459350976, -343.8708198234176621 ) ) ;
#6704 = CARTESIAN_POINT ( 'NONE',  ( 21.98888790928170067, -295.4111832956580201, -318.8367466605033655 ) ) ;
#6705 = CARTESIAN_POINT ( 'NONE',  ( -28.94268546668699216, -290.9455890379921925, -344.7216248270497090 ) ) ;
#6706 = CARTESIAN_POINT ( 'NONE',  ( -46.14851910969489523, -275.1638176593491494, -344.7263281219547935 ) ) ;
#6707 = AXIS2_PLACEMENT_3D ( 'NONE', #16995, #45861, #74768 ) ;
#6708 = CARTESIAN_POINT ( 'NONE',  ( -98.04609444020337605, -279.8820406440989359, -313.4679384391710073 ) ) ;
#6709 = CARTESIAN_POINT ( 'NONE',  ( -111.6809736828326720, -294.5819116204035026, -274.2323713548228739 ) ) ;
#6710 = CARTESIAN_POINT ( 'NONE',  ( 34.44646749587986534, -283.7245050397887667, -294.7475342079135885 ) ) ;
#6711 = CARTESIAN_POINT ( 'NONE',  ( -27.78268987509830268, -285.0967239093956209, -197.6778916086147433 ) ) ;
#6712 = CARTESIAN_POINT ( 'NONE',  ( 123.4450140854237645, 148.1040090397345352, -262.7932479617338117 ) ) ;
#6713 = ORIENTED_EDGE ( 'NONE', *, *, #73275, .T. ) ;
#6714 = CARTESIAN_POINT ( 'NONE',  ( -108.0480724537290058, -284.4595844093128676, -252.1211508938320662 ) ) ;
#6715 = CARTESIAN_POINT ( 'NONE',  ( 1.206655381343710864, -281.6335901744072885, -204.0019679940370736 ) ) ;
#6716 = CARTESIAN_POINT ( 'NONE',  ( -109.8537878895348285, -283.0342814121304400, -295.0594144146552367 ) ) ;
#6717 = CIRCLE ( 'NONE', #52044, 9.103929867429224387 ) ;
#6718 = CARTESIAN_POINT ( 'NONE',  ( -72.41004682434640927, -280.5408137560759769, -202.0601189151636277 ) ) ;
#6719 = CARTESIAN_POINT ( 'NONE',  ( -105.7154506062859411, -279.6315352972225128, -304.3582219816107113 ) ) ;
#6720 = CARTESIAN_POINT ( 'NONE',  ( -82.08285599513421005, -276.9094976428775681, -214.2051214447836571 ) ) ;
#6721 = CARTESIAN_POINT ( 'NONE',  ( 66.05521907569730899, 47.24546878876408584, -318.8896612879527197 ) ) ;
#6722 = ORIENTED_EDGE ( 'NONE', *, *, #93228, .F. ) ;
#6723 = CARTESIAN_POINT ( 'NONE',  ( -76.26993376521713230, -299.5323573760761064, -206.1947854090703061 ) ) ;
#6724 = AXIS2_PLACEMENT_3D ( 'NONE', #80545, #43186, #79641 ) ;
#6725 = CARTESIAN_POINT ( 'NONE',  ( -71.67628606350481846, -277.6163352684956180, -204.0671329830324794 ) ) ;
#6726 = CARTESIAN_POINT ( 'NONE',  ( -69.21877995007181994, -293.3987208059937757, -201.3699690410987557 ) ) ;
#6727 = CARTESIAN_POINT ( 'NONE',  ( 23.01246486512854972, -293.4749351197648366, -311.6960472579104362 ) ) ;
#6728 = CARTESIAN_POINT ( 'NONE',  ( -110.7250515336934740, -289.7671005403453250, -293.6525386480440716 ) ) ;
#6730 = CARTESIAN_POINT ( 'NONE',  ( -24.98806372102210460, -284.6120460767558598, -197.5505584061987463 ) ) ;
#6729 = CARTESIAN_POINT ( 'NONE',  ( -13.97958449701159900, -293.3295739833139351, -343.1128729099827410 ) ) ;
#6731 = CARTESIAN_POINT ( 'NONE',  ( 7.402194449093554951, -294.5301292013162424, -211.1255764927018106 ) ) ;
#6732 = CARTESIAN_POINT ( 'NONE',  ( 29.77159426834535694, -283.2694102619713021, -300.4369155396558995 ) ) ;
#6733 = ORIENTED_EDGE ( 'NONE', *, *, #30878, .F. ) ;
#6734 = CARTESIAN_POINT ( 'NONE',  ( -113.7737673442578625, -291.5898537722490005, -262.6724811960321517 ) ) ;
#6735 = CARTESIAN_POINT ( 'NONE',  ( -43.76274118921946865, -280.4613092305531836, -197.5320077233581060 ) ) ;
#6736 = CARTESIAN_POINT ( 'NONE',  ( -2.163559205135533237, -293.3918340353606595, -338.4089476390099094 ) ) ;
#6737 = AXIS2_PLACEMENT_3D ( 'NONE', #49061, #37508, #44146 ) ;
#6738 = CARTESIAN_POINT ( 'NONE',  ( 0.6483754924009604848, -289.3622482158037315, -337.2113146170569280 ) ) ;
#6739 = CARTESIAN_POINT ( 'NONE',  ( -34.66268009850591625, -289.5116761196070456, -347.2529234958047937 ) ) ;
#6740 = CARTESIAN_POINT ( 'NONE',  ( 13.13802065155954324, -286.9480231644328114, -217.5581098758366920 ) ) ;
#6741 = ORIENTED_EDGE ( 'NONE', *, *, #39378, .T. ) ;
#6742 = CARTESIAN_POINT ( 'NONE',  ( 195.0233977251112947, 26.09208739110615838, 13.58423960365109195 ) ) ;
#6743 = CARTESIAN_POINT ( 'NONE',  ( -47.44306142105438795, -297.0396529500850988, -345.4495190763924484 ) ) ;
#6744 = CARTESIAN_POINT ( 'NONE',  ( -62.66591989841295884, -296.4141373707665821, -198.1670589112384846 ) ) ;
#6745 = CARTESIAN_POINT ( 'NONE',  ( -110.4040180262971660, -277.5356249193470717, -276.0853772726320585 ) ) ;
#6746 = CARTESIAN_POINT ( 'NONE',  ( -81.21014955545675207, -272.9814238445582077, -207.0898685236535641 ) ) ;
#6747 = CARTESIAN_POINT ( 'NONE',  ( -34.29169290404533399, -293.4929862397166289, -343.9913102248517021 ) ) ;
#6748 = CARTESIAN_POINT ( 'NONE',  ( 5.748759157823479349, -276.4048141683725817, -210.1214935816987293 ) ) ;
#6749 = CARTESIAN_POINT ( 'NONE',  ( -105.5046300928302259, -271.0818495909373951, -240.8254948327308114 ) ) ;
#6750 = CARTESIAN_POINT ( 'NONE',  ( 32.17217576012168934, -294.4440418615810131, -246.6455947132782285 ) ) ;
#6751 = CARTESIAN_POINT ( 'NONE',  ( -105.2430635470345521, -297.2632115875783256, -297.9949906519991600 ) ) ;
#6752 = CARTESIAN_POINT ( 'NONE',  ( 194.5881128153457098, -27.00396092263537540, 21.50000000000000000 ) ) ;
#6753 = CARTESIAN_POINT ( 'NONE',  ( -105.5145906721402582, -294.1369017818259408, -302.0231681110018371 ) ) ;
#6754 = CARTESIAN_POINT ( 'NONE',  ( -48.96278628175142700, -298.5593706151875040, -194.2926344110418029 ) ) ;
#6755 = CARTESIAN_POINT ( 'NONE',  ( 26.19570646661878754, -286.6336026538934334, -307.5882615394839945 ) ) ;
#6756 = CARTESIAN_POINT ( 'NONE',  ( -109.1178196114578043, -274.8347243191913094, -248.4300993436286547 ) ) ;
#6757 = CARTESIAN_POINT ( 'NONE',  ( -111.7603764912722113, -273.2914829440908306, -250.6280109516932839 ) ) ;
#6758 = CARTESIAN_POINT ( 'NONE',  ( -101.4838653887274518, -296.4092326601953573, -305.2591139474765214 ) ) ;
#6759 = CARTESIAN_POINT ( 'NONE',  ( -110.4953971236689938, -280.7637905563339018, -252.2265270257778695 ) ) ;
#6760 = CARTESIAN_POINT ( 'NONE',  ( -28.26676924479576414, -278.8497063325251020, -194.3411066717031872 ) ) ;
#6761 = CARTESIAN_POINT ( 'NONE',  ( -79.11132393653237216, -282.9484398959698410, -334.9259018302595905 ) ) ;
#6762 = CARTESIAN_POINT ( 'NONE',  ( 36.78514330758493145, -275.1579199981619581, -290.8680523908661826 ) ) ;
#6763 = CARTESIAN_POINT ( 'NONE',  ( -9.138071579272676104, -278.8147377829336619, -199.5727308531745621 ) ) ;
#6764 = CARTESIAN_POINT ( 'NONE',  ( -42.28346906920241111, -277.9898048292583326, -195.3570691104125103 ) ) ;
#6765 = CARTESIAN_POINT ( 'NONE',  ( -110.9302533213375170, -271.1630414604915700, -267.5971677107045252 ) ) ;
#6766 = CARTESIAN_POINT ( 'NONE',  ( 30.76387501785565348, -277.9662554485501573, -301.8941007075530365 ) ) ;
#6767 = CARTESIAN_POINT ( 'NONE',  ( 175.2296996224750103, 134.0000000000000284, 0.000000000000000000 ) ) ;
#6768 = CARTESIAN_POINT ( 'NONE',  ( 14.32908211502242857, -290.7937678050400336, -215.4393165220135131 ) ) ;
#6769 = CARTESIAN_POINT ( 'NONE',  ( -72.17226653832392458, -291.6043158448395616, -201.6746056895983941 ) ) ;
#6770 = CARTESIAN_POINT ( 'NONE',  ( 13.65843380474318991, -278.3402571758993531, -325.6498661402596326 ) ) ;
#6771 = CARTESIAN_POINT ( 'NONE',  ( 10.78751916717431314, -272.7169704748302479, -212.7728417827638623 ) ) ;
#6772 = DIRECTION ( 'NONE',  ( 0.000000000000000000, 0.000000000000000000, -1.000000000000000000 ) ) ;
#6773 = DIRECTION ( 'NONE',  ( 0.000000000000000000, 0.000000000000000000, 1.000000000000000000 ) ) ;
#6774 = CARTESIAN_POINT ( 'NONE',  ( -105.0402076491763808, -282.9781974211392139, -237.9633363029016664 ) ) ;
#6775 = CARTESIAN_POINT ( 'NONE',  ( 151.4851178187871312, 20.00000000000000000, 3.492110388858666870 ) ) ;
#6776 = CARTESIAN_POINT ( 'NONE',  ( 32.72129114376627967, -292.6353244162791043, -292.2313662452424978 ) ) ;
#6777 = CARTESIAN_POINT ( 'NONE',  ( 36.78760162229094277, -285.6290532716450912, -265.5295249872702357 ) ) ;
#6778 = CARTESIAN_POINT ( 'NONE',  ( 140.6539576904058606, 276.0000000000000568, -10.49999999999999822 ) ) ;
#6779 = DIRECTION ( 'NONE',  ( 0.000000000000000000, 0.000000000000000000, 1.000000000000000000 ) ) ;
#6780 = CARTESIAN_POINT ( 'NONE',  ( -41.16599750196969154, -293.1001064511826257, -345.2764686778536998 ) ) ;
#6781 = CARTESIAN_POINT ( 'NONE',  ( -113.4586947301442450, -283.1087249867977107, -264.2840055189940358 ) ) ;
#6782 = CARTESIAN_POINT ( 'NONE',  ( -109.0719931358301977, -280.3787816277598495, -253.0058455138177180 ) ) ;
#6783 = CARTESIAN_POINT ( 'NONE',  ( -57.66543618221821532, -287.0006128014463229, -196.4483851348814483 ) ) ;
#6784 = CARTESIAN_POINT ( 'NONE',  ( -19.96586882316425360, -278.5122215547523865, -196.3337278217716175 ) ) ;
#6785 = CARTESIAN_POINT ( 'NONE',  ( 21.99157979706356869, -286.9567232072396905, -227.7487042747412147 ) ) ;
#6786 = VECTOR ( 'NONE', #15157, 1000.000000000000000 ) ;
#6787 = CARTESIAN_POINT ( 'NONE',  ( -73.11267154320242412, -278.9614349638636668, -334.6858972757340212 ) ) ;
#6788 = CARTESIAN_POINT ( 'NONE',  ( -110.5534815158028294, -279.3512023371334294, -270.6488695304282714 ) ) ;
#6789 = EDGE_CURVE ( 'NONE', #59928, #48925, #82513, .T. ) ;
#6790 = CARTESIAN_POINT ( 'NONE',  ( -43.55631160385355827, -287.9540348119309670, -195.2104912067817963 ) ) ;
#6791 = ORIENTED_EDGE ( 'NONE', *, *, #15024, .T. ) ;
#6792 = CARTESIAN_POINT ( 'NONE',  ( -108.8878111973532157, -296.7481459817725522, -241.7546394066846744 ) ) ;
#6793 = CARTESIAN_POINT ( 'NONE',  ( 24.89449991426167230, -290.0915546015717723, -311.5973648834024630 ) ) ;
#6794 = DIRECTION ( 'NONE',  ( 8.659560562354937789E-17, -0.7071067811865472397, 0.7071067811865479058 ) ) ;
#6795 = CARTESIAN_POINT ( 'NONE',  ( -119.3990491898856732, -281.0519495502701943, -270.3937649182068412 ) ) ;
#6796 = ORIENTED_EDGE ( 'NONE', *, *, #27340, .T. ) ;
#6797 = CARTESIAN_POINT ( 'NONE',  ( -65.51583670687578831, -271.6845087381012149, -200.6605136050853844 ) ) ;
#6798 = EDGE_CURVE ( 'NONE', #51305, #83756, #89011, .T. ) ;
#6799 = CARTESIAN_POINT ( 'NONE',  ( 1.345532328506472419, -292.9441950195819118, -336.0097162928116745 ) ) ;
#6800 = CARTESIAN_POINT ( 'NONE',  ( -53.16881202234307580, -294.7681172037196120, -341.7397970965650416 ) ) ;
#6801 = CARTESIAN_POINT ( 'NONE',  ( -11.79965379505463297, -287.9109661624901833, -201.2357852788498462 ) ) ;
#6802 = AXIS2_PLACEMENT_3D ( 'NONE', #82364, #1898, #46365 ) ;
#6803 = CARTESIAN_POINT ( 'NONE',  ( 19.60156281330873540, -282.6506941180336412, -223.0610284341442480 ) ) ;
#6804 = CARTESIAN_POINT ( 'NONE',  ( -7.136018920196121940, -290.0888730158718545, -340.5623089576561711 ) ) ;
#6805 = CARTESIAN_POINT ( 'NONE',  ( -97.75979101718108666, -291.2364365761283693, -317.2967395087235900 ) ) ;
#6806 = CARTESIAN_POINT ( 'NONE',  ( -43.06068304860170315, -285.1243805312324184, -345.1942184142553742 ) ) ;
#6807 = CARTESIAN_POINT ( 'NONE',  ( -93.33253387578001536, -277.9963940603283845, -323.2961784113347221 ) ) ;
#6808 = CARTESIAN_POINT ( 'NONE',  ( 34.98405915197686511, -291.9137872170805394, -292.4082077718963433 ) ) ;
#6809 = CARTESIAN_POINT ( 'NONE',  ( -14.22573591802529513, -280.1770498845876318, -196.8569211956442189 ) ) ;
#6810 = CARTESIAN_POINT ( 'NONE',  ( -68.82767353928764464, -275.4942247610514414, -203.1199678787864684 ) ) ;
#6811 = CARTESIAN_POINT ( 'NONE',  ( -20.25526795762937127, -288.7662352645560304, -195.3538533559490702 ) ) ;
#6812 = CARTESIAN_POINT ( 'NONE',  ( 36.30865968177557335, -273.5549337528162823, -251.6635642317122006 ) ) ;
#6813 = CARTESIAN_POINT ( 'NONE',  ( 160.6539576904058606, 293.9636489450775230, -7.999911143031724237 ) ) ;
#6814 = CARTESIAN_POINT ( 'NONE',  ( -46.45792522568929428, -279.4411332258046059, -197.8194021589485203 ) ) ;
#6815 = CARTESIAN_POINT ( 'NONE',  ( 23.21363838431332738, -277.3871158940817736, -317.2978494860217893 ) ) ;
#6816 = CARTESIAN_POINT ( 'NONE',  ( -103.0667027729937359, -298.4244180156493940, -237.1477701089136758 ) ) ;
#6817 = CARTESIAN_POINT ( 'NONE',  ( -111.9931577696146121, -283.3858076672752304, -288.3047849279770389 ) ) ;
#6818 = CARTESIAN_POINT ( 'NONE',  ( -109.7059863760641463, -292.5144412789284729, -254.8245774364963268 ) ) ;
#6819 = CARTESIAN_POINT ( 'NONE',  ( -112.7556112951421596, -274.2948001941855978, -259.0834997254065115 ) ) ;
#6820 = CARTESIAN_POINT ( 'NONE',  ( -113.6901519526754072, -273.9388369354260817, -264.6796541390648372 ) ) ;
#6821 = CARTESIAN_POINT ( 'NONE',  ( -3.484979095569499918, -296.6043879013998890, -337.1118981292720491 ) ) ;
#6822 = CARTESIAN_POINT ( 'NONE',  ( -83.95613797422839752, -281.6935959865587620, -328.9692612425107541 ) ) ;
#6823 = CARTESIAN_POINT ( 'NONE',  ( -107.2394501601043402, -290.6329687966003803, -237.9843448037091491 ) ) ;
#6824 = CARTESIAN_POINT ( 'NONE',  ( 14.86406471174902499, -274.3325507775545020, -323.7847882684168894 ) ) ;
#6825 = CARTESIAN_POINT ( 'NONE',  ( -15.66079108021488331, -287.9281089825261688, -197.2557854055254438 ) ) ;
#6826 = CARTESIAN_POINT ( 'NONE',  ( -98.55008013413456069, -290.0307759435599451, -229.9234233872433038 ) ) ;
#6827 = ORIENTED_EDGE ( 'NONE', *, *, #19944, .T. ) ;
#6828 = CARTESIAN_POINT ( 'NONE',  ( -110.2253551251877326, -288.8343259320022298, -293.4814212516201906 ) ) ;
#6829 = CARTESIAN_POINT ( 'NONE',  ( -109.7204949041569790, -290.3512635300337479, -260.3220032173885556 ) ) ;
#6830 = ORIENTED_EDGE ( 'NONE', *, *, #48291, .F. ) ;
#6831 = CARTESIAN_POINT ( 'NONE',  ( 36.09339810295367101, -288.9109374044105039, -292.5150998761214396 ) ) ;
#6832 = CARTESIAN_POINT ( 'NONE',  ( -48.60691564909392071, -277.5326890548631695, -342.5594715398640346 ) ) ;
#6833 = CARTESIAN_POINT ( 'NONE',  ( -53.23865245455921524, -294.1715945164720551, -345.4406361985554099 ) ) ;
#6834 = CARTESIAN_POINT ( 'NONE',  ( -41.55524485777256416, -283.7551821413716198, -347.1959179724448745 ) ) ;
#6835 = CARTESIAN_POINT ( 'NONE',  ( -112.9782761821414283, -285.0679061440110900, -255.7710135701557590 ) ) ;
#6836 = CARTESIAN_POINT ( 'NONE',  ( 11.31675292249747855, -281.0823067329237119, -215.9144244794644578 ) ) ;
#6837 = CARTESIAN_POINT ( 'NONE',  ( 194.1796378510228749, 279.1575638736977112, -125.9076664125385037 ) ) ;
#6838 = CARTESIAN_POINT ( 'NONE',  ( -100.6270238236691341, -247.1647810672108676, -333.6273736269536130 ) ) ;
#6839 = CARTESIAN_POINT ( 'NONE',  ( -103.7292136647523222, -253.6277699525920752, -324.3870440700492850 ) ) ;
#6840 = CARTESIAN_POINT ( 'NONE',  ( -106.4555858548876159, -272.0677620063422069, -246.3637738258152865 ) ) ;
#6841 = CARTESIAN_POINT ( 'NONE',  ( 33.81251353248127600, -274.2406337770659661, -252.7173102048476778 ) ) ;
#6842 = CARTESIAN_POINT ( 'NONE',  ( -99.96207412128785563, -295.4662012159903384, -315.1522681502689807 ) ) ;
#6843 = CARTESIAN_POINT ( 'NONE',  ( 103.9790695402631542, 114.2035196735941014, -279.8796163930391003 ) ) ;
#6844 = CARTESIAN_POINT ( 'NONE',  ( -69.90654276699919478, -272.3170824185372112, -201.1165352077644570 ) ) ;
#6845 = CARTESIAN_POINT ( 'NONE',  ( -92.78289610387243158, -299.1067106019873449, -220.9937272232280350 ) ) ;
#6846 = CARTESIAN_POINT ( 'NONE',  ( 26.13035353343015998, -289.3736076648922904, -307.5095966231827447 ) ) ;
#6847 = CARTESIAN_POINT ( 'NONE',  ( -109.0156728521508143, -291.8340815830548536, -254.9641147490587798 ) ) ;
#6848 = EDGE_LOOP ( 'NONE', ( #78571, #68659, #63310, #44201 ) ) ;
#6849 = CARTESIAN_POINT ( 'NONE',  ( -62.77841576719750094, -298.6701996495469302, -197.9332662254898878 ) ) ;
#6850 = CARTESIAN_POINT ( 'NONE',  ( 11.17023993891524292, -287.2377583740539535, -215.6618384412749663 ) ) ;
#6851 = CARTESIAN_POINT ( 'NONE',  ( -4.562120616607214352, -295.4340278558877912, -339.8712993806753957 ) ) ;
#6852 = CARTESIAN_POINT ( 'NONE',  ( -5.817178022079361632, -295.1410031709812074, -340.5446731036466304 ) ) ;
#6853 = CARTESIAN_POINT ( 'NONE',  ( -0.09277589007679333533, -292.7294932912904528, -207.5796107721051555 ) ) ;
#6854 = VERTEX_POINT ( 'NONE', #46855 ) ;
#6855 = CARTESIAN_POINT ( 'NONE',  ( -13.53971524851210440, -276.2789602045210700, -198.6479412838396001 ) ) ;
#6856 = ORIENTED_EDGE ( 'NONE', *, *, #63349, .F. ) ;
#6857 = CARTESIAN_POINT ( 'NONE',  ( -93.02488084551742986, -278.7869767283418696, -217.1915935700891112 ) ) ;
#6858 = CARTESIAN_POINT ( 'NONE',  ( 30.92249417963552105, -273.5786587781303183, -242.1832972769480250 ) ) ;
#6859 = CARTESIAN_POINT ( 'NONE',  ( -109.4362405200949411, -273.8099651867767648, -256.8000895874391745 ) ) ;
#6860 = CARTESIAN_POINT ( 'NONE',  ( 35.82134529165360703, -276.4375555199185328, -266.1134143587142944 ) ) ;
#6861 = CARTESIAN_POINT ( 'NONE',  ( 11.12193141546653763, -276.4723563065655867, -211.7671220282612978 ) ) ;
#6862 = CARTESIAN_POINT ( 'NONE',  ( 31.50655769710617449, -273.9717737252917686, -300.9931958472498650 ) ) ;
#6863 = CARTESIAN_POINT ( 'NONE',  ( -109.9046191018525320, -297.0815070544902596, -279.6269827524902780 ) ) ;
#6864 =( GEOMETRIC_REPRESENTATION_CONTEXT ( 3 ) GLOBAL_UNCERTAINTY_ASSIGNED_CONTEXT ( ( #83551 ) ) GLOBAL_UNIT_ASSIGNED_CONTEXT ( ( #64964, #56918, #84346 ) ) REPRESENTATION_CONTEXT ( 'NONE', 'WORKASPACE' ) );
#6865 = CARTESIAN_POINT ( 'NONE',  ( 16.57862423517864769, -292.8409554647091113, -320.4407898865063089 ) ) ;
#6866 = DIRECTION ( 'NONE',  ( -1.000000000000000000, 0.000000000000000000, 0.000000000000000000 ) ) ;
#6867 = CARTESIAN_POINT ( 'NONE',  ( -112.1138860555012258, -278.8169008992088607, -288.5449083783926767 ) ) ;
#6868 = CARTESIAN_POINT ( 'NONE',  ( 34.70750918302831423, -275.8777800387776438, -282.4101755853341729 ) ) ;
#6869 = EDGE_CURVE ( 'NONE', #27807, #55409, #9795, .T. ) ;
#6870 = AXIS2_PLACEMENT_3D ( 'NONE', #11708, #3203, #90746 ) ;
#6871 = CARTESIAN_POINT ( 'NONE',  ( -18.28854320631695174, -284.9773865967538882, -196.2099722438857157 ) ) ;
#6872 = CARTESIAN_POINT ( 'NONE',  ( -81.90466411633786947, -299.4471366281514975, -209.7640378534141519 ) ) ;
#6873 = CARTESIAN_POINT ( 'NONE',  ( 82.62449080995027373, -301.4714224534961886, -196.9739619934580048 ) ) ;
#6874 = CARTESIAN_POINT ( 'NONE',  ( 23.67437527527419050, -286.1893846156170298, -229.9005749589418031 ) ) ;
#6875 = CARTESIAN_POINT ( 'NONE',  ( -93.84954952996797317, -277.4622521423027592, -222.5416621415513418 ) ) ;
#6876 = CARTESIAN_POINT ( 'NONE',  ( -79.37669450963343820, -278.0467752045547059, -209.9588484624203772 ) ) ;
#6877 = CARTESIAN_POINT ( 'NONE',  ( -55.70587383441166907, -285.2885709944625887, -343.1309728289907639 ) ) ;
#6878 = CARTESIAN_POINT ( 'NONE',  ( -68.19041699205519080, -278.6716325336151954, -336.9743919653828925 ) ) ;
#6879 = CARTESIAN_POINT ( 'NONE',  ( 185.2519943799831879, 3.000000000000000000, 9.000000000000001776 ) ) ;
#6880 = CARTESIAN_POINT ( 'NONE',  ( 35.82353380483935723, -273.6801225773508577, -248.8859689579149688 ) ) ;
#6881 = CARTESIAN_POINT ( 'NONE',  ( 34.94120171520702911, -276.0587111588223479, -259.3648184049165479 ) ) ;
#6882 = CARTESIAN_POINT ( 'NONE',  ( 36.97803798745025716, -283.4038447058798624, -258.7723949708142186 ) ) ;
#6883 = DIRECTION ( 'NONE',  ( 1.000000000000000000, 0.000000000000000000, 0.000000000000000000 ) ) ;
#6884 = CARTESIAN_POINT ( 'NONE',  ( 37.66428058273490365, -289.5940847440669472, -279.9163628558444543 ) ) ;
#6885 = CARTESIAN_POINT ( 'NONE',  ( 18.08390197224154150, -290.8465964040101426, -219.8149839727543906 ) ) ;
#6886 = CARTESIAN_POINT ( 'NONE',  ( -6.305593342992922068, -273.1534952555061295, -203.7427754997524971 ) ) ;
#6887 = CARTESIAN_POINT ( 'NONE',  ( -11.81356043243047438, -290.5274942293348772, -200.5985058486490118 ) ) ;
#6888 = CARTESIAN_POINT ( 'NONE',  ( -90.78337343436103879, -230.3218577325732781, -348.1307343985224634 ) ) ;
#6889 = CARTESIAN_POINT ( 'NONE',  ( 208.4306832106271088, -74.55766379199613425, -7.500000000000013323 ) ) ;
#6890 = CARTESIAN_POINT ( 'NONE',  ( -104.5544964833918442, -288.5607208999405771, -306.4879467546468277 ) ) ;
#6891 = CARTESIAN_POINT ( 'NONE',  ( -13.00673725730827712, -284.6039669252799627, -198.3765113330170209 ) ) ;
#6892 = CARTESIAN_POINT ( 'NONE',  ( -3.333066667267752248, -284.0191928491674958, -335.6346259346908596 ) ) ;
#6893 = CARTESIAN_POINT ( 'NONE',  ( -99.16201929787168012, -284.8143519411291322, -309.5820160768043934 ) ) ;
#6894 = EDGE_CURVE ( 'NONE', #36590, #74948, #25979, .T. ) ;
#6895 = CARTESIAN_POINT ( 'NONE',  ( -55.81059605911486443, -293.7955613790688858, -197.2504656760841328 ) ) ;
#6896 = CARTESIAN_POINT ( 'NONE',  ( -35.52854025202275778, -274.4075681216612566, -193.3904917673858677 ) ) ;
#6897 = CARTESIAN_POINT ( 'NONE',  ( -95.30249646358021209, -287.9670393870879934, -318.8565526130448688 ) ) ;
#6898 = CARTESIAN_POINT ( 'NONE',  ( -22.93890052929812384, -276.8729102018812682, -346.0562929192211072 ) ) ;
#6899 = CARTESIAN_POINT ( 'NONE',  ( 35.38352806009255858, -295.7496848076312972, -287.2367871789406877 ) ) ;
#6900 = CARTESIAN_POINT ( 'NONE',  ( -48.18343439339133027, -253.0206516614774728, -465.6442049081569508 ) ) ;
#6901 = CARTESIAN_POINT ( 'NONE',  ( -83.11486472582501506, -282.3784722272463910, -327.9247881687138033 ) ) ;
#6902 = CARTESIAN_POINT ( 'NONE',  ( -56.03294299444257121, -277.8114028498940797, -197.6739637014906066 ) ) ;
#6903 = CARTESIAN_POINT ( 'NONE',  ( 7.424657929120416000, -297.0036273313833703, -194.1730573998131888 ) ) ;
#6904 = CARTESIAN_POINT ( 'NONE',  ( 31.35470757426955046, -275.2350516737913608, -295.5020920236807456 ) ) ;
#6905 = CARTESIAN_POINT ( 'NONE',  ( -12.04017218948744805, -293.9074870923922163, -201.0930043797890221 ) ) ;
#6906 = CARTESIAN_POINT ( 'NONE',  ( 35.44216684457012434, -294.6060335039535971, -278.9261934527773974 ) ) ;
#6907 = CARTESIAN_POINT ( 'NONE',  ( -37.66994488711937095, -296.3713133498129650, -346.8802599108891513 ) ) ;
#6908 = CARTESIAN_POINT ( 'NONE',  ( -86.49154197761680507, -295.5913062068389081, -324.3360478171921955 ) ) ;
#6909 = CARTESIAN_POINT ( 'NONE',  ( -97.35373956792248862, -291.9374303022664776, -315.3664915234331261 ) ) ;
#6910 = CARTESIAN_POINT ( 'NONE',  ( -83.88151497312459526, -283.8378941471897861, -331.7717632045762457 ) ) ;
#6911 = CARTESIAN_POINT ( 'NONE',  ( 4.205934018149265263, -272.7448848494808544, -206.9419376233988999 ) ) ;
#6912 = CARTESIAN_POINT ( 'NONE',  ( -2.221011949415980347, -286.3372983410575898, -201.8223747401436867 ) ) ;
#6913 = CARTESIAN_POINT ( 'NONE',  ( -18.57971230128489992, -278.7891912710617248, -342.6095408891184775 ) ) ;
#6914 = EDGE_CURVE ( 'NONE', #36583, #39232, #31706, .T. ) ;
#6915 = CARTESIAN_POINT ( 'NONE',  ( -87.84813418538628582, -284.3835941454530598, -217.3280286275817730 ) ) ;
#6916 = CARTESIAN_POINT ( 'NONE',  ( -3.974031079240675890, -286.6120053661029488, -337.5438045115778323 ) ) ;
#6917 = CARTESIAN_POINT ( 'NONE',  ( -104.5266604826868644, -260.4492150524036447, -315.3738353148558531 ) ) ;
#6918 = CARTESIAN_POINT ( 'NONE',  ( -4.561334620148513430, -286.0038710971283535, -205.0661252264309553 ) ) ;
#6919 = CARTESIAN_POINT ( 'NONE',  ( -37.30230267540845546, -283.9928807237935189, -347.1388402226243670 ) ) ;
#6920 = CARTESIAN_POINT ( 'NONE',  ( -57.24149715323748921, -288.3614519093280819, -344.5565880092141242 ) ) ;
#6921 = CARTESIAN_POINT ( 'NONE',  ( -102.7356303687088968, -280.6688284196642371, -231.1423127269929978 ) ) ;
#6922 = CARTESIAN_POINT ( 'NONE',  ( -112.8099441430402976, -279.7091848142044910, -282.9246532532335436 ) ) ;
#6923 = CARTESIAN_POINT ( 'NONE',  ( -49.13981870071936697, -279.7309192988812470, -198.3208209077055528 ) ) ;
#6924 = CARTESIAN_POINT ( 'NONE',  ( -43.64561485211081049, -275.9521429260435639, -195.9311257194189579 ) ) ;
#6925 = CARTESIAN_POINT ( 'NONE',  ( 29.47564115329079470, -293.0549537924198376, -232.0930777389227444 ) ) ;
#6926 = CARTESIAN_POINT ( 'NONE',  ( 20.77864682589926204, -286.2199339869449091, -317.1999061506106159 ) ) ;
#6927 = AXIS2_PLACEMENT_3D ( 'NONE', #73676, #65670, #8787 ) ;
#6928 = CARTESIAN_POINT ( 'NONE',  ( -88.13157978398666614, -292.9551855496760595, -213.5559374248252595 ) ) ;
#6929 = CARTESIAN_POINT ( 'NONE',  ( -109.0787717184319234, -295.6716125633915908, -255.2005293943817037 ) ) ;
#6930 = CARTESIAN_POINT ( 'NONE',  ( -4.163817024218998242, -284.5313639721014169, -336.9985119457261931 ) ) ;
#6931 = CARTESIAN_POINT ( 'NONE',  ( -80.17060626431941728, -295.3170267777505273, -329.5030851958939593 ) ) ;
#6932 = CARTESIAN_POINT ( 'NONE',  ( 39.13179638315010322, -294.5593645940811030, -264.5907765352137062 ) ) ;
#6933 = CARTESIAN_POINT ( 'NONE',  ( -7.966087386808290205, -281.0988606643620074, -203.4074090307868516 ) ) ;
#6934 = CARTESIAN_POINT ( 'NONE',  ( 37.99016587947605217, -274.4257136689749359, -255.5986596014465135 ) ) ;
#6935 = CARTESIAN_POINT ( 'NONE',  ( -38.90976897433122161, -289.7227510883251398, -347.2431961744549085 ) ) ;
#6936 = CARTESIAN_POINT ( 'NONE',  ( -11.15161057318202786, -280.8541481673136104, -341.5110442238404858 ) ) ;
#6937 = CARTESIAN_POINT ( 'NONE',  ( -114.3689209509520595, -290.8745286872411384, -271.2327552579352528 ) ) ;
#6938 = CARTESIAN_POINT ( 'NONE',  ( 28.24861413923276388, -288.3200305144690105, -302.4547024036314156 ) ) ;
#6939 = CARTESIAN_POINT ( 'NONE',  ( 140.6539576904058606, 131.0000000000000568, 11.50000000000000000 ) ) ;
#6940 = CARTESIAN_POINT ( 'NONE',  ( 166.0114646923310602, 231.9370847612306932, -191.0689560128921300 ) ) ;
#6941 = CARTESIAN_POINT ( 'NONE',  ( 103.1691430569825201, 114.4498183994276701, -279.5267493636292784 ) ) ;
#6942 = CARTESIAN_POINT ( 'NONE',  ( -37.30987171927208834, -295.5523547857347353, -200.3611179825600459 ) ) ;
#6943 = CARTESIAN_POINT ( 'NONE',  ( -96.53033456514194199, -278.3498422243019945, -227.3575450987400757 ) ) ;
#6944 = ORIENTED_EDGE ( 'NONE', *, *, #25879, .F. ) ;
#6945 = CARTESIAN_POINT ( 'NONE',  ( -22.11684334101605742, -279.1719741586950363, -198.5983022467686965 ) ) ;
#6946 = CARTESIAN_POINT ( 'NONE',  ( -35.52003169720737219, -273.7411135690103379, -193.3906927978415240 ) ) ;
#6947 = CARTESIAN_POINT ( 'NONE',  ( -53.96950941693697246, -170.4674300608036503, -362.0100880823835041 ) ) ;
#6948 = CARTESIAN_POINT ( 'NONE',  ( -69.69623604000952355, -278.2092778345290753, -201.1240814426776637 ) ) ;
#6949 = CARTESIAN_POINT ( 'NONE',  ( 13.00798148109448782, -280.3648095250903793, -325.4678903628616808 ) ) ;
#6950 = CARTESIAN_POINT ( 'NONE',  ( -100.7170786770327879, -298.8713338101152317, -228.4144446106088537 ) ) ;
#6951 = CARTESIAN_POINT ( 'NONE',  ( 24.48267372241567230, -294.5829724668028007, -309.3886089952530938 ) ) ;
#6952 = ORIENTED_EDGE ( 'NONE', *, *, #82203, .F. ) ;
#6953 = CARTESIAN_POINT ( 'NONE',  ( 1.558507642033911456, -287.2050156837075860, -332.7150858843626224 ) ) ;
#6954 = CARTESIAN_POINT ( 'NONE',  ( -34.11578406128840868, -274.7431362305676998, -193.5307447415462434 ) ) ;
#6955 = CARTESIAN_POINT ( 'NONE',  ( -52.63716048434380212, -298.0175154456912878, -198.9296210900367896 ) ) ;
#6956 = VERTEX_POINT ( 'NONE', #81914 ) ;
#6957 = DIRECTION ( 'NONE',  ( 0.000000000000000000, 0.000000000000000000, 1.000000000000000000 ) ) ;
#6958 = CARTESIAN_POINT ( 'NONE',  ( 175.2296996224750103, 250.5000000000000568, 0.000000000000000000 ) ) ;
#6959 = FACE_OUTER_BOUND ( 'NONE', #2706, .T. ) ;
#6960 = CARTESIAN_POINT ( 'NONE',  ( -35.66947508278408918, -281.1532613951632129, -197.0586240018850503 ) ) ;
#6961 = CARTESIAN_POINT ( 'NONE',  ( -35.38488858966578476, -281.8364996814060532, -194.3866839478937720 ) ) ;
#6962 = CARTESIAN_POINT ( 'NONE',  ( -90.92175429966927425, -282.8952702857436066, -320.2869253693708060 ) ) ;
#6963 = CARTESIAN_POINT ( 'NONE',  ( -72.73920005939122291, -281.4384729274287338, -205.1086660705969109 ) ) ;
#6964 = CARTESIAN_POINT ( 'NONE',  ( -5.999160243941402904, -275.1124203219407036, -337.0709891403882921 ) ) ;
#6965 = CARTESIAN_POINT ( 'NONE',  ( 184.7149167944524493, -12.49482340714361506, 13.00000000000000178 ) ) ;
#6966 = DIRECTION ( 'NONE',  ( -1.000000000000000000, 0.000000000000000000, 0.000000000000000000 ) ) ;
#6967 = CARTESIAN_POINT ( 'NONE',  ( -6.629830887579506893, -277.4619086557471519, -340.8092852775565689 ) ) ;
#6968 = CYLINDRICAL_SURFACE ( 'NONE', #21749, 7.999999999999992895 ) ;
#6969 = CARTESIAN_POINT ( 'NONE',  ( -99.99286380534586272, -276.5442098938995628, -314.1039800648590585 ) ) ;
#6970 = ORIENTED_EDGE ( 'NONE', *, *, #15737, .F. ) ;
#6971 = DIRECTION ( 'NONE',  ( -0.000000000000000000, -0.000000000000000000, 1.000000000000000000 ) ) ;
#6972 = CARTESIAN_POINT ( 'NONE',  ( -91.23930866183877697, -285.7937962642237153, -323.0247163826246037 ) ) ;
#6973 = ADVANCED_FACE ( 'NONE', ( #39742 ), #38826, .T. ) ;
#6974 = CARTESIAN_POINT ( 'NONE',  ( 33.46706107295545252, -292.5068771936378198, -251.9567417481746077 ) ) ;
#6975 = CARTESIAN_POINT ( 'NONE',  ( 36.28539530061574681, -287.1801322140648267, -292.5961028353279403 ) ) ;
#6976 = CARTESIAN_POINT ( 'NONE',  ( -19.55086886134803947, -284.5239598567427493, -198.5178139538606956 ) ) ;
#6978 = CARTESIAN_POINT ( 'NONE',  ( 16.73624348595687295, -286.5095859844233814, -320.9687456464587285 ) ) ;
#6977 = CARTESIAN_POINT ( 'NONE',  ( -110.8977533990320552, -283.1557861643560727, -268.1516061122723613 ) ) ;
#6979 = CARTESIAN_POINT ( 'NONE',  ( 29.68329294213124925, -283.1593296971832387, -300.3988542733939653 ) ) ;
#6980 = CARTESIAN_POINT ( 'NONE',  ( 22.88933240778906963, -272.9419774280616480, -225.6708128688526358 ) ) ;
#6981 = CARTESIAN_POINT ( 'NONE',  ( -103.7301433442240892, -282.4603815668274933, -307.8714469036783612 ) ) ;
#6982 = CARTESIAN_POINT ( 'NONE',  ( -64.84571742789454163, -297.4114969671805397, -340.1498183009070999 ) ) ;
#6983 = CARTESIAN_POINT ( 'NONE',  ( -96.13021995200431036, -283.1944355199664187, -223.5216221635462830 ) ) ;
#6984 = CARTESIAN_POINT ( 'NONE',  ( -87.70109466164885248, -280.2693397686472849, -217.1182879169194564 ) ) ;
#6985 = CARTESIAN_POINT ( 'NONE',  ( 35.02642474499729985, -289.8137000907473180, -290.7279003110270423 ) ) ;
#6986 = CARTESIAN_POINT ( 'NONE',  ( 195.4638858641033892, 26.97464251841893201, 13.94285838819634549 ) ) ;
#6987 = FACE_BOUND ( 'NONE', #78000, .T. ) ;
#6988 = CARTESIAN_POINT ( 'NONE',  ( 25.28540849312504335, -294.9035634149785210, -227.9943107898707240 ) ) ;
#6989 = AXIS2_PLACEMENT_3D ( 'NONE', #40541, #2272, #3185 ) ;
#6990 = CARTESIAN_POINT ( 'NONE',  ( -82.03096345067650930, -275.6612755223351883, -330.5929234470335132 ) ) ;
#6991 = CARTESIAN_POINT ( 'NONE',  ( -105.8554877771612581, -290.1994379943457716, -235.4584931781828061 ) ) ;
#6992 = CARTESIAN_POINT ( 'NONE',  ( -26.10548938036544087, -293.3065770096691836, -343.3007367206303115 ) ) ;
#6993 = CARTESIAN_POINT ( 'NONE',  ( -91.65002219283027785, -277.9422885543603456, -220.8449627097939469 ) ) ;
#6994 = CARTESIAN_POINT ( 'NONE',  ( -91.22235272016261831, -271.3586151295104969, -218.9791671278488536 ) ) ;
#6995 = CARTESIAN_POINT ( 'NONE',  ( -7.082400480927849351, -293.7728859642442671, -203.3863595717635349 ) ) ;
#6996 = CARTESIAN_POINT ( 'NONE',  ( -54.42813229853332757, -285.7662352645559736, -345.3683826091709648 ) ) ;
#6997 = CARTESIAN_POINT ( 'NONE',  ( -33.48937704710156282, -293.4844005883448403, -346.5834846776421045 ) ) ;
#6998 = CARTESIAN_POINT ( 'NONE',  ( -37.24675459869111904, -290.6510736777672719, -344.1610597383615868 ) ) ;
#6999 = CARTESIAN_POINT ( 'NONE',  ( 27.20361063925697565, -291.2593712531426036, -230.1633094889005520 ) ) ;
#7000 = CARTESIAN_POINT ( 'NONE',  ( -78.48896982528417254, -291.0429839221006887, -331.4329218863165920 ) ) ;
#7001 = DIRECTION ( 'NONE',  ( 0.3428573139466625785, 0.000000000000000000, -0.9393874931428881636 ) ) ;
#7002 = CARTESIAN_POINT ( 'NONE',  ( -109.5769074143431254, -291.2012001682414279, -282.0448711806879487 ) ) ;
#7003 = ADVANCED_FACE ( 'NONE', ( #25107 ), #30972, .T. ) ;
#7004 = CARTESIAN_POINT ( 'NONE',  ( 193.9402003287077605, 214.5000000000000568, 16.58062614384823874 ) ) ;
#7005 = CARTESIAN_POINT ( 'NONE',  ( -102.8840994262729680, -292.2785564555401265, -230.6078038479448082 ) ) ;
#7007 = CARTESIAN_POINT ( 'NONE',  ( -85.92902774838911739, -291.3568475447674473, -215.8112333626125974 ) ) ;
#7006 = CARTESIAN_POINT ( 'NONE',  ( 37.88539608355938526, -279.6388598177692302, -275.5728101149813938 ) ) ;
#7008 = CARTESIAN_POINT ( 'NONE',  ( -91.04645891207493946, -279.6480491895856062, -215.1366148102190152 ) ) ;
#7009 = CARTESIAN_POINT ( 'NONE',  ( 36.15678312443506570, -280.9313019580994819, -247.4762485029094137 ) ) ;
#7010 = CARTESIAN_POINT ( 'NONE',  ( 31.81558776187212700, -285.1714003761456979, -241.2046241034049103 ) ) ;
#7011 = DIRECTION ( 'NONE',  ( -0.000000000000000000, -0.000000000000000000, -1.000000000000000000 ) ) ;
#7012 = CARTESIAN_POINT ( 'NONE',  ( 23.58522155720736180, -280.2730732385106194, -312.7730938278062922 ) ) ;
#7013 = CARTESIAN_POINT ( 'NONE',  ( -111.5057150680691507, -282.6997599146849325, -258.8525272093920648 ) ) ;
#7014 = CARTESIAN_POINT ( 'NONE',  ( 215.9306832106271088, -134.2391364535880882, 9.184850993605173582E-16 ) ) ;
#7015 = CARTESIAN_POINT ( 'NONE',  ( -112.3113342385274649, -277.2123964157004821, -256.0694552594962943 ) ) ;
#7016 = CARTESIAN_POINT ( 'NONE',  ( -111.1975124960409147, -283.2125681013214376, -291.0205344732594313 ) ) ;
#7017 = CARTESIAN_POINT ( 'NONE',  ( -96.41779914497033133, -273.9589860196180666, -227.1188957257437835 ) ) ;
#7018 = CARTESIAN_POINT ( 'NONE',  ( 9.339199855150262408, -285.8906705383787994, 74.50000000000001421 ) ) ;
#7019 = CARTESIAN_POINT ( 'NONE',  ( -98.97880242879470813, -292.7101435435285453, -229.6812116764525911 ) ) ;
#7020 = CARTESIAN_POINT ( 'NONE',  ( 13.55834334993410728, -276.1734498998011986, -213.3010256518856522 ) ) ;
#7021 = CARTESIAN_POINT ( 'NONE',  ( -9.984379220265084953, -276.3515637505444147, -338.0774528972052622 ) ) ;
#7022 = CARTESIAN_POINT ( 'NONE',  ( 18.58859047265045561, -296.2481679979908904, -320.3485107564493433 ) ) ;
#7023 = CARTESIAN_POINT ( 'NONE',  ( -60.02525093786476873, -289.5049175206884797, -343.9441087287246432 ) ) ;
#7024 = CARTESIAN_POINT ( 'NONE',  ( 37.37463990632037536, -279.4841628664315749, -258.7612681658479801 ) ) ;
#7025 = CARTESIAN_POINT ( 'NONE',  ( 15.43971002028817097, -292.6066879537513046, -214.2243466889837862 ) ) ;
#7026 = EDGE_CURVE ( 'NONE', #41724, #52563, #74841, .T. ) ;
#7027 = CARTESIAN_POINT ( 'NONE',  ( -20.00487668688056075, -291.3390828561145440, -199.1550204795333912 ) ) ;
#7028 = CARTESIAN_POINT ( 'NONE',  ( -37.70552466142714110, -293.0565156061199446, -345.3729781758001991 ) ) ;
#7029 = ORIENTED_EDGE ( 'NONE', *, *, #73031, .F. ) ;
#7030 = DIRECTION ( 'NONE',  ( -0.000000000000000000, -1.000000000000000000, -0.000000000000000000 ) ) ;
#7031 = CARTESIAN_POINT ( 'NONE',  ( -32.14665728274690792, -291.6270648105657983, -197.4718791760972181 ) ) ;
#7032 = CARTESIAN_POINT ( 'NONE',  ( 208.4306832106270804, -124.2391364535881024, 6.500000000000033751 ) ) ;
#7033 = CARTESIAN_POINT ( 'NONE',  ( -21.33282851196157992, -271.7666405000204009, -200.3683826091710216 ) ) ;
#7034 = CARTESIAN_POINT ( 'NONE',  ( -93.52545843255403213, -294.8955179977752437, -322.6892331384437398 ) ) ;
#7035 = CARTESIAN_POINT ( 'NONE',  ( -111.3933866198906202, -285.6245445313695086, -289.6391917190264280 ) ) ;
#7036 = CARTESIAN_POINT ( 'NONE',  ( -5.796726697909574177, -286.3120962107630021, -204.5148596655744768 ) ) ;
#7037 = CARTESIAN_POINT ( 'NONE',  ( 33.91752932821798083, -277.3179731855609589, -289.1448868062686870 ) ) ;
#7038 = CARTESIAN_POINT ( 'NONE',  ( -9.908448962836978069, -292.7122189930585137, -339.7820336625546815 ) ) ;
#7039 = CARTESIAN_POINT ( 'NONE',  ( 13.06113443965657872, -296.0969690239382999, -324.6303517046920319 ) ) ;
#7040 = CARTESIAN_POINT ( 'NONE',  ( 35.77521956815993320, -274.2557155123517987, -263.3982587461104004 ) ) ;
#7041 = VERTEX_POINT ( 'NONE', #40215 ) ;
#7042 = DIRECTION ( 'NONE',  ( 0.000000000000000000, 0.000000000000000000, -1.000000000000000000 ) ) ;
#7043 = CARTESIAN_POINT ( 'NONE',  ( -103.0997286745691923, -295.6961550887062344, -310.3814374858926612 ) ) ;
#7044 = CARTESIAN_POINT ( 'NONE',  ( 6.716206674132316756, -290.3683259345561396, -330.4271649894664620 ) ) ;
#7045 = CARTESIAN_POINT ( 'NONE',  ( 201.2384769459594338, 294.9663689418843546, -54.00000000002624745 ) ) ;
#7046 = CARTESIAN_POINT ( 'NONE',  ( -30.53256907643855911, -299.2151910733154523, -193.6690121210707218 ) ) ;
#7047 = EDGE_CURVE ( 'NONE', #58642, #50388, #26025, .T. ) ;
#7048 = CARTESIAN_POINT ( 'NONE',  ( 34.09385243788444342, -287.9991247326987036, -254.8416302928420123 ) ) ;
#7049 = VERTEX_POINT ( 'NONE', #75296 ) ;
#7050 = CARTESIAN_POINT ( 'NONE',  ( -86.64440001091345778, -278.4452443927756917, -211.4525367236306295 ) ) ;
#7051 = CARTESIAN_POINT ( 'NONE',  ( 30.81583674611254864, -294.6635482439505722, -305.9681812358531943 ) ) ;
#7052 = CARTESIAN_POINT ( 'NONE',  ( -41.71335259280697727, -287.2462313559519202, -346.0127037148496925 ) ) ;
#7053 = CARTESIAN_POINT ( 'NONE',  ( -44.78935280849671585, -295.4771217365113785, -347.0322411531286662 ) ) ;
#7054 = CARTESIAN_POINT ( 'NONE',  ( 34.23637452811453841, -293.6949321124462813, -255.9158171768883392 ) ) ;
#7055 = CARTESIAN_POINT ( 'NONE',  ( 160.5350683151633291, 215.0000000000000568, 20.22542485937379908 ) ) ;
#7056 = DIRECTION ( 'NONE',  ( 0.9167375550253613614, -2.772018683170089088E-15, -0.3994899938748440738 ) ) ;
#7057 = CARTESIAN_POINT ( 'NONE',  ( 37.87016018917535831, -288.9087604193013021, -257.4047721936249218 ) ) ;
#7058 = CARTESIAN_POINT ( 'NONE',  ( -119.3990491898856732, -288.0523547857347353, -270.3284710469131937 ) ) ;
#7059 = CARTESIAN_POINT ( 'NONE',  ( -62.00707101680345090, -279.0884357435809875, -197.4699962417320478 ) ) ;
#7060 = CARTESIAN_POINT ( 'NONE',  ( -67.26996307630848548, -285.4456307076307553, -338.9631276106981659 ) ) ;
#7061 = CARTESIAN_POINT ( 'NONE',  ( -111.7815602526666083, -283.3441965717582320, -253.1183362963863033 ) ) ;
#7062 = CARTESIAN_POINT ( 'NONE',  ( 29.51046450980167180, -286.0669579147032096, -303.1040909402275361 ) ) ;
#7063 = CARTESIAN_POINT ( 'NONE',  ( 26.61900499379244422, -277.9545973047178222, -311.0706754686984823 ) ) ;
#7064 = CARTESIAN_POINT ( 'NONE',  ( -105.4374961801752875, -273.2392712410683657, -243.8578155381300689 ) ) ;
#7065 = ORIENTED_EDGE ( 'NONE', *, *, #76588, .F. ) ;
#7067 = CARTESIAN_POINT ( 'NONE',  ( -110.3823259807169421, -277.8613037742954361, -273.3543842450285979 ) ) ;
#7066 = CARTESIAN_POINT ( 'NONE',  ( -108.7647745755792386, -278.3530741203107937, -285.4523219261550366 ) ) ;
#7068 = CARTESIAN_POINT ( 'NONE',  ( -18.63872135734161972, -275.3671001505113054, -195.9309720107538908 ) ) ;
#7069 = CARTESIAN_POINT ( 'NONE',  ( -107.0513787054035078, -277.7565670481077973, -238.4754808204128267 ) ) ;
#7070 = CARTESIAN_POINT ( 'NONE',  ( 82.92988855738929033, 83.04799596232011538, -299.9466387458070926 ) ) ;
#7071 = CARTESIAN_POINT ( 'NONE',  ( -112.5622897402321740, -298.1467245017408345, -256.9272357375537013 ) ) ;
#7072 = CARTESIAN_POINT ( 'NONE',  ( -85.28047601435908120, -280.1948066931273047, -330.5268031993605859 ) ) ;
#7073 = DIRECTION ( 'NONE',  ( -1.000000000000000000, 0.000000000000000000, 0.000000000000000000 ) ) ;
#7074 = CARTESIAN_POINT ( 'NONE',  ( -17.09966293588080077, -287.3992388870588570, -199.8489406817098200 ) ) ;
#7075 = CARTESIAN_POINT ( 'NONE',  ( -1.468010098879991121, -288.2813009617613602, -203.3756540442568053 ) ) ;
#7076 = CARTESIAN_POINT ( 'NONE',  ( 35.22440129381648433, -287.0171186732558795, -279.1959124088705266 ) ) ;
#7077 = CARTESIAN_POINT ( 'NONE',  ( -93.87025930839122623, -284.7716884051310444, -218.0906233700659129 ) ) ;
#7078 = CARTESIAN_POINT ( 'NONE',  ( -3.967757526706389815, -278.8997267243151441, -204.5244298472641731 ) ) ;
#7079 = CARTESIAN_POINT ( 'NONE',  ( -38.67038157317211500, -287.8957673897451741, -196.1251131226379982 ) ) ;
#7080 = CARTESIAN_POINT ( 'NONE',  ( -1.613138504112029858, -279.0147793021048983, -205.9082077491523251 ) ) ;
#7081 = CARTESIAN_POINT ( 'NONE',  ( -74.24652513619511751, -278.8690315782885705, -333.9164275119168792 ) ) ;
#7082 = CARTESIAN_POINT ( 'NONE',  ( 30.22934423381503777, -275.6707975466348444, -242.4408504447100370 ) ) ;
#7083 = CARTESIAN_POINT ( 'NONE',  ( -7.090927681746135747, -287.4589500239404174, -340.7521223062466902 ) ) ;
#7084 =( BOUNDED_CURVE ( )  B_SPLINE_CURVE ( 3, ( #71359, #70439, #28272, #6489 ),
 .UNSPECIFIED., .F., .F. ) 
 B_SPLINE_CURVE_WITH_KNOTS ( ( 4, 4 ),
 ( 0.000000000000000000, 1.570796326794896558 ),
 .UNSPECIFIED. ) 
 CURVE ( )  GEOMETRIC_REPRESENTATION_ITEM ( )  RATIONAL_B_SPLINE_CURVE ( ( 1.000000000000000000, 0.8047378541243649375, 0.8047378541243649375, 1.000000000000000000 ) ) 
 REPRESENTATION_ITEM ( '' )  );
#7085 = CARTESIAN_POINT ( 'NONE',  ( -44.39418969742571619, -283.9419087698825592, -346.9285527955577209 ) ) ;
#7086 = CARTESIAN_POINT ( 'NONE',  ( 22.47937911706563341, -282.6939875261372208, -318.7654306573768395 ) ) ;
#7087 = VERTEX_POINT ( 'NONE', #9954 ) ;
#7088 = ORIENTED_EDGE ( 'NONE', *, *, #81991, .T. ) ;
#7089 = PLANE ( 'NONE',  #45867 ) ;
#7090 = CARTESIAN_POINT ( 'NONE',  ( -48.66068399534277233, -291.0550835054452818, -345.3287199756893529 ) ) ;
#7091 =( BOUNDED_SURFACE ( )  B_SPLINE_SURFACE ( 3, 2, ( 
 ( #90402, #31287, #54439 ),
 ( #60635, #47316, #54908 ),
 ( #11363, #89472, #69131 ),
 ( #24633, #82396, #10415 ),
 ( #83787, #4259, #47796 ),
 ( #39279, #76698, #11824 ) ),
 .UNSPECIFIED., .F., .F., .F. ) 
 B_SPLINE_SURFACE_WITH_KNOTS ( ( 4, 2, 4 ),
 ( 3, 3 ),
 ( 4.712388980384689674, 5.132923315668655562, 5.553457650952620561 ),
 ( 0.000000000000000000, 1.000000000000000000 ),
 .UNSPECIFIED. ) 
 GEOMETRIC_REPRESENTATION_ITEM ( )  RATIONAL_B_SPLINE_SURFACE ( (
 ( 1.000000000000000000, 0.7071067811865479058, 1.000000000000000000),
 ( 1.000000000000000000, 0.7192895461630171017, 1.000000000000000000),
 ( 1.000000000000000000, 0.7311219824197653372, 1.000000000000000000),
 ( 1.000000000000000000, 0.7523130761988451320, 1.000000000000000000),
 ( 1.000000000000000000, 0.7616706333094609427, 1.000000000000000000),
 ( 1.000000000000000000, 0.7691239371209227516, 1.000000000000000000) ) ) 
 REPRESENTATION_ITEM ( '' )  SURFACE ( )  );
#7092 = CARTESIAN_POINT ( 'NONE',  ( -107.9057941361184305, -289.6154458966639140, -240.7975101447190127 ) ) ;
#7093 = CARTESIAN_POINT ( 'NONE',  ( -36.47075185634856354, -297.2604951136947875, -197.1997627011453176 ) ) ;
#7094 = CARTESIAN_POINT ( 'NONE',  ( 38.25551345877767773, -293.0780124340349175, -284.5167600108106285 ) ) ;
#7095 = CARTESIAN_POINT ( 'NONE',  ( -111.0305539148856582, -289.0214017338840335, -271.1738775337034326 ) ) ;
#7096 = CARTESIAN_POINT ( 'NONE',  ( 34.42319523733951314, -292.0276786710265924, -288.4656425308204462 ) ) ;
#7097 = CARTESIAN_POINT ( 'NONE',  ( -15.72010934889362233, -289.9713115370194032, -340.5543608675225187 ) ) ;
#7098 = CARTESIAN_POINT ( 'NONE',  ( -4.829096099716510437, -294.9805209788416391, -202.7746430608542312 ) ) ;
#7099 = CARTESIAN_POINT ( 'NONE',  ( -10.26108672732496530, -290.6988631617981014, -340.3013855461616117 ) ) ;
#7100 = CARTESIAN_POINT ( 'NONE',  ( -76.19917938228769572, -289.5343665863347269, -205.9572992815773773 ) ) ;
#7101 = CARTESIAN_POINT ( 'NONE',  ( -108.6286968551104337, -292.8552351796186599, -246.8927161664981327 ) ) ;
#7102 = CARTESIAN_POINT ( 'NONE',  ( -110.6257822262946604, -285.4860212947751847, -270.9230285595351120 ) ) ;
#7103 = CARTESIAN_POINT ( 'NONE',  ( -2.918675998981901554, -294.5060914746232470, -203.5254114378927852 ) ) ;
#7104 = CARTESIAN_POINT ( 'NONE',  ( 198.7962788613944554, 70.38469146215045669, -8.627472241147954080 ) ) ;
#7105 = CARTESIAN_POINT ( 'NONE',  ( 164.5772123382336360, 215.0000000000000568, 23.16839473634451352 ) ) ;
#7106 = CARTESIAN_POINT ( 'NONE',  ( -68.19420706344247662, -275.6289073083696621, -201.5972668998938104 ) ) ;
#7107 = CARTESIAN_POINT ( 'NONE',  ( 35.72668069995849294, -280.7978797817931991, -274.0507588419442300 ) ) ;
#7108 = CARTESIAN_POINT ( 'NONE',  ( -20.97594140799273177, -280.8421099611669547, -343.6071924052199620 ) ) ;
#7109 = CARTESIAN_POINT ( 'NONE',  ( -77.00765004450929041, -294.7661319212363082, -336.2316186421426210 ) ) ;
#7110 = CARTESIAN_POINT ( 'NONE',  ( -0.01613631748763947812, -272.7959631242477485, -206.4340675467720700 ) ) ;
#7111 = CARTESIAN_POINT ( 'NONE',  ( -108.9979491427641136, -276.8939667428833218, -250.1472208473432488 ) ) ;
#7112 = CARTESIAN_POINT ( 'NONE',  ( -67.03383423311878175, -298.9697968567703583, -203.1192200960973082 ) ) ;
#7113 = CARTESIAN_POINT ( 'NONE',  ( -32.70012028322606312, -272.6842735674172786, -194.0784015736182084 ) ) ;
#7114 = CIRCLE ( 'NONE', #19188, 161.1282194813176716 ) ;
#7115 = CARTESIAN_POINT ( 'NONE',  ( 8.610147779436365667, -295.8339420924097567, -327.9053352202059273 ) ) ;
#7116 = DIRECTION ( 'NONE',  ( -1.000000000000000000, 2.528396334038674078E-14, 0.000000000000000000 ) ) ;
#7117 = CARTESIAN_POINT ( 'NONE',  ( 12.47228721121615003, -295.1398145241167299, -324.0138475432739824 ) ) ;
#7118 = PLANE ( 'NONE',  #76246 ) ;
#7120 = CARTESIAN_POINT ( 'NONE',  ( -107.4593678003782458, -296.8207896077103101, -250.0507098084899269 ) ) ;
#7119 = CARTESIAN_POINT ( 'NONE',  ( 31.35486059148992410, -285.9765145794269188, -301.3319001026927140 ) ) ;
#7121 = CARTESIAN_POINT ( 'NONE',  ( -112.2191501870833292, -284.3269071426077517, -288.3715275247583918 ) ) ;
#7122 = CARTESIAN_POINT ( 'NONE',  ( 30.11507937956458747, -286.7372079471851407, -233.1651006806397390 ) ) ;
#7123 = CARTESIAN_POINT ( 'NONE',  ( -64.97632907408589631, -297.3912319468601595, -340.4801984846240543 ) ) ;
#7124 = CARTESIAN_POINT ( 'NONE',  ( 26.42306370415410299, -291.0241908030313311, -231.0953168893059910 ) ) ;
#7125 = CARTESIAN_POINT ( 'NONE',  ( -106.0266406357846165, -278.1946908041737743, -235.7964893375063866 ) ) ;
#7126 = CARTESIAN_POINT ( 'NONE',  ( -69.85430415644619018, -283.1237833571632336, -202.7746430608542312 ) ) ;
#7127 = DIRECTION ( 'NONE',  ( 0.000000000000000000, -1.000000000000000000, 0.000000000000000000 ) ) ;
#7128 = CARTESIAN_POINT ( 'NONE',  ( 29.17625045938557449, -285.9304288892359978, -239.3370506595847758 ) ) ;
#7129 = LINE ( 'NONE', #6192, #45722 ) ;
#7130 = DIRECTION ( 'NONE',  ( 0.000000000000000000, 0.7071067811865453523, 0.7071067811865496822 ) ) ;
#7131 = CARTESIAN_POINT ( 'NONE',  ( -109.6646779096919886, -297.9597641865797755, -285.1150300007515170 ) ) ;
#7132 = CARTESIAN_POINT ( 'NONE',  ( 31.48278798456017569, -282.5469119903268620, -237.0461362092005118 ) ) ;
#7134 = CARTESIAN_POINT ( 'NONE',  ( 35.13978117179284055, -281.6721582681755649, -279.4582361891523874 ) ) ;
#7133 = CARTESIAN_POINT ( 'NONE',  ( -108.7942807330012158, -294.2642801701703661, -294.2971896536288909 ) ) ;
#7135 = CARTESIAN_POINT ( 'NONE',  ( -79.47519025333227205, -295.7711118491522484, -334.8108582020454946 ) ) ;
#7136 = CARTESIAN_POINT ( 'NONE',  ( -94.16042442217737118, -298.7314441443371607, -223.4123825899095266 ) ) ;
#7137 = CARTESIAN_POINT ( 'NONE',  ( -112.2334996200438582, -280.5006066897011578, -274.3884017989200856 ) ) ;
#7138 = CARTESIAN_POINT ( 'NONE',  ( -109.3757370138529836, -295.4362798152733944, -283.6407202090755391 ) ) ;
#7139 = ORIENTED_EDGE ( 'NONE', *, *, #24867, .T. ) ;
#7140 = DIRECTION ( 'NONE',  ( -0.9531768234071980039, 0.3024135303179465994, 0.000000000000000000 ) ) ;
#7141 = CARTESIAN_POINT ( 'NONE',  ( -26.47904842952123872, -284.8932935787976817, -344.2637591965354318 ) ) ;
#7142 = CARTESIAN_POINT ( 'NONE',  ( 35.77081079830085031, -285.2666405000204577, -287.0812184334320705 ) ) ;
#7143 = CARTESIAN_POINT ( 'NONE',  ( 31.11108745493102390, -274.2988428703843056, -235.4558935581463004 ) ) ;
#7144 = CARTESIAN_POINT ( 'NONE',  ( -38.89545100498257568, -291.8654403850818539, -197.3776550423595779 ) ) ;
#7145 = CARTESIAN_POINT ( 'NONE',  ( 36.12186651307747809, -283.1563243192268260, -276.7925661319537198 ) ) ;
#7146 = CARTESIAN_POINT ( 'NONE',  ( 10.19473273332901186, -277.9837410051501365, -326.8122292550070256 ) ) ;
#7147 = CARTESIAN_POINT ( 'NONE',  ( -55.49168060666269042, -284.8820700471522400, -344.3680002438806582 ) ) ;
#7148 = CARTESIAN_POINT ( 'NONE',  ( 16.10452853613887214, -281.0680866321639542, -320.7398045616621971 ) ) ;
#7149 = CARTESIAN_POINT ( 'NONE',  ( -97.22357734207655255, -281.1699180712141128, -225.1827164605083169 ) ) ;
#7150 = CARTESIAN_POINT ( 'NONE',  ( -95.08788239902190753, -273.4085100799261454, -219.4260766293930374 ) ) ;
#7151 = CARTESIAN_POINT ( 'NONE',  ( 37.63539790685170061, -275.1655360718625616, -252.7699371046462886 ) ) ;
#7152 = CARTESIAN_POINT ( 'NONE',  ( 34.69567685560257075, -295.2294235094186092, -251.6013067403051195 ) ) ;
#7153 = CARTESIAN_POINT ( 'NONE',  ( 195.4781563537916043, 39.36132622696000283, 15.00000000000000000 ) ) ;
#7154 = EDGE_CURVE ( 'NONE', #70970, #15223, #24946, .T. ) ;
#7155 = FACE_OUTER_BOUND ( 'NONE', #28486, .T. ) ;
#7156 = CARTESIAN_POINT ( 'NONE',  ( -47.48995389434674763, -293.3194205098727707, -345.4431958992966543 ) ) ;
#7157 = CARTESIAN_POINT ( 'NONE',  ( 15.49562604702088642, -274.3318680299166772, -219.8279375278595467 ) ) ;
#7158 = CARTESIAN_POINT ( 'NONE',  ( -27.95376492520366796, -293.6892561052258657, -194.5809552263336002 ) ) ;
#7160 = CARTESIAN_POINT ( 'NONE',  ( -4.786900107585593034, -293.6765280656847494, -201.0199778420223424 ) ) ;
#7159 = CARTESIAN_POINT ( 'NONE',  ( -106.6379572354042296, -280.6233781216988064, -303.7686719486574702 ) ) ;
#7161 = CARTESIAN_POINT ( 'NONE',  ( -4.977042499739167347, -290.6251904383378246, -337.8337596082291725 ) ) ;
#7162 = CARTESIAN_POINT ( 'NONE',  ( -106.1172279546642869, -276.9385234058473202, -240.8661150861728117 ) ) ;
#7163 = CARTESIAN_POINT ( 'NONE',  ( -3.185369503373105537, -278.5174666350597477, -336.5023250997544437 ) ) ;
#7164 = CARTESIAN_POINT ( 'NONE',  ( 18.13778201089037623, -292.3284865894563040, -320.0123873693774499 ) ) ;
#7165 = CARTESIAN_POINT ( 'NONE',  ( 16.33108357850814585, -282.6644319118433941, -216.8129312042700008 ) ) ;
#7166 = CARTESIAN_POINT ( 'NONE',  ( -73.69702880635465192, -284.4777452976173890, -206.6871859149378565 ) ) ;
#7167 = ORIENTED_EDGE ( 'NONE', *, *, #41597, .T. ) ;
#7168 = CARTESIAN_POINT ( 'NONE',  ( -94.30417223308484154, -283.5732186842045053, -316.0686921172443817 ) ) ;
#7169 = CARTESIAN_POINT ( 'NONE',  ( 16.99435925800993985, -281.8838132093619038, -216.1656443505091545 ) ) ;
#7170 = CARTESIAN_POINT ( 'NONE',  ( -99.47545859961090287, -282.7489472816398575, -315.2538570478912447 ) ) ;
#7171 = CARTESIAN_POINT ( 'NONE',  ( -112.8320463949825694, -279.3177547684487081, -284.3626656460864410 ) ) ;
#7172 =( LENGTH_UNIT ( ) NAMED_UNIT ( * ) SI_UNIT ( .MILLI., .METRE. ) );
#7173 = CARTESIAN_POINT ( 'NONE',  ( -20.26228589976311056, -278.3568506892581809, -344.7860498234580291 ) ) ;
#7174 = CARTESIAN_POINT ( 'NONE',  ( -92.08974858914540107, -299.6948066931273047, -226.7417163044926838 ) ) ;
#7175 = ORIENTED_EDGE ( 'NONE', *, *, #89946, .F. ) ;
#7176 = CARTESIAN_POINT ( 'NONE',  ( -103.6668617920756787, -275.0136687236110333, -235.5933444221973332 ) ) ;
#7177 = CARTESIAN_POINT ( 'NONE',  ( -111.1215563367978376, -276.4260836690726819, -281.6915911053656032 ) ) ;
#7178 = CARTESIAN_POINT ( 'NONE',  ( -67.94153441006896799, -293.4161115380208571, -200.7939066959690706 ) ) ;
#7179 = CARTESIAN_POINT ( 'NONE',  ( 8.285327411402866105, -293.7575907092848979, -327.5406761253193508 ) ) ;
#7180 = CARTESIAN_POINT ( 'NONE',  ( -36.09413305362367197, -288.5445924022116628, -347.3025643310726309 ) ) ;
#7181 = CARTESIAN_POINT ( 'NONE',  ( 196.3496553477289979, 275.5000000000000568, -12.41762739670151028 ) ) ;
#7183 = CARTESIAN_POINT ( 'NONE',  ( -97.21202249259219741, -283.5491817299816830, -227.1888439198559695 ) ) ;
#7182 = CARTESIAN_POINT ( 'NONE',  ( 17.12867446459954124, -292.8689781493878854, -324.0235240223855158 ) ) ;
#7184 = CARTESIAN_POINT ( 'NONE',  ( -94.40425624975429741, -293.0751925236358488, -222.8572660269012999 ) ) ;
#7185 = CARTESIAN_POINT ( 'NONE',  ( -22.29957616885191030, -284.7280169917509625, -198.1669211354738707 ) ) ;
#7186 = CARTESIAN_POINT ( 'NONE',  ( 19.74563475441328819, -283.5179939348461176, -316.6657268384461759 ) ) ;
#7187 = CARTESIAN_POINT ( 'NONE',  ( -78.00158110369487474, -290.5252851946589203, -335.5352868487544242 ) ) ;
#7188 = CARTESIAN_POINT ( 'NONE',  ( -49.15803158862561162, -280.3898404293923932, -198.2614456371258314 ) ) ;
#7189 = CARTESIAN_POINT ( 'NONE',  ( 23.70320921492129784, -292.9668288521231716, -316.6377618017401119 ) ) ;
#7190 = CARTESIAN_POINT ( 'NONE',  ( -71.82482149821827022, -290.2991598961791624, -339.0275083183964853 ) ) ;
#7191 = CARTESIAN_POINT ( 'NONE',  ( -107.6725686388678440, -290.6446161164286082, -301.6866124972198122 ) ) ;
#7192 = CARTESIAN_POINT ( 'NONE',  ( -108.6653612838779139, -284.9247893153510063, -254.7484792412284094 ) ) ;
#7193 = ORIENTED_EDGE ( 'NONE', *, *, #48633, .T. ) ;
#7194 = CARTESIAN_POINT ( 'NONE',  ( 196.2721731643909493, 25.96757666558882249, 13.11199317982073964 ) ) ;
#7195 = CARTESIAN_POINT ( 'NONE',  ( -16.81832942683857723, -296.6503936476161698, -343.3476081012445889 ) ) ;
#7196 = CARTESIAN_POINT ( 'NONE',  ( -66.75045764000135762, -294.1142937034701959, -341.0040009966007233 ) ) ;
#7197 = CARTESIAN_POINT ( 'NONE',  ( -104.6536365235664761, -277.9972614360513603, -241.5078397260232066 ) ) ;
#7198 = CARTESIAN_POINT ( 'NONE',  ( -90.11608427741597893, -272.8379850721510138, -214.3027349565816166 ) ) ;
#7199 = CARTESIAN_POINT ( 'NONE',  ( -94.49241062865399954, -294.3795063799121863, -316.9051871735808277 ) ) ;
#7200 = CARTESIAN_POINT ( 'NONE',  ( 16.34818114384753329, -278.0365607360602667, -321.3058985051895320 ) ) ;
#7201 = CARTESIAN_POINT ( 'NONE',  ( -110.3400107804503847, -270.8703530188331001, -256.5917214264551944 ) ) ;
#7202 = CARTESIAN_POINT ( 'NONE',  ( 31.19371124689212493, -294.4082951049963413, -244.0927360039654275 ) ) ;
#7203 = CARTESIAN_POINT ( 'NONE',  ( -18.12629589025442556, -295.8782519814267289, -341.1071024106926757 ) ) ;
#7204 = CARTESIAN_POINT ( 'NONE',  ( -43.53359761804701833, -248.9297984573114206, -457.6993533439309090 ) ) ;
#7205 = CARTESIAN_POINT ( 'NONE',  ( -103.0138546998814775, -294.0651481195229167, -307.0352826579660928 ) ) ;
#7206 = CARTESIAN_POINT ( 'NONE',  ( -3.474620760922319640, -299.1171511841361621, -193.4594115620958235 ) ) ;
#7207 = CARTESIAN_POINT ( 'NONE',  ( -91.66225793563351942, -275.2782973076661506, -218.6289031468443227 ) ) ;
#7208 = CARTESIAN_POINT ( 'NONE',  ( -73.65123802759283933, -290.4880025271413615, -333.9760928769686075 ) ) ;
#7209 = ADVANCED_FACE ( 'NONE', ( #67733 ), #7091, .T. ) ;
#7210 = CARTESIAN_POINT ( 'NONE',  ( -6.752185930356357169, -294.9724303683275934, -336.6662392629854708 ) ) ;
#7211 = ADVANCED_FACE ( 'NONE', ( #21807 ), #80467, .F. ) ;
#7212 = CARTESIAN_POINT ( 'NONE',  ( -104.7165239969798876, -280.9769677934530705, -236.4951618567751268 ) ) ;
#7213 = CARTESIAN_POINT ( 'NONE',  ( -71.00243563160469762, -278.3020554667772899, -201.6570194123836472 ) ) ;
#7214 = CARTESIAN_POINT ( 'NONE',  ( -50.08479655238178196, -282.5591333045410352, -346.2497843848386196 ) ) ;
#7215 = CARTESIAN_POINT ( 'NONE',  ( 18.02198024882880034, -274.1683619831264878, -216.9163685676203386 ) ) ;
#7216 = CARTESIAN_POINT ( 'NONE',  ( -97.92776169824443855, -277.5748366934224123, -224.1254826648542746 ) ) ;
#7217 = CARTESIAN_POINT ( 'NONE',  ( 13.92988305839977414, -278.7687763035351054, -215.3240152272078660 ) ) ;
#7218 = CARTESIAN_POINT ( 'NONE',  ( -37.80895721098180928, -296.7310026960128084, -196.8694507646536067 ) ) ;
#7219 = CARTESIAN_POINT ( 'NONE',  ( 30.20466255269252542, -277.1216036762295403, -237.6473325055321197 ) ) ;
#7220 = DIRECTION ( 'NONE',  ( -1.000000000000000000, 0.000000000000000000, 0.000000000000000000 ) ) ;
#7221 = CARTESIAN_POINT ( 'NONE',  ( 3.276644636312318504, -290.6147296812558807, -206.8283415308592055 ) ) ;
#7222 = CARTESIAN_POINT ( 'NONE',  ( -84.26634997801217253, -291.4270372459754981, -209.2441245203598896 ) ) ;
#7223 = CARTESIAN_POINT ( 'NONE',  ( 35.84391337528088428, -277.3320258065396047, -253.1618620851873800 ) ) ;
#7224 = CARTESIAN_POINT ( 'NONE',  ( -103.7909281743501708, -271.0139915186837811, -235.4708296132491512 ) ) ;
#7225 = CARTESIAN_POINT ( 'NONE',  ( -114.1792412848347169, -283.7541924397377784, -269.9724163247458932 ) ) ;
#7226 = CARTESIAN_POINT ( 'NONE',  ( 210.0121166852535453, 37.89751991204045822, 12.09245862092500445 ) ) ;
#7227 = CARTESIAN_POINT ( 'NONE',  ( -106.1944638811755226, -282.9424797285483351, -240.4950376771912204 ) ) ;
#7228 = CARTESIAN_POINT ( 'NONE',  ( -35.09237171215954731, -55.96374926131388605, -21.49999999999998579 ) ) ;
#7229 = CARTESIAN_POINT ( 'NONE',  ( 21.32035684398580955, -291.7309960939639950, -226.2488342322953372 ) ) ;
#7230 = CARTESIAN_POINT ( 'NONE',  ( -69.28533722039857423, -283.7669347865880809, -203.3361320070691534 ) ) ;
#7231 = DIRECTION ( 'NONE',  ( 0.000000000000000000, 0.000000000000000000, 1.000000000000000000 ) ) ;
#7232 = DIRECTION ( 'NONE',  ( 0.5729786897769378884, 0.000000000000000000, -0.8195702660916291959 ) ) ;
#7233 = CARTESIAN_POINT ( 'NONE',  ( -53.60728416713134692, -293.2605465356435843, -343.6294976467989386 ) ) ;
#7234 = CARTESIAN_POINT ( 'NONE',  ( -111.8523100230623157, -282.8243325068079344, -286.8194523056383787 ) ) ;
#7235 = CARTESIAN_POINT ( 'NONE',  ( -110.2796499548566800, -280.0055263922336053, -281.6081571790532507 ) ) ;
#7236 = CARTESIAN_POINT ( 'NONE',  ( -113.5074147319497513, -285.6544849095171230, -278.5337942202795034 ) ) ;
#7237 = CARTESIAN_POINT ( 'NONE',  ( 4.725366358314717630, -286.6376670810212204, -210.6388719559611218 ) ) ;
#7238 = CARTESIAN_POINT ( 'NONE',  ( -97.35579628699115062, -279.3872387993422990, -312.9703550283261393 ) ) ;
#7239 = CARTESIAN_POINT ( 'NONE',  ( -107.2679349521096981, -279.0686007766782382, -292.0463360408438689 ) ) ;
#7240 = CARTESIAN_POINT ( 'NONE',  ( -77.66408300951567867, -287.4935398090840977, -206.7017727117505217 ) ) ;
#7241 = EDGE_LOOP ( 'NONE', ( #74576, #14622 ) ) ;
#7242 = CARTESIAN_POINT ( 'NONE',  ( -29.05750026640263783, -297.9865096745180608, -193.3613442771316784 ) ) ;
#7243 = CARTESIAN_POINT ( 'NONE',  ( -48.27759395506573981, -291.1717583829959040, -344.2526611745329319 ) ) ;
#7244 = CARTESIAN_POINT ( 'NONE',  ( 197.1656530321902494, 41.90019538913895758, 12.64285714285713169 ) ) ;
#7245 = CARTESIAN_POINT ( 'NONE',  ( -88.47809603358389552, -280.1948066931273615, -334.5364918783848793 ) ) ;
#7246 = EDGE_LOOP ( 'NONE', ( #80302, #26116, #84583, #21763 ) ) ;
#7247 = CARTESIAN_POINT ( 'NONE',  ( 37.56701494694144117, -292.1294505906153631, -284.4002304093277758 ) ) ;
#7248 = CARTESIAN_POINT ( 'NONE',  ( 2.808707373818427389, -288.1218635581265630, -208.5658711673335688 ) ) ;
#7249 = CARTESIAN_POINT ( 'NONE',  ( -24.72539527704555340, -281.9754725635006594, -197.4309948290255363 ) ) ;
#7250 = CARTESIAN_POINT ( 'NONE',  ( 15.87570614894008614, -288.2137928377180174, -215.5294304189747834 ) ) ;
#7251 = CARTESIAN_POINT ( 'NONE',  ( -23.38535074789511370, -290.1926157370633632, -345.6380130623340960 ) ) ;
#7252 = CARTESIAN_POINT ( 'NONE',  ( -64.76353949753462302, -285.4104154463406076, -340.1683051118224057 ) ) ;
#7253 = CARTESIAN_POINT ( 'NONE',  ( -113.2368464688460818, -278.8813791914287776, -257.3639349635557778 ) ) ;
#7254 = ORIENTED_EDGE ( 'NONE', *, *, #66289, .T. ) ;
#7255 = CARTESIAN_POINT ( 'NONE',  ( 21.15598079295905265, -292.2864592625681439, -318.2075177388838370 ) ) ;
#7256 = CARTESIAN_POINT ( 'NONE',  ( 33.56509868952359454, -281.7690813911262353, -300.5176987633950034 ) ) ;
#7257 = CARTESIAN_POINT ( 'NONE',  ( -77.24785468263895893, -275.3712703558093153, -207.7642785429671619 ) ) ;
#7258 = CARTESIAN_POINT ( 'NONE',  ( 10.64812456238590066, -296.9090924074130271, -330.4860931364851808 ) ) ;
#7259 = CARTESIAN_POINT ( 'NONE',  ( 0.7076817878556337371, -272.7920367444243084, -204.5720357498089186 ) ) ;
#7260 = DIRECTION ( 'NONE',  ( 0.000000000000000000, 1.000000000000000000, 0.000000000000000000 ) ) ;
#7261 = CARTESIAN_POINT ( 'NONE',  ( -94.83539817078383294, -278.6951295816203356, -225.2581365094856949 ) ) ;
#7262 = CARTESIAN_POINT ( 'NONE',  ( 36.89660199557103226, -276.5196711305298436, -251.4750591648150930 ) ) ;
#7263 = CARTESIAN_POINT ( 'NONE',  ( -110.8354741793802276, -273.9030467697824065, -267.6355640499449464 ) ) ;
#7264 = CARTESIAN_POINT ( 'NONE',  ( -95.16541780068362755, -282.9259802854631403, -320.8510960763929347 ) ) ;
#7265 = CARTESIAN_POINT ( 'NONE',  ( -80.13461248654070346, -293.2245296477840384, -209.9100366727946323 ) ) ;
#7266 = CARTESIAN_POINT ( 'NONE',  ( -96.32987636094588879, -274.8068644004699195, -222.1034674048001420 ) ) ;
#7267 = CARTESIAN_POINT ( 'NONE',  ( -62.72800018497400032, -298.9339808649056067, -198.0870252002743257 ) ) ;
#7268 = CARTESIAN_POINT ( 'NONE',  ( 36.51944549281796526, -295.3965629740329177, -258.2578604923841112 ) ) ;
#7269 = CARTESIAN_POINT ( 'NONE',  ( -69.82750888952243429, -281.4807601740003520, -337.7896654513637031 ) ) ;
#7270 = CARTESIAN_POINT ( 'NONE',  ( -74.66492877972062558, -291.2360943320602473, -203.0356332492932552 ) ) ;
#7271 = CARTESIAN_POINT ( 'NONE',  ( -40.82706062568297511, -272.0283339704262744, -195.7469068541524280 ) ) ;
#7272 = CARTESIAN_POINT ( 'NONE',  ( -54.80130261255236945, -287.4314623565190914, -196.1883285346809771 ) ) ;
#7273 = CARTESIAN_POINT ( 'NONE',  ( -95.35059346602918140, -290.1009269421457475, -225.5370801424006686 ) ) ;
#7274 = EDGE_LOOP ( 'NONE', ( #29793, #86470, #92033, #65757 ) ) ;
#7275 = CARTESIAN_POINT ( 'NONE',  ( -111.9935966042498308, -288.9214562681422649, -286.6614446004053320 ) ) ;
#7276 = CARTESIAN_POINT ( 'NONE',  ( -73.55913816900171298, -289.2136750876487099, -333.7820373800358880 ) ) ;
#7277 = ORIENTED_EDGE ( 'NONE', *, *, #28588, .T. ) ;
#7278 = CARTESIAN_POINT ( 'NONE',  ( -65.77558574881582842, -286.7685004050736666, -199.1219766837695602 ) ) ;
#7279 = CARTESIAN_POINT ( 'NONE',  ( -94.46692208612743968, -278.2430617321524551, -315.8651140816054976 ) ) ;
#7280 = CARTESIAN_POINT ( 'NONE',  ( 21.08392122010786096, -291.7998335950834417, -220.6626927068153634 ) ) ;
#7281 = CARTESIAN_POINT ( 'NONE',  ( -113.4972347800642041, -285.0653552029529010, -281.3974856930398118 ) ) ;
#7282 = CARTESIAN_POINT ( 'NONE',  ( -113.1153965253515565, -284.7120382297592869, -284.2217233150922198 ) ) ;
#7283 = CARTESIAN_POINT ( 'NONE',  ( 13.34672591524345009, -281.1181539504035527, -217.7285905783485020 ) ) ;
#7284 = CARTESIAN_POINT ( 'NONE',  ( 194.3816077206797672, 279.0927965383107221, -125.9308262313876554 ) ) ;
#7285 = CARTESIAN_POINT ( 'NONE',  ( 83.43343483694488327, 83.57203687522600433, -301.5415206557701140 ) ) ;
#7286 = CARTESIAN_POINT ( 'NONE',  ( -22.83531149767027557, -108.3062553589070376, -359.1681096793552115 ) ) ;
#7287 = CARTESIAN_POINT ( 'NONE',  ( -91.23458003854895537, -272.4580642510734947, -220.8636993540350488 ) ) ;
#7288 = CARTESIAN_POINT ( 'NONE',  ( 17.52601395158817610, -273.7800237770179592, -221.6673662946266461 ) ) ;
#7289 = CARTESIAN_POINT ( 'NONE',  ( -2.001332507245941361, -294.1044473235040755, -338.7027986749537263 ) ) ;
#7290 = CARTESIAN_POINT ( 'NONE',  ( -97.10692441846769896, -247.3327781681390434, -331.7524723150551722 ) ) ;
#7291 = CARTESIAN_POINT ( 'NONE',  ( -5.305412031941359352, -273.1498058260812627, -200.8846865860590754 ) ) ;
#7292 = CARTESIAN_POINT ( 'NONE',  ( -39.22298429835362299, -299.8887444167067429, -196.1371374432262087 ) ) ;
#7293 = CARTESIAN_POINT ( 'NONE',  ( 36.14846292514583581, -288.8760192597929404, -271.0239987986652750 ) ) ;
#7294 = ORIENTED_EDGE ( 'NONE', *, *, #45328, .T. ) ;
#7295 = CARTESIAN_POINT ( 'NONE',  ( 22.11203495250237694, -295.1474022478846564, -318.9417577962707355 ) ) ;
#7296 = CARTESIAN_POINT ( 'NONE',  ( -22.45341665638626338, -286.7401623425297430, -198.7806865494790145 ) ) ;
#7297 = CARTESIAN_POINT ( 'NONE',  ( -35.51730267654592410, -272.9948440623159627, -193.6788546413600045 ) ) ;
#7298 = CARTESIAN_POINT ( 'NONE',  ( 38.69058855379418560, -294.2113767598840468, -258.9026380222433659 ) ) ;
#7299 = CARTESIAN_POINT ( 'NONE',  ( 8.874196962227477670, -294.9294089835647128, -331.8722369708993938 ) ) ;
#7300 = CARTESIAN_POINT ( 'NONE',  ( -110.2457897413033692, -290.7798233996524004, -265.7377335876513484 ) ) ;
#7301 = ORIENTED_EDGE ( 'NONE', *, *, #86873, .T. ) ;
#7302 = CARTESIAN_POINT ( 'NONE',  ( -87.10669878723285819, -275.2859343075214724, -213.4341772667394537 ) ) ;
#7303 = CARTESIAN_POINT ( 'NONE',  ( 32.19907589617695720, -273.9325119451387422, -238.1086016015925679 ) ) ;
#7304 = EDGE_LOOP ( 'NONE', ( #59580, #39641, #11949, #25899 ) ) ;
#7305 = CARTESIAN_POINT ( 'NONE',  ( -108.6017983359425330, -277.6910922696535522, -299.3701735770973755 ) ) ;
#7306 = AXIS2_PLACEMENT_3D ( 'NONE', #49041, #62320, #91160 ) ;
#7307 = CARTESIAN_POINT ( 'NONE',  ( -4.938610846734867721, -272.8859581490106052, -204.0411808673291034 ) ) ;
#7308 = CARTESIAN_POINT ( 'NONE',  ( -81.26716764257807313, -274.5190730836419561, -211.6051682571911954 ) ) ;
#7309 = CARTESIAN_POINT ( 'NONE',  ( 34.94136667986096256, -276.6522269190517136, -282.4392749586534137 ) ) ;
#7310 = CARTESIAN_POINT ( 'NONE',  ( 31.62381642964157891, -276.8972517539813794, -238.3339914456489907 ) ) ;
#7311 = CARTESIAN_POINT ( 'NONE',  ( 0.2051289676536661166, -274.5753082265285911, -335.7551433604197655 ) ) ;
#7312 = CARTESIAN_POINT ( 'NONE',  ( -107.6986632188032473, -296.9416090447183478, -290.2052711020807010 ) ) ;
#7313 = CARTESIAN_POINT ( 'NONE',  ( -0.4783833154159193857, -293.1269915589218726, -334.1096994262956628 ) ) ;
#7314 = DIRECTION ( 'NONE',  ( -1.000000000000000000, -0.000000000000000000, 0.000000000000000000 ) ) ;
#7315 = CARTESIAN_POINT ( 'NONE',  ( -108.5970784161944920, -278.6756281051976885, -299.3817652547846819 ) ) ;
#7316 = EDGE_CURVE ( 'NONE', #66639, #69774, #58267, .T. ) ;
#7317 = CARTESIAN_POINT ( 'NONE',  ( -43.20497315338152333, -277.2949324147015204, -343.1252714782054909 ) ) ;
#7318 = CARTESIAN_POINT ( 'NONE',  ( 38.07360725524704037, -286.0739223711511841, -257.4064627545597546 ) ) ;
#7319 = CARTESIAN_POINT ( 'NONE',  ( -87.36587989630380946, -297.7475330820072941, -326.5344579262251727 ) ) ;
#7320 = CARTESIAN_POINT ( 'NONE',  ( 185.2169494693457921, 214.5000000000000568, 22.91843887563416615 ) ) ;
#7321 = CARTESIAN_POINT ( 'NONE',  ( 35.43606684423092190, -286.6508172190175401, -262.8779127012985555 ) ) ;
#7322 = CARTESIAN_POINT ( 'NONE',  ( -68.48392182479585699, -275.7068954339067091, -337.5177131985232677 ) ) ;
#7323 = CARTESIAN_POINT ( 'NONE',  ( -85.50448027146268259, -276.3079747631875307, -326.0678421554713395 ) ) ;
#7324 = CARTESIAN_POINT ( 'NONE',  ( -6.981474314252575475, -284.6539601972892797, -338.9551571135510244 ) ) ;
#7325 = CARTESIAN_POINT ( 'NONE',  ( 7.836818112054698027, -277.6246654281800943, -328.2707868051127775 ) ) ;
#7326 = CARTESIAN_POINT ( 'NONE',  ( 37.70778159425776721, -273.7843746852797722, -257.0949468214871558 ) ) ;
#7327 = CARTESIAN_POINT ( 'NONE',  ( 23.13199988185597888, -275.6329188942714836, -229.2677022577485104 ) ) ;
#7328 = CARTESIAN_POINT ( 'NONE',  ( -83.46261069444261693, -281.4221282114945097, -210.9412948250862314 ) ) ;
#7329 = DIRECTION ( 'NONE',  ( -0.5000000000000046629, 0.8660254037844359321, 0.000000000000000000 ) ) ;
#7330 = CARTESIAN_POINT ( 'NONE',  ( 35.01367428307751339, -289.7512843928762436, -292.1779677071431820 ) ) ;
#7331 = CARTESIAN_POINT ( 'NONE',  ( 35.48612735234511462, -291.3212389420839941, -252.3888785349612931 ) ) ;
#7332 = LINE ( 'NONE', #78839, #67864 ) ;
#7333 = CARTESIAN_POINT ( 'NONE',  ( -39.16288030708625456, -296.8237485672630100, -196.9741648151990887 ) ) ;
#7334 = CARTESIAN_POINT ( 'NONE',  ( -86.73348826152849256, -289.4967310613776590, -214.8724866495738013 ) ) ;
#7335 = CARTESIAN_POINT ( 'NONE',  ( -102.0362518552990423, -259.7623939308359695, -328.6249738900723969 ) ) ;
#7336 = CARTESIAN_POINT ( 'NONE',  ( 17.06571399127465583, -89.54582641780471874, -21.50000000000000000 ) ) ;
#7337 = CARTESIAN_POINT ( 'NONE',  ( -108.1622392593899349, -288.6682118485084629, -298.7716615952896291 ) ) ;
#7338 = CARTESIAN_POINT ( 'NONE',  ( -46.36266841555873697, -284.1790391573577494, -194.9118227992420032 ) ) ;
#7339 = CARTESIAN_POINT ( 'NONE',  ( -5.763761739604193579, -284.0539317238017247, -336.8445880951425693 ) ) ;
#7340 = CARTESIAN_POINT ( 'NONE',  ( -95.23796663636437643, -284.7263841119616359, -315.1099008191312123 ) ) ;
#7341 = CARTESIAN_POINT ( 'NONE',  ( -111.3152682984157451, -292.7164615455351964, -255.9300100085924328 ) ) ;
#7342 = CARTESIAN_POINT ( 'NONE',  ( -7.702645710841940385, -274.7632777462546301, -199.2603914410591699 ) ) ;
#7343 = CARTESIAN_POINT ( 'NONE',  ( -86.46713220710074665, -287.8076055874947201, -327.8407148384625316 ) ) ;
#7344 = CARTESIAN_POINT ( 'NONE',  ( -80.22618522096833260, -277.6151522787772592, -334.3777930783103329 ) ) ;
#7345 = CARTESIAN_POINT ( 'NONE',  ( 34.33651968054503101, -295.8020994586047436, -291.2416911104346582 ) ) ;
#7346 = CARTESIAN_POINT ( 'NONE',  ( -48.18343439339133027, -279.1637174034430018, -435.8377362501374819 ) ) ;
#7347 = CARTESIAN_POINT ( 'NONE',  ( -54.49178911615187815, -294.3376638359846424, -195.3683826091709363 ) ) ;
#7348 = CARTESIAN_POINT ( 'NONE',  ( -76.40332558018849340, -282.2709157401953917, -332.6742866197554918 ) ) ;
#7349 = CARTESIAN_POINT ( 'NONE',  ( -101.6823991907854463, -277.0691194793241152, -231.7209270219530595 ) ) ;
#7350 = CARTESIAN_POINT ( 'NONE',  ( -29.14603860014715764, -296.5530167252624665, -194.1633003519424676 ) ) ;
#7351 = CARTESIAN_POINT ( 'NONE',  ( 5.449747793456863221, -275.8044679810632260, -329.6923719141394145 ) ) ;
#7352 = CARTESIAN_POINT ( 'NONE',  ( -66.85939642382594172, -293.1782835180126767, -202.8376897577792306 ) ) ;
#7353 = CARTESIAN_POINT ( 'NONE',  ( 35.85612424714413748, -294.4626086341283440, -268.0186931386346600 ) ) ;
#7354 = CARTESIAN_POINT ( 'NONE',  ( -19.54178905977980918, -293.7018708416291588, -195.9981090741242724 ) ) ;
#7355 = CARTESIAN_POINT ( 'NONE',  ( 37.87552115377394557, -295.0442818344714055, -284.4201210769314798 ) ) ;
#7356 = CARTESIAN_POINT ( 'NONE',  ( -75.65986327579751958, -295.4119945539263767, -332.5547311101244645 ) ) ;
#7357 = CARTESIAN_POINT ( 'NONE',  ( -95.64335279893977315, -291.9027365869796427, -317.5407528813690874 ) ) ;
#7358 = CARTESIAN_POINT ( 'NONE',  ( -65.25020913368327058, -283.5736460396396410, -342.1396242093028377 ) ) ;
#7359 = CARTESIAN_POINT ( 'NONE',  ( -57.76549615179668962, -271.9308735383560816, -197.3465018183667610 ) ) ;
#7360 = CARTESIAN_POINT ( 'NONE',  ( 38.97555232233433031, -287.2575177201455290, -260.1299409768067790 ) ) ;
#7361 = CARTESIAN_POINT ( 'NONE',  ( -72.40499749212899872, -279.4983972245187829, -336.2725132946476378 ) ) ;
#7362 = CARTESIAN_POINT ( 'NONE',  ( -94.29749217648718229, -284.2601039909745850, -224.3038033710650723 ) ) ;
#7363 = AXIS2_PLACEMENT_3D ( 'NONE', #2833, #53490, #82366 ) ;
#7364 = CARTESIAN_POINT ( 'NONE',  ( 2.105958780920293094, -286.5242751722619801, -334.2098248602603121 ) ) ;
#7365 = CARTESIAN_POINT ( 'NONE',  ( -47.92246533766702044, -278.0586734568408360, -195.2857899559915325 ) ) ;
#7366 = CARTESIAN_POINT ( 'NONE',  ( 138.4517698930976621, 181.0451598467585939, -241.7086681466011271 ) ) ;
#7367 = CARTESIAN_POINT ( 'NONE',  ( -106.2338551108908717, -283.7345201533813110, -294.8399708850815273 ) ) ;
#7368 = CARTESIAN_POINT ( 'NONE',  ( 20.75488144871690466, -282.0795940391786871, -220.4132701381974186 ) ) ;
#7369 = CARTESIAN_POINT ( 'NONE',  ( -85.02792095063060174, -288.7504108396719289, -330.5857798872023636 ) ) ;
#7370 = CARTESIAN_POINT ( 'NONE',  ( -106.6995022861665063, -280.5613197533720040, -238.6755537127948230 ) ) ;
#7371 = CARTESIAN_POINT ( 'NONE',  ( -113.5542500113674294, -279.9590010970384810, -263.0776403166724435 ) ) ;
#7372 = CARTESIAN_POINT ( 'NONE',  ( -6.767482008568397767, -280.2983314334559282, -204.0585803137349785 ) ) ;
#7373 = CARTESIAN_POINT ( 'NONE',  ( -33.99153014528766903, -276.0743977868228285, -195.7915319182122289 ) ) ;
#7374 = CARTESIAN_POINT ( 'NONE',  ( 38.81654538241593144, -293.6941541911065201, -281.7154845770832026 ) ) ;
#7375 = CARTESIAN_POINT ( 'NONE',  ( -0.1943082086063979974, -286.5759808413779410, -335.1656272501982698 ) ) ;
#7376 = CARTESIAN_POINT ( 'NONE',  ( -61.45494562234897984, -293.3443279717359360, -198.0214343523827552 ) ) ;
#7377 = CARTESIAN_POINT ( 'NONE',  ( -109.1904178402274397, -295.2803978796736146, -284.9834920409502956 ) ) ;
#7378 = CARTESIAN_POINT ( 'NONE',  ( -6.637615445609045040, -284.5660254688896771, -338.1878864456475640 ) ) ;
#7379 = CARTESIAN_POINT ( 'NONE',  ( -107.9911126678050550, -295.9746349995157289, -288.8699270060547519 ) ) ;
#7380 = ADVANCED_FACE ( 'NONE', ( #489 ), #76310, .T. ) ;
#7381 = CARTESIAN_POINT ( 'NONE',  ( -112.2604165958704954, -291.4259945195586852, -286.7525314066531905 ) ) ;
#7382 = CARTESIAN_POINT ( 'NONE',  ( 34.33226316028071068, -282.3938069907771364, -284.8024528873946224 ) ) ;
#7383 = CARTESIAN_POINT ( 'NONE',  ( -111.5876062096892696, -271.8581163455078809, -250.6548316373763896 ) ) ;
#7384 = CARTESIAN_POINT ( 'NONE',  ( -96.30754671483715867, -290.5381907459117201, -319.7408516773059546 ) ) ;
#7385 = CARTESIAN_POINT ( 'NONE',  ( -71.20821920759951240, -281.6340472725624977, -338.1354816430568917 ) ) ;
#7386 = CARTESIAN_POINT ( 'NONE',  ( -113.1117357226714972, -290.7145117023840157, -284.0240004984877373 ) ) ;
#7387 = CARTESIAN_POINT ( 'NONE',  ( 4.734086419195035589, -286.9708946122954671, -210.6191333610420884 ) ) ;
#7388 = CARTESIAN_POINT ( 'NONE',  ( 221.8344101925596306, -0.9999999999999997780, -22.50000000000000000 ) ) ;
#7389 = CARTESIAN_POINT ( 'NONE',  ( -100.4238177162668393, -246.2515245119496115, -332.5401888311394032 ) ) ;
#7390 = CARTESIAN_POINT ( 'NONE',  ( -111.1600279138487934, -270.9246594666713008, -270.3403961019906774 ) ) ;
#7391 = CARTESIAN_POINT ( 'NONE',  ( -102.2945453730720970, -278.2075512087710081, -236.5799876957273966 ) ) ;
#7392 = CARTESIAN_POINT ( 'NONE',  ( -39.69744901629324119, -278.9422343666826123, -197.0772920184110149 ) ) ;
#7393 = CARTESIAN_POINT ( 'NONE',  ( 36.56675697029471905, -274.9467652579022001, -248.6507670799472578 ) ) ;
#7394 = CARTESIAN_POINT ( 'NONE',  ( 181.3594537276159713, 251.3396015629845692, -165.1358875192213134 ) ) ;
#7395 = CARTESIAN_POINT ( 'NONE',  ( -39.55188914467541395, -278.5996758072924990, -193.9693651698094072 ) ) ;
#7396 = CARTESIAN_POINT ( 'NONE',  ( -91.96183380851151412, -281.8567976975985516, -321.2383014722413463 ) ) ;
#7397 = CARTESIAN_POINT ( 'NONE',  ( -84.60389220254988629, -299.1712945176369089, -210.8610405742479372 ) ) ;
#7398 = PRODUCT_DEFINITION_SHAPE ( 'NONE', 'NONE',  #93722 ) ;
#7399 = CARTESIAN_POINT ( 'NONE',  ( -105.7704830759360135, -291.3874835410810533, -244.6149867537183411 ) ) ;
#7400 = CARTESIAN_POINT ( 'NONE',  ( 22.35253574138633326, -286.8322729737879513, -313.2311737645909488 ) ) ;
#7401 = CARTESIAN_POINT ( 'NONE',  ( -38.36438704365086494, -274.6910569366528421, -193.4698512576767087 ) ) ;
#7402 = CARTESIAN_POINT ( 'NONE',  ( -93.77838007488207950, -273.2082476322101456, -224.0392921260430796 ) ) ;
#7403 = ORIENTED_EDGE ( 'NONE', *, *, #70232, .T. ) ;
#7404 = DIRECTION ( 'NONE',  ( -1.000000000000000000, 0.000000000000000000, 0.000000000000000000 ) ) ;
#7405 = CARTESIAN_POINT ( 'NONE',  ( 196.1604930303647052, 24.75642484911453067, 13.67253731732742494 ) ) ;
#7406 = CARTESIAN_POINT ( 'NONE',  ( -107.1909812488175646, -280.8455200767294286, -241.5445928190535767 ) ) ;
#7407 = ADVANCED_FACE ( 'NONE', ( #36001 ), #88022, .F. ) ;
#7408 = CARTESIAN_POINT ( 'NONE',  ( -5.436336988437288298, -281.5617868795328604, -204.3590431843336717 ) ) ;
#7409 = CARTESIAN_POINT ( 'NONE',  ( 22.92967474464701993, -282.6865176902531971, -224.0653042454112835 ) ) ;
#7410 = CARTESIAN_POINT ( 'NONE',  ( -109.1573545956944713, -283.7995885584018652, -256.0111973508373353 ) ) ;
#7411 = CARTESIAN_POINT ( 'NONE',  ( -71.53128412206604025, -281.4560224062233260, -204.4534078623156859 ) ) ;
#7412 = CARTESIAN_POINT ( 'NONE',  ( -93.42900568078000845, -271.7057625159539498, -222.5407886399894721 ) ) ;
#7413 = CARTESIAN_POINT ( 'NONE',  ( 209.7199135963037406, 27.99931114053373804, 12.09245862092541657 ) ) ;
#7414 = CARTESIAN_POINT ( 'NONE',  ( 30.40553344078523068, -276.8258151589418503, -306.7291272325348928 ) ) ;
#7415 = LINE ( 'NONE', #23845, #64300 ) ;
#7416 = CARTESIAN_POINT ( 'NONE',  ( 35.65144221479864228, -277.7742414586551831, -287.6502583164456723 ) ) ;
#7417 = CARTESIAN_POINT ( 'NONE',  ( -59.51152465938343994, -275.9084964070916612, -343.4850208587597535 ) ) ;
#7418 = EDGE_LOOP ( 'NONE', ( #20822, #91078, #16702, #11786 ) ) ;
#7419 = FACE_OUTER_BOUND ( 'NONE', #2512, .T. ) ;
#7420 = CARTESIAN_POINT ( 'NONE',  ( -111.5133652729610390, -286.3583831934366231, -283.9501325348069258 ) ) ;
#7421 = CARTESIAN_POINT ( 'NONE',  ( 35.45708788859575833, -292.6470921678688342, -262.5949118206045227 ) ) ;
#7422 = EDGE_CURVE ( 'NONE', #37641, #11917, #68744, .T. ) ;
#7423 = CARTESIAN_POINT ( 'NONE',  ( 39.47629699141587878, -286.8440308249012105, -265.8326795976899461 ) ) ;
#7424 = CARTESIAN_POINT ( 'NONE',  ( -108.3706339366843707, -282.5199907487194082, -291.2118141177707002 ) ) ;
#7426 = CARTESIAN_POINT ( 'NONE',  ( 14.15300692814562922, -284.8615251816797240, -216.5348918934058418 ) ) ;
#7425 = CARTESIAN_POINT ( 'NONE',  ( -70.49652195816902633, -282.0728041394958154, -336.0724916501939674 ) ) ;
#7427 = VECTOR ( 'NONE', #91516, 1000.000000000000000 ) ;
#7428 = CARTESIAN_POINT ( 'NONE',  ( -2.225260288398726694, -283.7815079380501970, -334.8267560375776384 ) ) ;
#7429 = CARTESIAN_POINT ( 'NONE',  ( 12.65082333798339675, -272.7485685126762291, -214.3833030623713398 ) ) ;
#7430 = CARTESIAN_POINT ( 'NONE',  ( -97.42632129310945288, -282.3193136978437110, -317.2255897905537267 ) ) ;
#7431 = CARTESIAN_POINT ( 'NONE',  ( -47.33909678044954461, -297.1793749872496733, -344.6918162647891677 ) ) ;
#7432 = CARTESIAN_POINT ( 'NONE',  ( -97.85283191370568545, -283.1599014465709843, -225.6836823457252592 ) ) ;
#7433 = CARTESIAN_POINT ( 'NONE',  ( -96.27524051113842063, -278.8857423555685386, -313.8590963136624055 ) ) ;
#7434 = CARTESIAN_POINT ( 'NONE',  ( 36.04082636296087827, -289.7616302308222771, -286.6998084993668385 ) ) ;
#7435 = CARTESIAN_POINT ( 'NONE',  ( 196.5940483389518647, 25.86285152137379839, 12.79436563626940249 ) ) ;
#7436 = FACE_BOUND ( 'NONE', #16047, .T. ) ;
#7437 = CARTESIAN_POINT ( 'NONE',  ( 34.13241908337529651, -295.7889322477259952, -295.0321057524276966 ) ) ;
#7438 = CARTESIAN_POINT ( 'NONE',  ( -54.43381538617030913, -275.2714312219372346, -343.4411264895401246 ) ) ;
#7439 = CARTESIAN_POINT ( 'NONE',  ( -113.0112184758847320, -289.9166622764174690, -257.0088592312889659 ) ) ;
#7440 = CARTESIAN_POINT ( 'NONE',  ( -12.76078324710743672, -293.1272320691778077, -340.0010074388002863 ) ) ;
#7441 = CARTESIAN_POINT ( 'NONE',  ( -48.70047374889004033, -275.8844992550568804, -343.0229221647573468 ) ) ;
#7442 = CARTESIAN_POINT ( 'NONE',  ( -68.54548304247643387, -295.7773204443063264, -202.9885613389541277 ) ) ;
#7443 = CARTESIAN_POINT ( 'NONE',  ( -65.53150343221980734, -292.9908656688523934, -202.4757313526060045 ) ) ;
#7444 = CARTESIAN_POINT ( 'NONE',  ( -114.2704648735229114, -281.0519495502701943, -270.3937649182068981 ) ) ;
#7445 = CARTESIAN_POINT ( 'NONE',  ( 22.61477395183548467, -292.6692338763337489, -317.5830181715749632 ) ) ;
#7446 = CARTESIAN_POINT ( 'NONE',  ( -98.76533831848146860, -291.5902516473811943, -311.2934915457029774 ) ) ;
#7447 = CARTESIAN_POINT ( 'NONE',  ( -74.16790956180355465, -289.8094647211008805, -203.8945526027512472 ) ) ;
#7448 = CARTESIAN_POINT ( 'NONE',  ( 27.55861952962299100, -289.4477770440237805, -305.1585738415649871 ) ) ;
#7449 = LINE ( 'NONE', #78043, #39566 ) ;
#7450 = CARTESIAN_POINT ( 'NONE',  ( -109.7813925020787593, -291.2188711344051057, -280.7023806571189652 ) ) ;
#7451 = CARTESIAN_POINT ( 'NONE',  ( 161.2244399300530233, -11.64849832608277325, 10.00000000000000000 ) ) ;
#7452 = CARTESIAN_POINT ( 'NONE',  ( -40.30793926865678856, -290.2937017117659479, -346.9196100134480503 ) ) ;
#7453 = CARTESIAN_POINT ( 'NONE',  ( -64.13344471534428237, -277.7246182546919613, -199.8745057071383826 ) ) ;
#7454 = CARTESIAN_POINT ( 'NONE',  ( -35.34083299532585443, -280.4098703869225915, -193.3951366930848792 ) ) ;
#7455 = CARTESIAN_POINT ( 'NONE',  ( 39.25662076447748206, -281.3209443646743466, -278.5205064152426644 ) ) ;
#7456 = CARTESIAN_POINT ( 'NONE',  ( 37.44411412497085223, -285.6330496409593138, -276.6743678429252782 ) ) ;
#7457 = CARTESIAN_POINT ( 'NONE',  ( 197.4027394742815886, 40.84896208771627357, 12.00000000000000533 ) ) ;
#7458 = CARTESIAN_POINT ( 'NONE',  ( 22.79893944653491644, -280.2907011003915159, -313.9026273621292944 ) ) ;
#7459 = CARTESIAN_POINT ( 'NONE',  ( -26.87436509219875802, -284.1849662811917483, -196.0430288327169137 ) ) ;
#7460 = CARTESIAN_POINT ( 'NONE',  ( -30.24964759220584298, -125.8449128503669527, -361.7634443971322753 ) ) ;
#7461 = CARTESIAN_POINT ( 'NONE',  ( -108.9487845264195585, -277.3700243759020054, -243.8432954897286891 ) ) ;
#7462 = CARTESIAN_POINT ( 'NONE',  ( -95.57280689031875909, -284.1493092877096842, -220.3752646503569110 ) ) ;
#7463 = CARTESIAN_POINT ( 'NONE',  ( -47.31662083503962890, -298.8636883046322055, -197.7569371551957147 ) ) ;
#7464 = CARTESIAN_POINT ( 'NONE',  ( -60.52944703691477457, -293.3466080621436163, -200.2448844830101393 ) ) ;
#7465 = CARTESIAN_POINT ( 'NONE',  ( -105.0949417310843330, -274.4379548514282305, -234.9181851586274377 ) ) ;
#7466 = CARTESIAN_POINT ( 'NONE',  ( 19.19526936679832119, -275.8732280863191022, -316.5940060058034078 ) ) ;
#7467 = CARTESIAN_POINT ( 'NONE',  ( -83.57316182170224295, -297.6859669656770961, -329.4836663018785430 ) ) ;
#7468 = CARTESIAN_POINT ( 'NONE',  ( -85.16301476901415413, -289.8581645878473978, -330.7791399507503911 ) ) ;
#7469 = CARTESIAN_POINT ( 'NONE',  ( 19.98977024346277531, -278.9548693950283678, -221.1233832260824670 ) ) ;
#7470 = CARTESIAN_POINT ( 'NONE',  ( -68.32681738763457702, -291.4896017467254978, -199.8561667211738211 ) ) ;
#7471 = CARTESIAN_POINT ( 'NONE',  ( -65.40607646833963429, -290.7348041068386806, -202.7029073236534202 ) ) ;
#7472 = CARTESIAN_POINT ( 'NONE',  ( -14.41819649820433646, -292.7547783979167093, -341.7719969028601668 ) ) ;
#7473 = ORIENTED_EDGE ( 'NONE', *, *, #55430, .F. ) ;
#7474 = CARTESIAN_POINT ( 'NONE',  ( 152.6878565075764413, 20.88255170682893080, 8.268021619243398845 ) ) ;
#7475 = CARTESIAN_POINT ( 'NONE',  ( -107.4525815674616354, -290.3320298012379794, -249.7630531818940653 ) ) ;
#7476 = LINE ( 'NONE', #27885, #65620 ) ;
#7477 = CARTESIAN_POINT ( 'NONE',  ( -83.14512187467356341, -286.3836548251858858, -208.6923339555095254 ) ) ;
#7478 = CARTESIAN_POINT ( 'NONE',  ( 26.47324843497312585, -301.4082689599840705, -200.3320873922942553 ) ) ;
#7479 = CARTESIAN_POINT ( 'NONE',  ( -47.61199230273555116, -294.2384363786133008, -346.4356952810940129 ) ) ;
#7480 = CARTESIAN_POINT ( 'NONE',  ( -113.6612436882926005, -285.9435643748756775, -264.3040664952717975 ) ) ;
#7481 = CARTESIAN_POINT ( 'NONE',  ( -109.9941950075484414, -284.4859016005613626, -262.7479411179006092 ) ) ;
#7482 = CARTESIAN_POINT ( 'NONE',  ( 28.47188256612149004, -276.6265065085495394, -237.2057250053155428 ) ) ;
#7483 = CARTESIAN_POINT ( 'NONE',  ( 2.425238653974422842, -292.5369014915720527, -333.5922310729378069 ) ) ;
#7484 = CARTESIAN_POINT ( 'NONE',  ( 6.683448190523597177, -296.2047645162321601, -329.9208869976035317 ) ) ;
#7485 = CARTESIAN_POINT ( 'NONE',  ( -16.28153566092877469, -275.5688269709810925, -340.7251504719338868 ) ) ;
#7486 = ORIENTED_EDGE ( 'NONE', *, *, #38083, .T. ) ;
#7487 = CARTESIAN_POINT ( 'NONE',  ( 195.9399694403358012, 40.74223533523908714, 13.37580287366501075 ) ) ;
#7488 = CARTESIAN_POINT ( 'NONE',  ( -64.26276884511517551, -295.0607372581387722, -342.4790793419596184 ) ) ;
#7489 = CARTESIAN_POINT ( 'NONE',  ( 18.92982692873014017, -290.1539974459580549, -319.1705488075295989 ) ) ;
#7490 = CARTESIAN_POINT ( 'NONE',  ( -40.51493896710162090, -296.0120873939782769, -195.4251063308001903 ) ) ;
#7491 = CARTESIAN_POINT ( 'NONE',  ( -73.14859241946263069, -298.6688428153473751, -202.4839277906755797 ) ) ;
#7492 = CARTESIAN_POINT ( 'NONE',  ( -9.462182177909394198, -287.0777806097381699, -202.7707827629659221 ) ) ;
#7493 = ORIENTED_EDGE ( 'NONE', *, *, #10209, .F. ) ;
#7494 = CARTESIAN_POINT ( 'NONE',  ( 10.68516722602901048, -279.7558737880664239, -210.4077516066589624 ) ) ;
#7495 = CARTESIAN_POINT ( 'NONE',  ( 35.39271337446832177, -294.5203958933500985, -295.4846725797062277 ) ) ;
#7496 = CARTESIAN_POINT ( 'NONE',  ( -7.429742796862990772, -286.8037157253946816, -339.9853298483084814 ) ) ;
#7497 = CARTESIAN_POINT ( 'NONE',  ( -37.68462341544178429, -295.3895794750191612, -347.3522851773561229 ) ) ;
#7498 = CARTESIAN_POINT ( 'NONE',  ( -57.66489531546407932, -292.1158247085380708, -200.1722482218223433 ) ) ;
#7499 = FACE_OUTER_BOUND ( 'NONE', #65338, .T. ) ;
#7500 = DIRECTION ( 'NONE',  ( 0.000000000000000000, 0.000000000000000000, 1.000000000000000000 ) ) ;
#7501 = CARTESIAN_POINT ( 'NONE',  ( 65.57626950315574277, 46.04035155596911011, -315.5245225721080828 ) ) ;
#7502 = CARTESIAN_POINT ( 'NONE',  ( 37.43278685889510626, -289.2642766528747984, -285.5757113255085642 ) ) ;
#7503 = CARTESIAN_POINT ( 'NONE',  ( -72.08107566293803359, -286.9809262143061233, -342.4248175857292154 ) ) ;
#7504 = ORIENTED_EDGE ( 'NONE', *, *, #55943, .T. ) ;
#7505 = CARTESIAN_POINT ( 'NONE',  ( -59.26513456127775470, -279.1241844158719232, -196.6544303010856254 ) ) ;
#7506 = CARTESIAN_POINT ( 'NONE',  ( -54.07545657469196954, -285.2675302851075685, -343.3529032704057045 ) ) ;
#7507 = CARTESIAN_POINT ( 'NONE',  ( -113.7367640406030347, -283.1677138658753279, -267.1211478547521097 ) ) ;
#7508 = CARTESIAN_POINT ( 'NONE',  ( 2.053330970347486240, -286.6001331627439299, -333.5223855580690611 ) ) ;
#7509 = CARTESIAN_POINT ( 'NONE',  ( 34.89226831338478263, -277.7045605732045033, -293.2206736133009031 ) ) ;
#7510 = CARTESIAN_POINT ( 'NONE',  ( -75.24792998976515435, -298.0247872125918889, -207.8436233722052577 ) ) ;
#7511 = EDGE_LOOP ( 'NONE', ( #17720, #57229, #12802, #9857, #45994, #67486, #38928 ) ) ;
#7512 = CARTESIAN_POINT ( 'NONE',  ( 24.83559786442586059, -292.7757425721266031, -309.6386536368795532 ) ) ;
#7513 = CARTESIAN_POINT ( 'NONE',  ( 15.08576560626180729, -281.4199230255133557, -214.0329021909632274 ) ) ;
#7515 = CARTESIAN_POINT ( 'NONE',  ( -68.55930357958888521, -278.9792883320132546, -204.2600294641966627 ) ) ;
#7514 = CARTESIAN_POINT ( 'NONE',  ( -94.79085638998031982, -279.1873969923022401, -225.3010778704303902 ) ) ;
#7516 = CARTESIAN_POINT ( 'NONE',  ( -27.05166235598578339, -275.2595806962778511, -194.3104845988935381 ) ) ;
#7517 = CARTESIAN_POINT ( 'NONE',  ( -80.06543920429247407, -276.5356547595656025, -334.1131574249279765 ) ) ;
#7518 = CARTESIAN_POINT ( 'NONE',  ( -49.33571708643257381, -154.2190595633487646, -362.6006225449885960 ) ) ;
#7519 = CARTESIAN_POINT ( 'NONE',  ( -101.1263169161629207, -297.4188209467308752, -312.5296757055573948 ) ) ;
#7520 = EDGE_CURVE ( 'NONE', #26188, #92859, #17383, .T. ) ;
#7521 = CYLINDRICAL_SURFACE ( 'NONE', #5010, 24.00000000000001066 ) ;
#7522 = DIRECTION ( 'NONE',  ( -0.000000000000000000, -0.000000000000000000, -1.000000000000000000 ) ) ;
#7523 = CARTESIAN_POINT ( 'NONE',  ( -96.83369361257679486, -286.2285485655050934, -227.5036289521088122 ) ) ;
#7524 = CARTESIAN_POINT ( 'NONE',  ( -65.52266070490216521, -287.4488603876047819, -199.7793967597515916 ) ) ;
#7525 = CARTESIAN_POINT ( 'NONE',  ( -42.67962717982778287, -288.4697143638476291, -343.3185769933509164 ) ) ;
#7526 = CARTESIAN_POINT ( 'NONE',  ( -55.69358219213990679, -282.7899312403828276, -345.0788222283591153 ) ) ;
#7527 = CARTESIAN_POINT ( 'NONE',  ( -106.2540708422838804, -277.3026111395839166, -243.8073779705785853 ) ) ;
#7528 = CARTESIAN_POINT ( 'NONE',  ( -110.7155917216020669, -286.2620343397297233, -281.9657661453371702 ) ) ;
#7529 = CARTESIAN_POINT ( 'NONE',  ( -68.80187949688786375, -278.1107202179663318, -203.7205532436693716 ) ) ;
#7530 = CARTESIAN_POINT ( 'NONE',  ( -101.0016860170209867, -279.3659320730376407, -307.1872531578542862 ) ) ;
#7531 = CARTESIAN_POINT ( 'NONE',  ( 22.51985857732192287, -276.6291946196266167, -312.3357182232217042 ) ) ;
#7532 = CARTESIAN_POINT ( 'NONE',  ( -69.20620378931118921, -288.2569926970262486, -340.0365204887157802 ) ) ;
#7533 = CARTESIAN_POINT ( 'NONE',  ( -76.66644741529918861, -284.3668530391385616, -336.4358553633669544 ) ) ;
#7534 = CARTESIAN_POINT ( 'NONE',  ( -35.89406115168510780, -283.5268304124132897, -347.2990659101908477 ) ) ;
#7535 = ORIENTED_EDGE ( 'NONE', *, *, #79046, .F. ) ;
#7536 = ORIENTED_EDGE ( 'NONE', *, *, #57188, .T. ) ;
#7537 = CARTESIAN_POINT ( 'NONE',  ( 113.5000000000000568, -296.0521521680024080, -400.5374811273811702 ) ) ;
#7538 = CARTESIAN_POINT ( 'NONE',  ( -18.01616243145861418, -290.6660064438785298, -343.6197630057914125 ) ) ;
#7539 = CARTESIAN_POINT ( 'NONE',  ( -99.61981450826766604, -289.8293835929119382, -225.9231303750227369 ) ) ;
#7540 = CARTESIAN_POINT ( 'NONE',  ( -62.09799676616633235, -272.7809153287201411, -201.4369986573041444 ) ) ;
#7541 = EDGE_CURVE ( 'NONE', #54596, #88194, #59177, .T. ) ;
#7542 = CARTESIAN_POINT ( 'NONE',  ( 26.41304628102256302, -292.3324110308308263, -227.2715612061519437 ) ) ;
#7543 = CARTESIAN_POINT ( 'NONE',  ( -26.39079803461989471, -287.3902801190625382, -343.2877873085156466 ) ) ;
#7544 = CARTESIAN_POINT ( 'NONE',  ( -1.935229270645188349, -290.7676620133106553, -205.3516790365035263 ) ) ;
#7545 = CARTESIAN_POINT ( 'NONE',  ( 35.15382308976920456, -288.9087564804833619, -281.9099528905251759 ) ) ;
#7546 = CARTESIAN_POINT ( 'NONE',  ( -106.6662871844225293, -299.4805209788416391, -237.0123917617630980 ) ) ;
#7547 = CARTESIAN_POINT ( 'NONE',  ( 24.22491171025234635, -290.1344191207115841, -313.2820103225519119 ) ) ;
#7548 = CARTESIAN_POINT ( 'NONE',  ( -96.01611929541947177, -289.1967194168807964, -223.3787705850851353 ) ) ;
#7549 = CARTESIAN_POINT ( 'NONE',  ( -111.7136014883612916, -292.6816188629391036, -260.2905747033634611 ) ) ;
#7550 = CARTESIAN_POINT ( 'NONE',  ( -92.72924764313725632, -284.8127112288997296, -318.2929105695568524 ) ) ;
#7551 = CARTESIAN_POINT ( 'NONE',  ( -53.03209716464139234, -293.8517713624847261, -196.7970998129312648 ) ) ;
#7552 = CARTESIAN_POINT ( 'NONE',  ( -113.8396535124608846, -271.2111691839079413, -270.3440440569521002 ) ) ;
#7553 = DIRECTION ( 'NONE',  ( 0.000000000000000000, 0.000000000000000000, -1.000000000000000000 ) ) ;
#7554 = CARTESIAN_POINT ( 'NONE',  ( -99.85839943869147817, -275.0994566530900443, -228.1959883563837082 ) ) ;
#7555 = CARTESIAN_POINT ( 'NONE',  ( -24.04615841946317900, -282.0751310521201844, -342.3043615649121421 ) ) ;
#7556 = CARTESIAN_POINT ( 'NONE',  ( -29.25361161516740438, -280.9496414997782381, -344.9756191661328444 ) ) ;
#7557 = CARTESIAN_POINT ( 'NONE',  ( -112.1148551396041739, -295.9711105592699596, -252.6655221761070038 ) ) ;
#7558 = CARTESIAN_POINT ( 'NONE',  ( 19.79522903882365270, -273.1344383052042417, -223.3149136557231316 ) ) ;
#7559 = CARTESIAN_POINT ( 'NONE',  ( -111.8330156254960031, -276.6286538162293596, -270.6191118479970896 ) ) ;
#7560 = CARTESIAN_POINT ( 'NONE',  ( -93.12961096979383058, -298.5439760193398229, -222.4987571077944608 ) ) ;
#7561 = CARTESIAN_POINT ( 'NONE',  ( 34.21650822272301440, -294.7520833863972598, -253.1376664859379275 ) ) ;
#7562 = CARTESIAN_POINT ( 'NONE',  ( 185.2169494693457921, 275.5000000000000568, 22.91843887563416615 ) ) ;
#7563 = CARTESIAN_POINT ( 'NONE',  ( -67.35211760191585029, -296.2589141621091358, -337.0979870479409328 ) ) ;
#7564 = AXIS2_PLACEMENT_3D ( 'NONE', #75251, #90812, #46350 ) ;
#7565 = CARTESIAN_POINT ( 'NONE',  ( 201.2104617360081704, 60.19600395700751250, 9.000000000000000000 ) ) ;
#7567 = CARTESIAN_POINT ( 'NONE',  ( -93.94254614738427733, -295.8993819926137689, -316.4822198388223455 ) ) ;
#7566 = CARTESIAN_POINT ( 'NONE',  ( 32.50801539778480276, -285.9406706493257957, -298.7740774193781590 ) ) ;
#7568 = CARTESIAN_POINT ( 'NONE',  ( -111.1079767696223257, -284.2745469950962161, -292.4871306347912423 ) ) ;
#7569 = CARTESIAN_POINT ( 'NONE',  ( 37.35733814426770749, -286.9861625435822248, -251.7654740621152882 ) ) ;
#7570 = CARTESIAN_POINT ( 'NONE',  ( -30.61749422227395812, -290.1372171988945752, -195.8304968842527956 ) ) ;
#7571 = CARTESIAN_POINT ( 'NONE',  ( -3.719015550639384493, -279.6817046848572659, -201.2548502630838811 ) ) ;
#7572 = DIRECTION ( 'NONE',  ( -0.000000000000000000, -0.000000000000000000, 1.000000000000000000 ) ) ;
#7573 = CARTESIAN_POINT ( 'NONE',  ( 152.4536156746142410, 275.0000000000000568, -12.49999999999999289 ) ) ;
#7574 = CARTESIAN_POINT ( 'NONE',  ( 35.51653086186653496, -286.4635454192661541, -279.2385433773913519 ) ) ;
#7576 = CARTESIAN_POINT ( 'NONE',  ( 197.3617861379907481, 72.09200933227452879, -11.67137979308930973 ) ) ;
#7575 = CARTESIAN_POINT ( 'NONE',  ( -67.94321647820565602, -288.3649064124025472, -340.6820942808840300 ) ) ;
#7577 = DIRECTION ( 'NONE',  ( 0.000000000000000000, 0.000000000000000000, 1.000000000000000000 ) ) ;
#7578 = CARTESIAN_POINT ( 'NONE',  ( -96.23051212741820848, -297.5339354342016236, -314.8628036802110159 ) ) ;
#7579 = CARTESIAN_POINT ( 'NONE',  ( 18.71545513458323029, -282.2646124421497120, -218.4361563856606381 ) ) ;
#7581 = CARTESIAN_POINT ( 'NONE',  ( 17.61797404352745033, -281.9046644720332324, -318.4394052001749174 ) ) ;
#7580 = CARTESIAN_POINT ( 'NONE',  ( -100.9149473132007984, -295.1141581088621706, -229.9031268782814550 ) ) ;
#7582 = CARTESIAN_POINT ( 'NONE',  ( 21.36902674083426135, -294.3903855568235031, -320.1813001886582697 ) ) ;
#7583 = CARTESIAN_POINT ( 'NONE',  ( -96.14510400025876891, -281.1918237686740554, -223.8083484985326663 ) ) ;
#7584 = CARTESIAN_POINT ( 'NONE',  ( -70.56360710539951242, -296.6616997712624197, -205.0806829565654539 ) ) ;
#7585 = VERTEX_POINT ( 'NONE', #72013 ) ;
#7586 = FACE_OUTER_BOUND ( 'NONE', #37527, .T. ) ;
#7587 = CARTESIAN_POINT ( 'NONE',  ( -43.03373505995562454, -285.1041155077929261, -344.8397983263134847 ) ) ;
#7588 = DIRECTION ( 'NONE',  ( 0.000000000000000000, 1.000000000000000000, -0.000000000000000000 ) ) ;
#7589 = CARTESIAN_POINT ( 'NONE',  ( -4.771743288812454686, -289.9809262143061801, -202.8022627189028810 ) ) ;
#7590 = CARTESIAN_POINT ( 'NONE',  ( -60.81205016550025988, -272.9524639128127887, -197.1393481123545826 ) ) ;
#7591 = CARTESIAN_POINT ( 'NONE',  ( -104.7022500853002782, -290.7644453777260196, -242.0949726629434622 ) ) ;
#7592 = CARTESIAN_POINT ( 'NONE',  ( 23.16499986282335755, -283.6530653494654075, -312.4282905670766013 ) ) ;
#7593 = CARTESIAN_POINT ( 'NONE',  ( -93.53604036198451865, -274.8255083754425527, -222.5019076399073583 ) ) ;
#7594 = CARTESIAN_POINT ( 'NONE',  ( 30.37562633873334406, -283.6073703194417135, -305.3011252756749627 ) ) ;
#7595 = CARTESIAN_POINT ( 'NONE',  ( 35.53212311648148614, -280.4672768188665373, -279.5229458044086641 ) ) ;
#7596 = CARTESIAN_POINT ( 'NONE',  ( -36.18438647925570706, -298.0662671119145557, -193.3611179743799084 ) ) ;
#7597 = CARTESIAN_POINT ( 'NONE',  ( -7.688617024244204678, -274.2633972671821425, -199.2433162556457376 ) ) ;
#7598 = CARTESIAN_POINT ( 'NONE',  ( 27.05030845490103886, -295.9747773250498426, -307.7105949064519450 ) ) ;
#7599 = CARTESIAN_POINT ( 'NONE',  ( 209.2599468862078140, 293.9636489450776367, -44.00000000000000000 ) ) ;
#7600 = EDGE_CURVE ( 'NONE', #26503, #27314, #50680, .T. ) ;
#7601 = CARTESIAN_POINT ( 'NONE',  ( 159.4851178187871312, 17.43233815881133708, 9.000000000000000000 ) ) ;
#7602 = CARTESIAN_POINT ( 'NONE',  ( 31.10381796597688009, -292.1162905066678945, -302.9720514571015997 ) ) ;
#7603 = CARTESIAN_POINT ( 'NONE',  ( -14.03988465984631162, -273.8704231777816744, -201.1150795582342425 ) ) ;
#7604 = CARTESIAN_POINT ( 'NONE',  ( -71.87595467953094897, -293.1241919154217612, -202.3018618893248401 ) ) ;
#7606 = CARTESIAN_POINT ( 'NONE',  ( -53.32154567384359467, -293.0568145391248436, -195.3892560803734852 ) ) ;
#7605 = CARTESIAN_POINT ( 'NONE',  ( 39.58706461736021254, -278.0519495502701943, -270.3284710469133074 ) ) ;
#7607 = CARTESIAN_POINT ( 'NONE',  ( -51.06324492613408950, -291.2279474053913191, -343.9786727187244537 ) ) ;
#7608 = CARTESIAN_POINT ( 'NONE',  ( -68.83150431908634914, -275.4669150004635299, -338.2605629045983164 ) ) ;
#7609 = CARTESIAN_POINT ( 'NONE',  ( -59.60278503193910637, -279.2628775725405035, -341.3946191971621147 ) ) ;
#7610 = CARTESIAN_POINT ( 'NONE',  ( -9.983073168576796164, -292.7719474781958411, -339.5913117521433264 ) ) ;
#7611 = CARTESIAN_POINT ( 'NONE',  ( 23.28124332873744251, -284.0272181631349326, -315.8051958119506821 ) ) ;
#7612 =( BOUNDED_CURVE ( )  B_SPLINE_CURVE ( 3, ( #81407, #52998, #81872, #44499 ),
 .UNSPECIFIED., .F., .F. ) 
 B_SPLINE_CURVE_WITH_KNOTS ( ( 4, 4 ),
 ( 4.712388980384689674, 6.283185307179586232 ),
 .UNSPECIFIED. ) 
 CURVE ( )  GEOMETRIC_REPRESENTATION_ITEM ( )  RATIONAL_B_SPLINE_CURVE ( ( 1.000000000000000000, 0.8047378541243649375, 0.8047378541243649375, 1.000000000000000000 ) ) 
 REPRESENTATION_ITEM ( '' )  );
#7613 = ORIENTED_EDGE ( 'NONE', *, *, #55070, .T. ) ;
#7614 = CARTESIAN_POINT ( 'NONE',  ( -1.245244861868627373, -282.2257596511749398, -333.8365731129762821 ) ) ;
#7615 = CARTESIAN_POINT ( 'NONE',  ( -31.11263331340023441, -281.2086377712009835, -193.8711398463640876 ) ) ;
#7616 =( BOUNDED_CURVE ( )  B_SPLINE_CURVE ( 3, ( #9043, #88590, #34121, #69628 ),
 .UNSPECIFIED., .F., .F. ) 
 B_SPLINE_CURVE_WITH_KNOTS ( ( 4, 4 ),
 ( 1.570796326794896780, 3.141592653589793116 ),
 .UNSPECIFIED. ) 
 CURVE ( )  GEOMETRIC_REPRESENTATION_ITEM ( )  RATIONAL_B_SPLINE_CURVE ( ( 1.000000000000000000, 0.8047378541243650485, 0.8047378541243650485, 1.000000000000000000 ) ) 
 REPRESENTATION_ITEM ( '' )  );
#7617 = CARTESIAN_POINT ( 'NONE',  ( -88.07013429756909773, -282.5380739131590531, -327.8308650439746543 ) ) ;
#7618 = CARTESIAN_POINT ( 'NONE',  ( -114.1492823443344236, -279.4776537539678429, -271.6165480716911134 ) ) ;
#7619 = CARTESIAN_POINT ( 'NONE',  ( 0.000000000000000000, 0.000000000000000000, 0.000000000000000000 ) ) ;
#7620 = CARTESIAN_POINT ( 'NONE',  ( 33.06626714848160731, -276.6931869621677720, -240.8066092224560748 ) ) ;
#7621 = AXIS2_PLACEMENT_3D ( 'NONE', #46135, #2135, #82591 ) ;
#7622 = CARTESIAN_POINT ( 'NONE',  ( -109.1418805571601069, -293.0519495502701943, -270.3937649182068412 ) ) ;
#7623 = ORIENTED_EDGE ( 'NONE', *, *, #24310, .F. ) ;
#7624 = CARTESIAN_POINT ( 'NONE',  ( -47.57004184560806692, -299.9224262388724469, -196.0092313632375465 ) ) ;
#7625 = AXIS2_PLACEMENT_3D ( 'NONE', #91159, #85489, #5960 ) ;
#7626 = CARTESIAN_POINT ( 'NONE',  ( -105.7895014853543501, -276.1791902067704996, -300.2690069769762431 ) ) ;
#7627 = CARTESIAN_POINT ( 'NONE',  ( -110.2660640340680942, -292.5837008754213002, -249.0067000929882965 ) ) ;
#7628 = CARTESIAN_POINT ( 'NONE',  ( -0.7140533417946419714, -293.9007257746479240, -333.6826868982256542 ) ) ;
#7629 = CARTESIAN_POINT ( 'NONE',  ( -69.33743605679320865, -288.9696059422478811, -340.3455227269321313 ) ) ;
#7630 = DIRECTION ( 'NONE',  ( 0.000000000000000000, 0.000000000000000000, 1.000000000000000000 ) ) ;
#7632 = CARTESIAN_POINT ( 'NONE',  ( 2.900117375362208705, -285.0021159433473485, -208.4980713541659441 ) ) ;
#7631 = CARTESIAN_POINT ( 'NONE',  ( 39.06747973268240059, -292.0905341600092697, -267.4770886751508669 ) ) ;
#7633 = CARTESIAN_POINT ( 'NONE',  ( -110.4980700321603138, -292.5799634769675208, -257.4571301719701069 ) ) ;
#7634 = CARTESIAN_POINT ( 'NONE',  ( -25.00689306722070882, -284.6920396171124139, -197.6556299666691245 ) ) ;
#7635 = CARTESIAN_POINT ( 'NONE',  ( -69.20794076186041366, -284.7955577433317558, -336.6002808003874520 ) ) ;
#7636 = CARTESIAN_POINT ( 'NONE',  ( -57.21838058625493062, -290.2436529163837236, -344.5627835646071162 ) ) ;
#7637 = CARTESIAN_POINT ( 'NONE',  ( 18.00704895523404758, -281.3656396487743905, -222.6501507017215147 ) ) ;
#7638 = CARTESIAN_POINT ( 'NONE',  ( 36.70274736358680912, -292.0994463974083715, -250.6781375959988338 ) ) ;
#7639 = CARTESIAN_POINT ( 'NONE',  ( -1.866167020558459066, -289.3971126146655024, -338.5200893048668149 ) ) ;
#7640 = CARTESIAN_POINT ( 'NONE',  ( 5.528237079389339392, -288.9807012610447714, -334.2492654508545229 ) ) ;
#7641 = CARTESIAN_POINT ( 'NONE',  ( -94.95836545548854701, -285.3506306034757358, -225.5153819152156132 ) ) ;
#7642 = ORIENTED_EDGE ( 'NONE', *, *, #18737, .T. ) ;
#7643 = CARTESIAN_POINT ( 'NONE',  ( 195.8183634747502708, 24.45209547744994438, 12.33938814790248628 ) ) ;
#7644 = CARTESIAN_POINT ( 'NONE',  ( -6.282051222323046247, -296.5088506631732344, -339.4668608203849658 ) ) ;
#7645 = CARTESIAN_POINT ( 'NONE',  ( -102.7030309332422036, -294.7144204661468621, -310.1253570340539909 ) ) ;
#7646 = CARTESIAN_POINT ( 'NONE',  ( -109.1154549935966287, -277.8031526839623666, -255.7401531204066032 ) ) ;
#7647 = CARTESIAN_POINT ( 'NONE',  ( -31.25867328258182098, -273.6346691520885770, -193.6502351993405284 ) ) ;
#7648 = CARTESIAN_POINT ( 'NONE',  ( -63.83617255819731895, -293.8837330351287846, -339.1811037829581323 ) ) ;
#7649 = CARTESIAN_POINT ( 'NONE',  ( 36.36516036808060903, -277.3998447183226403, -277.0896191435438141 ) ) ;
#7650 = CARTESIAN_POINT ( 'NONE',  ( 96.73425794709139325, -297.9926885423967065, -196.3887082001726014 ) ) ;
#7651 = CARTESIAN_POINT ( 'NONE',  ( 35.68879948544971370, -294.6546769442354616, -262.5444581666731096 ) ) ;
#7652 = CARTESIAN_POINT ( 'NONE',  ( -41.04112375576690397, -296.1794408085536361, -343.5894495695878277 ) ) ;
#7653 = CARTESIAN_POINT ( 'NONE',  ( -43.36971919400434672, -266.0673380770966219, -435.0464150650843180 ) ) ;
#7654 = CARTESIAN_POINT ( 'NONE',  ( -83.09006787485284917, -293.6761491385539102, -330.0683166829167021 ) ) ;
#7655 = CARTESIAN_POINT ( 'NONE',  ( -113.3860173099026980, -273.4976330378809735, -258.9787793034378751 ) ) ;
#7656 = CARTESIAN_POINT ( 'NONE',  ( -110.4910485170179584, -274.7649140722647303, -253.8029331787696776 ) ) ;
#7657 = CARTESIAN_POINT ( 'NONE',  ( -86.87974619603271265, -290.7027659352472710, -324.3686684384343266 ) ) ;
#7658 = CARTESIAN_POINT ( 'NONE',  ( -90.41968730244110475, -296.1626224865080985, -320.5818608107164778 ) ) ;
#7659 = CARTESIAN_POINT ( 'NONE',  ( -111.1768338370665248, -280.3387799664700424, -285.4839951828166136 ) ) ;
#7660 = CARTESIAN_POINT ( 'NONE',  ( -113.5510591164620280, -277.3290768031770881, -263.0443214946834019 ) ) ;
#7661 = VERTEX_POINT ( 'NONE', #44940 ) ;
#7662 = EDGE_CURVE ( 'NONE', #46169, #75426, #44596, .T. ) ;
#7663 = CARTESIAN_POINT ( 'NONE',  ( -55.68591280941213739, -282.6308908247459613, -345.0391110419173515 ) ) ;
#7664 = CARTESIAN_POINT ( 'NONE',  ( 37.49074956737972286, -275.1230969662741472, -288.1214037199364952 ) ) ;
#7665 = CARTESIAN_POINT ( 'NONE',  ( -95.42364132032581381, -281.9866027466409264, -316.9410683459303186 ) ) ;
#7666 = CARTESIAN_POINT ( 'NONE',  ( -109.7827233945500041, -277.2544304177322942, -246.5561374350880897 ) ) ;
#7667 = CARTESIAN_POINT ( 'NONE',  ( -47.83698939556524010, -277.9189514125929463, -195.8782054105980137 ) ) ;
#7668 = ADVANCED_FACE ( 'NONE', ( #79099 ), #15616, .T. ) ;
#7669 = CARTESIAN_POINT ( 'NONE',  ( -35.78579231260732740, -296.7568535785565587, -196.8683204030683953 ) ) ;
#7670 = CARTESIAN_POINT ( 'NONE',  ( 21.35259629559766026, -276.9103621467494918, -223.6506560989280104 ) ) ;
#7671 = DIRECTION ( 'NONE',  ( 0.000000000000000000, 0.000000000000000000, 1.000000000000000000 ) ) ;
#7672 = CARTESIAN_POINT ( 'NONE',  ( 20.95322147525778789, -290.9170975352554365, -222.6106318888103317 ) ) ;
#7673 = CARTESIAN_POINT ( 'NONE',  ( -114.1878387977255755, -290.6129992367972363, -265.4958357126591864 ) ) ;
#7674 = CARTESIAN_POINT ( 'NONE',  ( 6.152895172813707347, -276.6406331744695990, -208.9927003505397067 ) ) ;
#7675 = CARTESIAN_POINT ( 'NONE',  ( -73.71628697692410981, -295.5678831119499819, -204.9629692364338496 ) ) ;
#7676 = CARTESIAN_POINT ( 'NONE',  ( -112.3696400062573417, -283.5415057738342739, -286.9432486954008823 ) ) ;
#7677 = DIRECTION ( 'NONE',  ( 0.000000000000000000, -1.000000000000000000, 0.000000000000000000 ) ) ;
#7678 = CARTESIAN_POINT ( 'NONE',  ( -94.00535565743152233, -281.8701695921554915, -319.5152833590767045 ) ) ;
#7679 = FACE_OUTER_BOUND ( 'NONE', #18341, .T. ) ;
#7680 = CARTESIAN_POINT ( 'NONE',  ( -19.96334679007314961, -291.0753015629081233, -198.9985110039530696 ) ) ;
#7681 = CARTESIAN_POINT ( 'NONE',  ( -111.4599240142477043, -282.7566209790031735, -265.3587569217504551 ) ) ;
#7682 = CARTESIAN_POINT ( 'NONE',  ( 199.9311642430739653, 275.7557892102190067, 9.103929867429336298 ) ) ;
#7683 = DIRECTION ( 'NONE',  ( -0.000000000000000000, -1.000000000000000000, -0.000000000000000000 ) ) ;
#7684 = CARTESIAN_POINT ( 'NONE',  ( 22.60738330158192610, -290.9360399063122031, -225.2933018846084678 ) ) ;
#7685 = CARTESIAN_POINT ( 'NONE',  ( -112.7988210684069941, -283.1797209547839316, -258.6585086977402170 ) ) ;
#7686 = CARTESIAN_POINT ( 'NONE',  ( -97.52642612285806933, -279.5620666486678374, -313.0941704240725016 ) ) ;
#7687 = CARTESIAN_POINT ( 'NONE',  ( -52.11183345544348811, -287.0723337618114783, -195.1415095971085805 ) ) ;
#7688 = CARTESIAN_POINT ( 'NONE',  ( -95.76594100401823084, -285.1665145707737565, -226.5934577975501156 ) ) ;
#7689 = CARTESIAN_POINT ( 'NONE',  ( -70.70383998876822318, -278.9264471233134941, -335.9533625136695036 ) ) ;
#7690 = CARTESIAN_POINT ( 'NONE',  ( -107.9734917034731154, -279.1036162903054674, -289.4333948835920864 ) ) ;
#7691 = CARTESIAN_POINT ( 'NONE',  ( -110.5667568546550967, -286.3440450655735958, -286.5812203473781778 ) ) ;
#7692 = ORIENTED_EDGE ( 'NONE', *, *, #26979, .F. ) ;
#7693 = CARTESIAN_POINT ( 'NONE',  ( -114.1206415309323319, -296.4666736376944982, -263.8683446475938013 ) ) ;
#7695 = CARTESIAN_POINT ( 'NONE',  ( 35.30760767710200554, -289.7532316566247914, -287.5053555669150001 ) ) ;
#7694 = AXIS2_PLACEMENT_3D ( 'NONE', #31819, #17148, #54054 ) ;
#7696 = CARTESIAN_POINT ( 'NONE',  ( 186.6539576904058890, 276.0000000000000568, 11.60392986742922616 ) ) ;
#7697 = CARTESIAN_POINT ( 'NONE',  ( 36.57525178469696669, -277.6233781216988064, -234.7283546768995564 ) ) ;
#7698 = ORIENTED_EDGE ( 'NONE', *, *, #75701, .F. ) ;
#7699 = CARTESIAN_POINT ( 'NONE',  ( 27.38371178845299880, -291.4193583067088866, -230.0486717460100294 ) ) ;
#7700 = CARTESIAN_POINT ( 'NONE',  ( -10.51544827116342162, -287.9287060366370383, -201.7103035990886895 ) ) ;
#7701 = CARTESIAN_POINT ( 'NONE',  ( -92.98487232703223526, -280.9994775696483771, -221.5380259732319530 ) ) ;
#7702 = CARTESIAN_POINT ( 'NONE',  ( 25.85971434397253077, -288.4065610552826229, -227.3937481752561212 ) ) ;
#7703 = CARTESIAN_POINT ( 'NONE',  ( 39.11240135817894270, -288.9179131124528226, -274.3802218320415705 ) ) ;
#7704 = CARTESIAN_POINT ( 'NONE',  ( -105.9323875721547381, -286.1549196030840108, -300.6978653650383535 ) ) ;
#7705 = CARTESIAN_POINT ( 'NONE',  ( -114.3778511503410584, -278.7391516640313398, -268.7363643332592460 ) ) ;
#7706 = ORIENTED_EDGE ( 'NONE', *, *, #10597, .T. ) ;
#7707 = CARTESIAN_POINT ( 'NONE',  ( 1.016942057057161009, -292.6242209746561684, -335.4604940753806659 ) ) ;
#7708 = CARTESIAN_POINT ( 'NONE',  ( 39.27788474882164138, -281.4875186570441770, -278.5206377531734461 ) ) ;
#7709 = CARTESIAN_POINT ( 'NONE',  ( -43.60964428983029961, -275.8326859452370741, -196.3394306331634596 ) ) ;
#7710 = CARTESIAN_POINT ( 'NONE',  ( 154.0561329571324904, 19.33057573605696788, 12.42898486165470118 ) ) ;
#7711 = CARTESIAN_POINT ( 'NONE',  ( 10.59707575819634329, -289.1948066931273615, -210.1954327657594490 ) ) ;
#7712 = CARTESIAN_POINT ( 'NONE',  ( -93.38257246444671011, -271.4995230722699375, -219.0253014632682778 ) ) ;
#7713 = DIRECTION ( 'NONE',  ( -0.000000000000000000, -1.000000000000000000, -0.000000000000000000 ) ) ;
#7714 = CARTESIAN_POINT ( 'NONE',  ( -99.51680620269306132, -278.5896029714816109, -231.8947761276758683 ) ) ;
#7715 = CARTESIAN_POINT ( 'NONE',  ( 29.59307016885221486, -276.2705804382162569, -232.9996283841600473 ) ) ;
#7716 = CARTESIAN_POINT ( 'NONE',  ( 52.55529011099631731, -300.6244180898165723, -196.7495985462560100 ) ) ;
#7717 = CARTESIAN_POINT ( 'NONE',  ( -96.99714541536069135, -282.9607609712040812, -318.6937652232096525 ) ) ;
#7718 = CARTESIAN_POINT ( 'NONE',  ( -105.6467904554949655, -292.6909565159702993, -241.7252189521745152 ) ) ;
#7719 = CARTESIAN_POINT ( 'NONE',  ( -20.71757579726060428, -299.7768269639770438, -194.0502373830632337 ) ) ;
#7720 = EDGE_CURVE ( 'NONE', #89141, #24992, #59661, .T. ) ;
#7721 = CARTESIAN_POINT ( 'NONE',  ( -70.57075117558406419, -298.8287550621636797, -201.3405494019295645 ) ) ;
#7722 = EDGE_CURVE ( 'NONE', #39851, #49577, #67264, .T. ) ;
#7723 = CARTESIAN_POINT ( 'NONE',  ( -8.501361644253609740, -296.6739735586709799, -339.4276804638399767 ) ) ;
#7724 = CARTESIAN_POINT ( 'NONE',  ( -79.42821710171530469, -281.6218152181293704, -332.2380402828636647 ) ) ;
#7725 = CARTESIAN_POINT ( 'NONE',  ( -114.0917573914470324, -290.1364766763873604, -276.9475576843412341 ) ) ;
#7726 = CARTESIAN_POINT ( 'NONE',  ( -77.42672740886654026, -271.5315811386577707, -207.3925751272192599 ) ) ;
#7727 = CARTESIAN_POINT ( 'NONE',  ( -66.89776550876669603, -287.2713448766969577, -200.1266576683457004 ) ) ;
#7728 = CARTESIAN_POINT ( 'NONE',  ( -95.20299327749819440, -288.8407391502150290, -315.3958114271890736 ) ) ;
#7729 = CARTESIAN_POINT ( 'NONE',  ( -112.5292696805186949, -274.5677371315042024, -270.3867812072841730 ) ) ;
#7730 = ORIENTED_EDGE ( 'NONE', *, *, #76024, .T. ) ;
#7731 = CARTESIAN_POINT ( 'NONE',  ( -87.01526988795936290, -288.3024077196182020, -328.4921727197404380 ) ) ;
#7732 = CARTESIAN_POINT ( 'NONE',  ( 5.853716174388502225, -288.1152533452939792, -329.2989425407670296 ) ) ;
#7733 = ORIENTED_EDGE ( 'NONE', *, *, #35766, .T. ) ;
#7734 = CARTESIAN_POINT ( 'NONE',  ( -103.7795747657820016, -286.1330110146640777, -231.9475000415241368 ) ) ;
#7735 = CARTESIAN_POINT ( 'NONE',  ( 3.149356406875054581, -276.8247395209326100, -331.1275711240854775 ) ) ;
#7736 = CARTESIAN_POINT ( 'NONE',  ( 36.41069530732725212, -292.2073198182430360, -249.2876169929024570 ) ) ;
#7737 = CARTESIAN_POINT ( 'NONE',  ( -50.06845808036404577, -283.8617499965509978, -346.2525266442955285 ) ) ;
#7738 = CARTESIAN_POINT ( 'NONE',  ( 34.66691277832745754, -282.7491219691924584, -244.9553018154132928 ) ) ;
#7739 = CARTESIAN_POINT ( 'NONE',  ( -44.41304438088690176, -283.4724330888014379, -347.0678387719418083 ) ) ;
#7740 = CARTESIAN_POINT ( 'NONE',  ( 35.05317645576933927, -281.7546275580630777, -260.4423215796209661 ) ) ;
#7741 = CARTESIAN_POINT ( 'NONE',  ( 103.4350560888410513, 116.3533902402046039, -283.0411789926872643 ) ) ;
#7742 = CARTESIAN_POINT ( 'NONE',  ( 120.4372898702119130, 149.8266080471096870, -262.8568676293995168 ) ) ;
#7743 = CARTESIAN_POINT ( 'NONE',  ( -31.73477069997540667, -124.2925422290134208, -360.7507360266465071 ) ) ;
#7744 = CARTESIAN_POINT ( 'NONE',  ( -27.25782929498327434, -273.3806123188020933, -197.8468930990040064 ) ) ;
#7745 = CARTESIAN_POINT ( 'NONE',  ( -74.58207618928659599, -295.0412269025912337, -337.7459758234620608 ) ) ;
#7746 = CARTESIAN_POINT ( 'NONE',  ( -109.3415214902221209, -269.1509101800525627, -295.3710750286876987 ) ) ;
#7747 = CARTESIAN_POINT ( 'NONE',  ( -10.50480749357722132, -273.0797659103408819, -198.6592401252945024 ) ) ;
#7748 = CARTESIAN_POINT ( 'NONE',  ( -75.87166970081077011, -299.3926353640264892, -206.8483228001516920 ) ) ;
#7749 = CARTESIAN_POINT ( 'NONE',  ( -5.564139607152227107, -289.9403148723486652, -336.6289844569672596 ) ) ;
#7750 = ORIENTED_EDGE ( 'NONE', *, *, #72944, .F. ) ;
#7751 = CARTESIAN_POINT ( 'NONE',  ( -39.09042823831595115, -296.0148425062287174, -347.1059038886952521 ) ) ;
#7752 = CARTESIAN_POINT ( 'NONE',  ( -89.71133815167226544, -285.7812382303979462, -219.3433495042972936 ) ) ;
#7753 = CARTESIAN_POINT ( 'NONE',  ( -94.84555590992553675, -272.1623599824624762, -219.6186399147071029 ) ) ;
#7754 = CARTESIAN_POINT ( 'NONE',  ( 35.33702570241221252, -294.6717908555838221, -295.4633908134493936 ) ) ;
#7755 = CARTESIAN_POINT ( 'NONE',  ( 30.84147947820869007, -293.5829467071689010, -234.6012339510699292 ) ) ;
#7756 = CARTESIAN_POINT ( 'NONE',  ( -60.26098000395240462, -291.9133906232751769, -200.9993000362906628 ) ) ;
#7757 = ORIENTED_EDGE ( 'NONE', *, *, #60013, .T. ) ;
#7758 = CARTESIAN_POINT ( 'NONE',  ( -92.14490766997379012, -275.1968761404424981, -218.3237460237761809 ) ) ;
#7759 = CARTESIAN_POINT ( 'NONE',  ( 13.71133409898293287, -273.5435252886511535, -213.1798321717830618 ) ) ;
#7760 = ORIENTED_EDGE ( 'NONE', *, *, #8954, .F. ) ;
#7761 = CARTESIAN_POINT ( 'NONE',  ( -100.4186499674009383, -277.4769843675793481, -314.4159168386735814 ) ) ;
#7762 = PRODUCT_DEFINITION_CONTEXT ( 'detailed design', #78364, 'design' ) ;
#7763 = CARTESIAN_POINT ( 'NONE',  ( 35.81620661834794817, -273.8252641290115434, -260.6471540384591776 ) ) ;
#7764 = CARTESIAN_POINT ( 'NONE',  ( -63.42952076588308330, -274.7837419285031615, -201.8373356671743295 ) ) ;
#7765 = CARTESIAN_POINT ( 'NONE',  ( 34.34922166516801667, -276.2958808459353577, -255.3393228957438907 ) ) ;
#7766 = CARTESIAN_POINT ( 'NONE',  ( -85.18777873020214031, -275.1618072837981117, -211.3295436033829446 ) ) ;
#7767 = AXIS2_PLACEMENT_3D ( 'NONE', #76083, #25875, #75155 ) ;
#7768 = CARTESIAN_POINT ( 'NONE',  ( 37.91336121491469413, -273.5110305658723746, -265.5700288548729873 ) ) ;
#7769 = CARTESIAN_POINT ( 'NONE',  ( -47.79942961734017359, -295.8399312599377708, -342.7625107140514729 ) ) ;
#7770 = CARTESIAN_POINT ( 'NONE',  ( -2.883789903580015856, -293.1620033748531000, -335.3844010531342406 ) ) ;
#7771 = FACE_BOUND ( 'NONE', #46629, .T. ) ;
#7772 = CARTESIAN_POINT ( 'NONE',  ( -95.86308428181750685, -279.7189087915049868, -220.3931628794002791 ) ) ;
#7773 = CARTESIAN_POINT ( 'NONE',  ( 17.28414232958849084, -275.0261739179064762, -221.8608397717020466 ) ) ;
#7774 = CARTESIAN_POINT ( 'NONE',  ( -91.54174124195003515, -283.9845055329766410, -216.3643234902861821 ) ) ;
#7775 = CARTESIAN_POINT ( 'NONE',  ( -108.1330159686006027, -298.8790747090135369, -245.0902251058344348 ) ) ;
#7776 = CARTESIAN_POINT ( 'NONE',  ( -6.024775384615294271, -229.5268262511776527, 22.50000000000000000 ) ) ;
#7777 = CARTESIAN_POINT ( 'NONE',  ( -30.50603757819384754, -285.3378227149538588, -197.4687663638026152 ) ) ;
#7778 = CARTESIAN_POINT ( 'NONE',  ( -110.4970133349439436, -276.6457991668419822, -281.5982957252188612 ) ) ;
#7779 = CARTESIAN_POINT ( 'NONE',  ( -18.88656183603281136, -275.3845748300075797, -341.5986276675744762 ) ) ;
#7780 = CARTESIAN_POINT ( 'NONE',  ( -97.41917347918865744, -285.9388096817781388, -315.2787732009737738 ) ) ;
#7781 = CARTESIAN_POINT ( 'NONE',  ( 30.53621410309122552, -276.3834113618925130, -242.3042780304308224 ) ) ;
#7782 = CARTESIAN_POINT ( 'NONE',  ( 175.2296996224749250, 215.0000000000000568, -24.99999999999999289 ) ) ;
#7783 = CARTESIAN_POINT ( 'NONE',  ( 22.14672521501110225, -273.3072902055077407, -222.7214346415330795 ) ) ;
#7784 = CARTESIAN_POINT ( 'NONE',  ( -91.76439620766440441, -281.2790824145556030, -218.4388812317861834 ) ) ;
#7785 = CARTESIAN_POINT ( 'NONE',  ( 152.0840361487231860, 129.8837617311558290, 12.49999999999999822 ) ) ;
#7786 = CARTESIAN_POINT ( 'NONE',  ( -29.10930434397941013, -290.8688905168899623, -345.5238421913936122 ) ) ;
#7787 = CARTESIAN_POINT ( 'NONE',  ( 11.41685575594190105, -292.3764198906819729, -327.4164581689026932 ) ) ;
#7788 = ADVANCED_FACE ( 'NONE', ( #36462 ), #44488, .T. ) ;
#7789 = DIRECTION ( 'NONE',  ( -1.000000000000000000, 0.000000000000000000, -0.000000000000000000 ) ) ;
#7790 = CARTESIAN_POINT ( 'NONE',  ( -70.63401616881532163, -296.3979187062666369, -204.9349602359829987 ) ) ;
#7791 = CARTESIAN_POINT ( 'NONE',  ( -57.97593008291472216, -289.9224807047769445, -198.9975062916075217 ) ) ;
#7792 = CARTESIAN_POINT ( 'NONE',  ( 207.9739649226136180, 291.4638663531892462, -68.48153742335392735 ) ) ;
#7793 = CARTESIAN_POINT ( 'NONE',  ( 201.2104617360081704, 15.00000000000000000, -10.00000000000000000 ) ) ;
#7794 = CARTESIAN_POINT ( 'NONE',  ( -12.46819195455078422, -287.2144499604723933, -342.5553490690209628 ) ) ;
#7795 = CARTESIAN_POINT ( 'NONE',  ( -89.17837263452987884, -283.5751211425088059, -214.7293962043702606 ) ) ;
#7796 = CARTESIAN_POINT ( 'NONE',  ( -92.99292412680347297, -285.2966533060040319, -318.5291841698085591 ) ) ;
#7797 = CARTESIAN_POINT ( 'NONE',  ( -109.7735294940198116, -285.4906532609048213, -260.0542357320898645 ) ) ;
#7798 = CARTESIAN_POINT ( 'NONE',  ( -72.38608958492390855, -291.4933863839065111, -337.0861078632919430 ) ) ;
#7799 = CARTESIAN_POINT ( 'NONE',  ( -49.72002346270375028, -274.2318256799778737, -194.3302159693817543 ) ) ;
#7800 = CARTESIAN_POINT ( 'NONE',  ( -97.19236366976461738, -289.2594414276187536, -224.2184801119245208 ) ) ;
#7801 = CARTESIAN_POINT ( 'NONE',  ( 8.241063248432322297, -276.4480114231924404, -332.4852636165502417 ) ) ;
#7802 = CARTESIAN_POINT ( 'NONE',  ( 20.99466275004447979, -296.1755330987402886, -316.9509738207449345 ) ) ;
#7803 = CARTESIAN_POINT ( 'NONE',  ( -48.18343439339131606, -268.0651010539579033, -439.6569430059153092 ) ) ;
#7804 = CARTESIAN_POINT ( 'NONE',  ( -69.91165696735023971, -294.1233781216987495, -202.8022627189028810 ) ) ;
#7805 = CARTESIAN_POINT ( 'NONE',  ( -36.20257361892731041, -281.7223979839528738, -343.8454419590273687 ) ) ;
#7806 = CARTESIAN_POINT ( 'NONE',  ( -92.01835198473742139, -275.8299030656888817, -322.0157949895496472 ) ) ;
#7807 = CARTESIAN_POINT ( 'NONE',  ( -113.4877042674186640, -271.1039975042810397, -264.6586001561869921 ) ) ;
#7808 = CARTESIAN_POINT ( 'NONE',  ( 34.80639335941709334, -275.0598188850057682, -282.4372946443554611 ) ) ;
#7809 = CARTESIAN_POINT ( 'NONE',  ( 33.97433270854487830, -294.8294560904062109, -251.7941792345553722 ) ) ;
#7810 = CARTESIAN_POINT ( 'NONE',  ( 28.61165144478358968, -294.9242566572890496, -302.3146262542020963 ) ) ;
#7811 = CARTESIAN_POINT ( 'NONE',  ( 25.99424740338993445, -294.4087614943904896, -227.5227332453404188 ) ) ;
#7812 = CARTESIAN_POINT ( 'NONE',  ( 35.90248460558718335, -295.1485931673587402, -292.6447351935624397 ) ) ;
#7813 = CARTESIAN_POINT ( 'NONE',  ( -72.12644790865400068, -295.3591005119073998, -334.5549892667825702 ) ) ;
#7814 = CARTESIAN_POINT ( 'NONE',  ( -112.1144590672487880, -292.4692947643744105, -276.8270073976423760 ) ) ;
#7815 = CARTESIAN_POINT ( 'NONE',  ( -108.2263092204673143, -284.3345099156609876, -300.5702927562213631 ) ) ;
#7816 = CARTESIAN_POINT ( 'NONE',  ( 13.15909497732119249, -272.8882905716575920, -213.8111232551791545 ) ) ;
#7817 = CARTESIAN_POINT ( 'NONE',  ( 39.57775978659211802, -287.3286859626279579, -265.8205126028088898 ) ) ;
#7818 = CARTESIAN_POINT ( 'NONE',  ( -35.04226508535295181, -279.0030212258500910, -344.9704967766186314 ) ) ;
#7819 = CARTESIAN_POINT ( 'NONE',  ( -46.76070133416745023, -284.7249658739941083, -197.5198690464767139 ) ) ;
#7820 = CARTESIAN_POINT ( 'NONE',  ( 10.81346653292563786, -284.7174067719048480, -212.7948037001758053 ) ) ;
#7821 = CARTESIAN_POINT ( 'NONE',  ( -97.57965056221893008, -277.3145912500148142, -224.3868114770451712 ) ) ;
#7822 = CARTESIAN_POINT ( 'NONE',  ( -90.78337343436103879, -230.3218577325732781, -348.1307343985224634 ) ) ;
#7823 = CARTESIAN_POINT ( 'NONE',  ( -77.07727883789266343, -285.0118166057017675, -208.9898211045761229 ) ) ;
#7824 = AXIS2_PLACEMENT_3D ( 'NONE', #80114, #7677, #30388 ) ;
#7825 = CARTESIAN_POINT ( 'NONE',  ( 16.93090000069533829, -282.0091973299744268, -216.2266622698892604 ) ) ;
#7826 = CARTESIAN_POINT ( 'NONE',  ( -82.72322185915061254, -288.7145941210014257, -332.2750719646207358 ) ) ;
#7827 = CARTESIAN_POINT ( 'NONE',  ( -72.45373703409956079, -279.1090686605271003, -338.0039549217130457 ) ) ;
#7828 = ADVANCED_FACE ( 'NONE', ( #66291 ), #79375, .T. ) ;
#7829 = CARTESIAN_POINT ( 'NONE',  ( -17.46974813775018021, -278.1161131322775759, -344.2421290448695572 ) ) ;
#7831 = EDGE_CURVE ( 'NONE', #89245, #73999, #37835, .T. ) ;
#7830 = CARTESIAN_POINT ( 'NONE',  ( -5.556575836668641521, -280.3156372975103636, -204.6442565365026098 ) ) ;
#7832 = CARTESIAN_POINT ( 'NONE',  ( 0.2610015416381004649, -276.5353930609064150, -205.8645475316958482 ) ) ;
#7833 = CARTESIAN_POINT ( 'NONE',  ( 37.46000585225958446, -293.7812842492056120, -288.6838769745202171 ) ) ;
#7834 = CARTESIAN_POINT ( 'NONE',  ( -56.51179552487676006, -287.3203993690483458, -342.5560744034848994 ) ) ;
#7835 = AXIS2_PLACEMENT_3D ( 'NONE', #60451, #30161, #66613 ) ;
#7836 = CARTESIAN_POINT ( 'NONE',  ( -101.0266835503384186, -292.7091322717921571, -228.4254666199307451 ) ) ;
#7837 = CARTESIAN_POINT ( 'NONE',  ( 18.19765951440566099, -293.1512774009930240, -318.2300770456562304 ) ) ;
#7838 = CARTESIAN_POINT ( 'NONE',  ( 34.50474111316298576, -293.0459148747185623, -257.2464007213786772 ) ) ;
#7839 = CARTESIAN_POINT ( 'NONE',  ( -106.9855132839358305, -292.0456940053614971, -238.1217449781401001 ) ) ;
#7840 = CARTESIAN_POINT ( 'NONE',  ( 32.83011356680909643, -281.9328945366125936, -249.8718712637184467 ) ) ;
#7841 = CARTESIAN_POINT ( 'NONE',  ( -36.17635543328511716, -296.9867554724299907, -193.6704353362449922 ) ) ;
#7842 = CARTESIAN_POINT ( 'NONE',  ( -17.74229264157356312, -289.4571983152096095, -344.7195473127935088 ) ) ;
#7843 = CARTESIAN_POINT ( 'NONE',  ( -19.23689546071541301, -280.9613325135925379, -343.9850312482377035 ) ) ;
#7844 = CARTESIAN_POINT ( 'NONE',  ( 12.40539572523971401, -288.7142162585620326, -329.1060815590088851 ) ) ;
#7845 = CARTESIAN_POINT ( 'NONE',  ( -77.06412516446302163, -285.8373119732323744, -209.0294615953273194 ) ) ;
#7846 = CARTESIAN_POINT ( 'NONE',  ( 208.4306832106270804, -124.2391364535881024, 0.000000000000000000 ) ) ;
#7847 = CARTESIAN_POINT ( 'NONE',  ( -49.42433641670088207, -154.1833738735614077, -363.2467176495409831 ) ) ;
#7848 = CARTESIAN_POINT ( 'NONE',  ( 201.9871895515904043, 292.2036489450776457, -53.99999999998372147 ) ) ;
#7849 = CARTESIAN_POINT ( 'NONE',  ( -79.13876353550847398, -278.6691146984443321, -210.3144093544044608 ) ) ;
#7850 = CARTESIAN_POINT ( 'NONE',  ( -71.07170645813098986, -278.5164105010307480, -205.2584726204851222 ) ) ;
#7851 = CARTESIAN_POINT ( 'NONE',  ( -31.25750281044283696, -273.7937095030862906, -193.6097999099276592 ) ) ;
#7852 = CARTESIAN_POINT ( 'NONE',  ( -106.8576566752619783, -266.2287397320313289, -305.9886098359324933 ) ) ;
#7853 = CARTESIAN_POINT ( 'NONE',  ( -72.22152776909865679, -278.1746721828476439, -202.3612588296030026 ) ) ;
#7854 = CARTESIAN_POINT ( 'NONE',  ( -54.08253899494208383, -281.2881180102810958, -343.1577038242150479 ) ) ;
#7855 = CARTESIAN_POINT ( 'NONE',  ( 28.70513694042041308, -295.8079305119152878, -308.0412502057671986 ) ) ;
#7856 = CARTESIAN_POINT ( 'NONE',  ( -9.710012036928262091, -292.9153293096463244, -202.6724007151781564 ) ) ;
#7857 = CARTESIAN_POINT ( 'NONE',  ( -29.13456773689200219, -287.6307889366717632, -343.3945791871334450 ) ) ;
#7858 = CARTESIAN_POINT ( 'NONE',  ( -15.81385885964917470, -274.9748115644696327, -196.4826544351321616 ) ) ;
#7859 = CARTESIAN_POINT ( 'NONE',  ( -93.08102006560196173, -296.0486911266057177, -317.5199371560336203 ) ) ;
#7860 = ORIENTED_EDGE ( 'NONE', *, *, #59380, .T. ) ;
#7861 = DIRECTION ( 'NONE',  ( -0.000000000000000000, -1.000000000000000000, -0.000000000000000000 ) ) ;
#7862 = ADVANCED_FACE ( 'NONE', ( #88504 ), #81436, .T. ) ;
#7863 = CARTESIAN_POINT ( 'NONE',  ( -109.9602055073348765, -280.7390416093109025, -249.4836929548602029 ) ) ;
#7864 = CARTESIAN_POINT ( 'NONE',  ( -34.31426914201708911, -281.1707443673003013, -197.1019463498369078 ) ) ;
#7865 = CARTESIAN_POINT ( 'NONE',  ( -109.6948069130452694, -280.0145456464238691, -293.7467858612341161 ) ) ;
#7866 = CARTESIAN_POINT ( 'NONE',  ( 29.52441060181652333, -281.0133473354478042, -300.3575081863629634 ) ) ;
#7867 = CARTESIAN_POINT ( 'NONE',  ( -4.986337434218993003, -272.9659516091461455, -204.1366003303986929 ) ) ;
#7868 = DIRECTION ( 'NONE',  ( 0.000000000000000000, 0.000000000000000000, 1.000000000000000000 ) ) ;
#7869 = CARTESIAN_POINT ( 'NONE',  ( 175.2296996224750103, 275.5000000000000568, 0.000000000000000000 ) ) ;
#7870 = CARTESIAN_POINT ( 'NONE',  ( 38.56648807445828453, -276.2045202652068383, -258.3555646900310308 ) ) ;
#7871 = ORIENTED_EDGE ( 'NONE', *, *, #31927, .T. ) ;
#7872 = CARTESIAN_POINT ( 'NONE',  ( 15.56298187118347265, -278.3045312282047234, -323.5946947879721165 ) ) ;
#7873 = CARTESIAN_POINT ( 'NONE',  ( -92.91799830677950922, -276.4046985153819946, -322.8763751534348216 ) ) ;
#7874 = ORIENTED_EDGE ( 'NONE', *, *, #47697, .T. ) ;
#7875 = DIRECTION ( 'NONE',  ( 0.000000000000000000, 0.000000000000000000, -1.000000000000000000 ) ) ;
#7876 = CARTESIAN_POINT ( 'NONE',  ( -110.9136329199378537, -286.3237800610236263, -286.6576670865500205 ) ) ;
#7877 = CARTESIAN_POINT ( 'NONE',  ( -92.67193276102551636, -290.4298858457653409, -222.4949808486858274 ) ) ;
#7878 = CARTESIAN_POINT ( 'NONE',  ( 22.01678789598922847, -286.2430670753387858, -221.4746915785638635 ) ) ;
#7879 = CARTESIAN_POINT ( 'NONE',  ( -94.21492683277554647, -282.1291721564969066, -317.7257683049259640 ) ) ;
#7881 = CARTESIAN_POINT ( 'NONE',  ( 19.78221980405417568, -284.9674739533084562, -222.6110511891691317 ) ) ;
#7880 = CARTESIAN_POINT ( 'NONE',  ( -98.02848019283301539, -282.5510825744433419, -312.0731454985016171 ) ) ;
#7882 = CARTESIAN_POINT ( 'NONE',  ( 34.33146479532327078, -282.9647166658353967, -286.1752868207253186 ) ) ;
#7883 = CARTESIAN_POINT ( 'NONE',  ( -69.25692826692680626, -271.6322069577688580, -202.4764768922208020 ) ) ;
#7884 = AXIS2_PLACEMENT_3D ( 'NONE', #25803, #76484, #69842 ) ;
#7885 = CARTESIAN_POINT ( 'NONE',  ( -109.4740261224480093, -282.6392924544429093, -294.9246674279370382 ) ) ;
#7886 = CARTESIAN_POINT ( 'NONE',  ( -112.3648795842791941, -298.5256188982440335, -272.4404370897309491 ) ) ;
#7887 = AXIS2_PLACEMENT_3D ( 'NONE', #8841, #66625, #1749 ) ;
#7888 = CARTESIAN_POINT ( 'NONE',  ( -68.63467242439438110, -280.5716956690453685, -204.1481409026625897 ) ) ;
#7889 = CARTESIAN_POINT ( 'NONE',  ( -70.28624685163519814, -287.6191410373857593, -202.7986633752721275 ) ) ;
#7890 = CARTESIAN_POINT ( 'NONE',  ( 196.5838024899613856, 20.48082335702326873, 13.01360888346138367 ) ) ;
#7891 = AXIS2_PLACEMENT_3D ( 'NONE', #79436, #65710, #822 ) ;
#7892 = LINE ( 'NONE', #92669, #77655 ) ;
#7893 = CARTESIAN_POINT ( 'NONE',  ( 35.31267797015716781, -295.2066607720008733, -249.5617856799250660 ) ) ;
#7894 = VECTOR ( 'NONE', #56981, 1000.000000000000000 ) ;
#7895 = CARTESIAN_POINT ( 'NONE',  ( -107.1381010420987394, -276.1947112032342488, -297.8103996846610926 ) ) ;
#7896 = CARTESIAN_POINT ( 'NONE',  ( -23.35139513059944960, -288.0749500300123032, -345.9692720543474707 ) ) ;
#7897 = CARTESIAN_POINT ( 'NONE',  ( 22.46485579483354300, -291.3534596134875301, -227.1005611582333472 ) ) ;
#7898 = CARTESIAN_POINT ( 'NONE',  ( -108.9706615412812596, -277.0207249879943561, -286.8649032456038412 ) ) ;
#7899 = CARTESIAN_POINT ( 'NONE',  ( -87.33907527759036782, -293.8978430308621910, -325.2348635833365051 ) ) ;
#7900 = CARTESIAN_POINT ( 'NONE',  ( -92.94047739810316955, -292.5475500958058319, -222.2984563303981247 ) ) ;
#7901 = CARTESIAN_POINT ( 'NONE',  ( 35.77081079830085031, -277.8376638359845288, -253.6410175316879361 ) ) ;
#7902 = CARTESIAN_POINT ( 'NONE',  ( -27.85341573640096513, -293.4137773554000432, -346.1283948010387803 ) ) ;
#7903 = CARTESIAN_POINT ( 'NONE',  ( 35.75556045586952791, -289.2860665322921818, -280.6135695641382881 ) ) ;
#7904 = CARTESIAN_POINT ( 'NONE',  ( -113.1040745153595992, -288.7098464367003317, -276.8445238061522673 ) ) ;
#7905 = CARTESIAN_POINT ( 'NONE',  ( 3.960202679077717836, -289.9094446596550370, -331.3284650955091024 ) ) ;
#7906 = DIRECTION ( 'NONE',  ( 0.000000000000000000, -1.000000000000000000, 0.000000000000000000 ) ) ;
#7907 = CARTESIAN_POINT ( 'NONE',  ( -78.25627047467871478, -290.4206444389456578, -331.0735626091944823 ) ) ;
#7908 = CARTESIAN_POINT ( 'NONE',  ( 161.2244399300530233, 8.542400036368780647, 25.74970488511327815 ) ) ;
#7909 = CARTESIAN_POINT ( 'NONE',  ( -15.05304048304508058, -289.9749397069415977, -343.7052226039473339 ) ) ;
#7910 = CARTESIAN_POINT ( 'NONE',  ( -87.81075411548221155, -277.3710099016477670, -214.4032642897158780 ) ) ;
#7911 = CARTESIAN_POINT ( 'NONE',  ( -106.1585801564188785, -279.3306217380792873, -235.7462808467416835 ) ) ;
#7912 = CARTESIAN_POINT ( 'NONE',  ( 30.70510843258561451, -280.7527074191285124, -234.2561307284209988 ) ) ;
#7913 = CARTESIAN_POINT ( 'NONE',  ( 36.98155252631730860, -285.4180333054229095, -259.9282364223599302 ) ) ;
#7914 = CARTESIAN_POINT ( 'NONE',  ( 209.5027106082920056, 29.50523358103493621, 14.69807322781335479 ) ) ;
#7915 = CARTESIAN_POINT ( 'NONE',  ( -24.64217692196449860, -278.3554982582028288, -197.2202430342596529 ) ) ;
#7916 = CARTESIAN_POINT ( 'NONE',  ( -78.09490476767805944, -281.5999099516347428, -333.3228282422173265 ) ) ;
#7917 = CARTESIAN_POINT ( 'NONE',  ( 156.1449889021179160, 215.0000000000000568, 16.91223866672558529 ) ) ;
#7918 = CARTESIAN_POINT ( 'NONE',  ( -98.26169566711723746, -276.4143253438988381, -316.3332161561735347 ) ) ;
#7919 = CARTESIAN_POINT ( 'NONE',  ( -104.1545026975579020, -282.9807547602968611, -308.1189680917823921 ) ) ;
#7920 = CARTESIAN_POINT ( 'NONE',  ( -65.88555339742242722, -274.4717160403345133, -202.9975509168688745 ) ) ;
#7921 = CARTESIAN_POINT ( 'NONE',  ( -92.28220072421791542, -292.8499697486639661, -221.0676545624600635 ) ) ;
#7922 = CARTESIAN_POINT ( 'NONE',  ( -23.48784656349971200, -299.5373519014282806, -193.8512418494217684 ) ) ;
#7923 = CARTESIAN_POINT ( 'NONE',  ( 26.65710265469163076, -274.7374777641269930, -235.0955074956486897 ) ) ;
#7924 = CARTESIAN_POINT ( 'NONE',  ( -9.730641833557097442, -296.6916292594438573, -340.0936793098232442 ) ) ;
#7925 = CARTESIAN_POINT ( 'NONE',  ( -28.97506936117078169, -289.1156991169128787, -346.9587456471790574 ) ) ;
#7926 = CARTESIAN_POINT ( 'NONE',  ( 18.12012216225994266, -278.9197260147113866, -219.0454238271456120 ) ) ;
#7927 = CARTESIAN_POINT ( 'NONE',  ( -33.53724234021917994, -291.9321216610143210, -193.4551617408098991 ) ) ;
#7928 = EDGE_CURVE ( 'NONE', #75392, #14315, #38307, .T. ) ;
#7929 = CARTESIAN_POINT ( 'NONE',  ( -94.29480758823179087, -288.9618003250732841, -316.4018825239820671 ) ) ;
#7930 = CARTESIAN_POINT ( 'NONE',  ( 22.41950978074509493, -292.1718727155264901, -315.6777643980386188 ) ) ;
#7931 = ORIENTED_EDGE ( 'NONE', *, *, #29868, .F. ) ;
#7932 = CARTESIAN_POINT ( 'NONE',  ( 197.1016235222741670, 72.78816326493900135, 12.11671654626785433 ) ) ;
#7933 = CARTESIAN_POINT ( 'NONE',  ( -110.3986519023002302, -290.0490111061756124, -271.1797991876197784 ) ) ;
#7934 = CARTESIAN_POINT ( 'NONE',  ( 196.7510731661265595, -143.7221692137691775, -22.50000000000000000 ) ) ;
#7935 = CARTESIAN_POINT ( 'NONE',  ( -57.70509259614949826, -286.7368315208547642, -196.2913908803028846 ) ) ;
#7936 = CARTESIAN_POINT ( 'NONE',  ( -105.5937364680635966, -293.2662352645559167, -254.8156830097664738 ) ) ;
#7937 = CARTESIAN_POINT ( 'NONE',  ( -36.28973329757899080, -294.0980555643682237, -347.1316803670979994 ) ) ;
#7938 = EDGE_CURVE ( 'NONE', #8402, #38700, #69074, .T. ) ;
#7939 = CARTESIAN_POINT ( 'NONE',  ( 39.03799595980812853, -282.9333955015293895, -275.6102689358332896 ) ) ;
#7940 = CARTESIAN_POINT ( 'NONE',  ( -85.72456080356995756, -285.1937654039052177, -215.6300524162169552 ) ) ;
#7941 = CARTESIAN_POINT ( 'NONE',  ( 17.64344766955986898, -276.1744823984302002, -221.5222512166006936 ) ) ;
#7942 = CARTESIAN_POINT ( 'NONE',  ( -25.98140794945219412, -292.9268743664404155, -344.1363886498006082 ) ) ;
#7943 = CARTESIAN_POINT ( 'NONE',  ( 35.41613615781426461, -274.2202530623489452, -260.6953141466017314 ) ) ;
#7944 = ORIENTED_EDGE ( 'NONE', *, *, #679, .T. ) ;
#7945 = CARTESIAN_POINT ( 'NONE',  ( 195.7340404941960514, 41.37717207137899322, 12.47808917857981470 ) ) ;
#7946 = CARTESIAN_POINT ( 'NONE',  ( 15.46109875539708689, -293.9964709504282041, -326.3754797260445457 ) ) ;
#7947 = CARTESIAN_POINT ( 'NONE',  ( -14.13994448591539310, -288.2754540701741348, -199.5752238779358265 ) ) ;
#7948 = CARTESIAN_POINT ( 'NONE',  ( -76.91091064297273761, -296.6483323364652733, -336.1174144921039328 ) ) ;
#7949 = ADVANCED_FACE ( 'NONE', ( #46795 ), #81393, .F. ) ;
#7950 = CARTESIAN_POINT ( 'NONE',  ( 33.12531798419511375, -287.9469192570459768, -250.9113872191048813 ) ) ;
#7951 = CARTESIAN_POINT ( 'NONE',  ( -112.8364222513997248, -277.4355549987857330, -284.3390504998582173 ) ) ;
#7952 = CARTESIAN_POINT ( 'NONE',  ( -19.30313127504841475, -295.4775053082207705, -345.1683424128270303 ) ) ;
#7953 = CARTESIAN_POINT ( 'NONE',  ( -23.56025265417988379, -287.0175368800004776, -344.9152156619758784 ) ) ;
#7954 = CARTESIAN_POINT ( 'NONE',  ( 35.46780223414203448, -294.2023151367526452, -295.5149038562099122 ) ) ;
#7956 = CARTESIAN_POINT ( 'NONE',  ( -6.036413579860385070, -292.8085834472713032, -204.3771384064993697 ) ) ;
#7955 = CIRCLE ( 'NONE', #60888, 7.999911143031724237 ) ;
#7957 = DIRECTION ( 'NONE',  ( 1.000000000000000000, 0.000000000000000000, 0.000000000000000000 ) ) ;
#7958 = CARTESIAN_POINT ( 'NONE',  ( 139.1539576904058606, 249.5000000000000568, 10.50000000000000000 ) ) ;
#7959 = CARTESIAN_POINT ( 'NONE',  ( -21.04059066060629135, -109.3119883924524771, -359.1154128302550816 ) ) ;
#7960 = CARTESIAN_POINT ( 'NONE',  ( -2.556400534608909147, -288.0238275467715994, -202.4297073922786865 ) ) ;
#7961 = CARTESIAN_POINT ( 'NONE',  ( -19.05039376806006857, -283.7666405000204009, -190.3683826091709363 ) ) ;
#7962 = EDGE_LOOP ( 'NONE', ( #25311, #79005, #28023, #91449 ) ) ;
#7963 = CIRCLE ( 'NONE', #481, 25.50000000000000355 ) ;
#7964 = CARTESIAN_POINT ( 'NONE',  ( -112.3005092421667115, -278.1156456214510513, -253.2004151000520267 ) ) ;
#7965 = CARTESIAN_POINT ( 'NONE',  ( -96.55178080688489217, -285.9235182833341469, -316.1443998227013594 ) ) ;
#7966 = CARTESIAN_POINT ( 'NONE',  ( -103.9126535757035015, -282.6352095054799065, -307.9771861908458845 ) ) ;
#7968 = CARTESIAN_POINT ( 'NONE',  ( -10.22183121759466573, -286.7753876966069697, -339.7404668137065187 ) ) ;
#7967 = CIRCLE ( 'NONE', #68461, 5.568361562975243650 ) ;
#7969 = CARTESIAN_POINT ( 'NONE',  ( -35.57669818200841405, -275.9344558797519653, -194.6039557898241696 ) ) ;
#7970 = CARTESIAN_POINT ( 'NONE',  ( -107.8967211018427008, -297.2954636387335654, -251.3398210208746093 ) ) ;
#7971 = CARTESIAN_POINT ( 'NONE',  ( 23.33070614837535928, -292.8112814322578856, -311.9242032630952508 ) ) ;
#7972 = CARTESIAN_POINT ( 'NONE',  ( 20.98336255574975695, -281.5260210089689394, -220.2262317231332247 ) ) ;
#7974 = CARTESIAN_POINT ( 'NONE',  ( -83.49568151612434974, -278.7486767383157371, -213.6060776626616189 ) ) ;
#7973 = CARTESIAN_POINT ( 'NONE',  ( 33.58653086281132971, -275.7806169780106984, -287.6818394754311043 ) ) ;
#7975 = CARTESIAN_POINT ( 'NONE',  ( -41.19106775703900780, -275.0845710428190500, -193.7148463023310114 ) ) ;
#7976 = CARTESIAN_POINT ( 'NONE',  ( -6.710842559334417423, -275.5797089320426494, -340.6835161545515120 ) ) ;
#7977 = CARTESIAN_POINT ( 'NONE',  ( -48.55409767859317327, -154.7049544282948546, -365.0407483515516560 ) ) ;
#7978 = CARTESIAN_POINT ( 'NONE',  ( -26.80725467259023986, -274.9181422207075798, -344.6694346137963976 ) ) ;
#7979 = CARTESIAN_POINT ( 'NONE',  ( -112.8104714642036157, -298.1292117583039385, -258.3168843575630262 ) ) ;
#7980 = CARTESIAN_POINT ( 'NONE',  ( -69.85430415644619018, -279.9805209788416391, -337.9475929042657754 ) ) ;
#7981 = CARTESIAN_POINT ( 'NONE',  ( 202.9739649223127742, 291.4636489454787807, -68.19743562414970484 ) ) ;
#7982 = CARTESIAN_POINT ( 'NONE',  ( -89.89400091338661980, -286.3684677463857611, -219.1758144907784640 ) ) ;
#7983 = CARTESIAN_POINT ( 'NONE',  ( -32.39507036174258303, -287.8738255240219814, -194.5226353243144217 ) ) ;
#7984 = CARTESIAN_POINT ( 'NONE',  ( 19.59981007584344681, -286.2532955138565853, -224.4985394635234002 ) ) ;
#7985 = CARTESIAN_POINT ( 'NONE',  ( -106.0196446601928102, -276.5946788698287264, -297.3755650157638115 ) ) ;
#7986 = CARTESIAN_POINT ( 'NONE',  ( -95.23363775000161979, -285.7665605741071317, -316.8505576613182484 ) ) ;
#7987 = CARTESIAN_POINT ( 'NONE',  ( -96.15348774456148817, -277.6502049444628710, -225.9343076109350932 ) ) ;
#7988 = CARTESIAN_POINT ( 'NONE',  ( -97.27824057330747110, -279.2771582993402717, -312.9135989107572868 ) ) ;
#7989 = AXIS2_PLACEMENT_3D ( 'NONE', #83286, #83760, #3773 ) ;
#7990 = CARTESIAN_POINT ( 'NONE',  ( 34.22610807783807019, -276.2382313293148286, -285.0593243508667456 ) ) ;
#7991 = CARTESIAN_POINT ( 'NONE',  ( 38.95060028379592154, -286.4337139448103926, -277.2526791771106787 ) ) ;
#7992 = CARTESIAN_POINT ( 'NONE',  ( -5.021231372576554719, -281.2697649534921993, -200.6506731364722498 ) ) ;
#7993 = CARTESIAN_POINT ( 'NONE',  ( 37.80677678180712320, -282.2517723688818592, -286.9214769481020539 ) ) ;
#7994 = ORIENTED_EDGE ( 'NONE', *, *, #24610, .F. ) ;
#7995 = VERTEX_POINT ( 'NONE', #4202 ) ;
#7996 = DIRECTION ( 'NONE',  ( -0.8510748438184358999, -0.5250018354872690862, -0.006684530980050039546 ) ) ;
#7997 = CARTESIAN_POINT ( 'NONE',  ( 15.83615169445521254, -290.1695175808054614, -324.4009525675751320 ) ) ;
#7998 = CARTESIAN_POINT ( 'NONE',  ( -112.1541873705144781, -289.4392702276746832, -254.2871902977917387 ) ) ;
#7999 = CARTESIAN_POINT ( 'NONE',  ( -8.669945598421884725, -296.2834264217712530, -341.0170974821744494 ) ) ;
#8000 = CARTESIAN_POINT ( 'NONE',  ( -44.57489798370398404, -297.1555933027912602, -197.5075850789002345 ) ) ;
#8001 = CARTESIAN_POINT ( 'NONE',  ( -2.095157989460947778, -291.8549465728301584, -202.0016882125615609 ) ) ;
#8002 = CARTESIAN_POINT ( 'NONE',  ( 20.90040732358131947, -285.4021005891712548, -225.2106509410555759 ) ) ;
#8003 = B_SPLINE_CURVE_WITH_KNOTS ( 'NONE', 3,
 ( #24027, #10747, #33002, #60041, #39148, #61893, #40083, #68528 ),
 .UNSPECIFIED., .F., .F.,
 ( 4, 2, 2, 4 ),
 ( 0.000000000000000000, 0.0004662050538968414977, 0.0009324101077936829953, 0.001864820215587370978 ),
 .UNSPECIFIED. ) ;
#8004 = CARTESIAN_POINT ( 'NONE',  ( -0.7803967397976755427, -289.7604347740268622, -334.0623913322140766 ) ) ;
#8005 = CARTESIAN_POINT ( 'NONE',  ( -106.6662871844225293, -293.4805209788415823, -237.0123917617630980 ) ) ;
#8006 = CARTESIAN_POINT ( 'NONE',  ( 35.21617955764460817, -289.7962630860748732, -289.3441300505067488 ) ) ;
#8007 = CARTESIAN_POINT ( 'NONE',  ( 2.193668350929908417, -286.5242751726996175, -334.3516811274839142 ) ) ;
#8008 = CARTESIAN_POINT ( 'NONE',  ( -40.78026240149577575, -291.0955449567578626, -345.2948692940261708 ) ) ;
#8009 = CARTESIAN_POINT ( 'NONE',  ( -101.9732587860497546, -285.0242763615592025, -304.9098380994175841 ) ) ;
#8010 = CARTESIAN_POINT ( 'NONE',  ( -83.16926140034645698, -293.4268758796561656, -210.7147740084812710 ) ) ;
#8011 = CARTESIAN_POINT ( 'NONE',  ( 153.2628468892384603, 20.37991841447902175, -11.93555113919331134 ) ) ;
#8012 = CARTESIAN_POINT ( 'NONE',  ( -73.18521390427548567, -275.5596664071740634, -204.0184947702227589 ) ) ;
#8013 = CARTESIAN_POINT ( 'NONE',  ( -34.85126290705520091, -282.2172706411769241, -343.4926593903437606 ) ) ;
#8014 = CARTESIAN_POINT ( 'NONE',  ( -6.452414031569595032, -280.6463450089007665, -338.7188412135294016 ) ) ;
#8015 = CARTESIAN_POINT ( 'NONE',  ( -0.7920108885427427081, -293.7765922506057450, -337.9650164259404050 ) ) ;
#8016 = CARTESIAN_POINT ( 'NONE',  ( -79.41291222442505671, -271.7156659612984981, -209.4056313917288605 ) ) ;
#8017 = CARTESIAN_POINT ( 'NONE',  ( 12.69795933561254131, -274.4281117527275455, -325.5431708728868898 ) ) ;
#8018 = CARTESIAN_POINT ( 'NONE',  ( -108.9613680081086358, -298.0833784048866733, -253.8727386661447838 ) ) ;
#8019 = DIRECTION ( 'NONE',  ( 0.000000000000000000, 0.000000000000000000, -1.000000000000000000 ) ) ;
#8020 = CARTESIAN_POINT ( 'NONE',  ( -111.2830537992627740, -295.0139568837859656, -252.8496864380457794 ) ) ;
#8021 = AXIS2_PLACEMENT_3D ( 'NONE', #42595, #86150, #50174 ) ;
#8022 = CARTESIAN_POINT ( 'NONE',  ( -35.61876750191357388, -296.4554241701134174, -343.9427735942774120 ) ) ;
#8023 = CARTESIAN_POINT ( 'NONE',  ( 222.4306832106270804, -135.2391364535880882, 22.50000000000000000 ) ) ;
#8024 = CARTESIAN_POINT ( 'NONE',  ( -72.19251452969369609, -296.3284564878208585, -334.7028803549815166 ) ) ;
#8025 = FACE_OUTER_BOUND ( 'NONE', #2498, .T. ) ;
#8027 = CARTESIAN_POINT ( 'NONE',  ( -105.9871871336933395, -296.2195411300162391, -295.3451539059549305 ) ) ;
#8026 = CARTESIAN_POINT ( 'NONE',  ( -98.00479789158495691, -283.1801664615961727, -225.5718821187446679 ) ) ;
#8028 = CARTESIAN_POINT ( 'NONE',  ( -95.81656071533025454, -285.2288055099918438, -220.1843345743191662 ) ) ;
#8029 = CARTESIAN_POINT ( 'NONE',  ( -2.280207228873084802, -284.5119467509238689, -337.2939643009593738 ) ) ;
#8030 = CARTESIAN_POINT ( 'NONE',  ( 20.27374764682814146, -286.5264429128648658, -219.2314271746945451 ) ) ;
#8031 = CARTESIAN_POINT ( 'NONE',  ( -41.67413367338352970, -289.9974237825621799, -195.6021983822802213 ) ) ;
#8032 = PRESENTATION_LAYER_ASSIGNMENT (  '', '', ( #48848 ) ) ;
#8033 = CARTESIAN_POINT ( 'NONE',  ( -8.911334228678228442, -279.6119048896013055, -198.9757335164242988 ) ) ;
#8034 = CARTESIAN_POINT ( 'NONE',  ( -54.49178911615187815, -274.7666405000204009, -345.3538533559490702 ) ) ;
#8035 = VECTOR ( 'NONE', #18647, 1000.000000000000000 ) ;
#8036 = CARTESIAN_POINT ( 'NONE',  ( -43.39876772438888963, -263.1881392940089199, -501.4585950967926919 ) ) ;
#8037 = CARTESIAN_POINT ( 'NONE',  ( 34.39551870740162798, -286.5514388889804991, -285.9410210727103276 ) ) ;
#8038 = CARTESIAN_POINT ( 'NONE',  ( -77.98429921428237321, -288.5046875320861091, -335.4589974825216814 ) ) ;
#8039 = CARTESIAN_POINT ( 'NONE',  ( 82.64890176555634582, -299.5541904835127980, -188.7068768330456123 ) ) ;
#8040 = CARTESIAN_POINT ( 'NONE',  ( -96.75637080641293153, -298.7593735611004035, -226.5637852109154551 ) ) ;
#8041 = CARTESIAN_POINT ( 'NONE',  ( -105.8092805577969528, -279.5367008895115646, -304.4035007314972177 ) ) ;
#8043 = CARTESIAN_POINT ( 'NONE',  ( -5.545452586470449141, -280.1490631427390099, -204.6261491367922360 ) ) ;
#8042 = CARTESIAN_POINT ( 'NONE',  ( -58.41602785233541084, -293.3432175373289965, -342.7638291730453943 ) ) ;
#8044 = CARTESIAN_POINT ( 'NONE',  ( 13.39742235110125534, -294.5320294081415113, -328.3502179017373805 ) ) ;
#8045 = AXIS2_PLACEMENT_3D ( 'NONE', #26662, #19096, #40362 ) ;
#8046 = CARTESIAN_POINT ( 'NONE',  ( 15.31355574053964475, -284.8689055239517529, -216.1694375706188964 ) ) ;
#8047 = CARTESIAN_POINT ( 'NONE',  ( -109.8862592678147507, -280.3071135819704409, -289.4453676147621763 ) ) ;
#8048 = EDGE_CURVE ( 'NONE', #60407, #70970, #74830, .T. ) ;
#8049 = CARTESIAN_POINT ( 'NONE',  ( -96.28258130028333994, -296.2184039834166924, -226.8729404565453365 ) ) ;
#8050 = VERTEX_POINT ( 'NONE', #33077 ) ;
#8051 = DIRECTION ( 'NONE',  ( 0.000000000000000000, 1.000000000000000000, 0.000000000000000000 ) ) ;
#8052 = AXIS2_PLACEMENT_3D ( 'NONE', #67191, #2326, #31206 ) ;
#8053 = CARTESIAN_POINT ( 'NONE',  ( 35.66881769675151759, -283.3308813288306851, -254.7661243090953462 ) ) ;
#8054 = DIRECTION ( 'NONE',  ( 0.000000000000000000, 1.000000000000000000, 0.000000000000000000 ) ) ;
#8055 = CARTESIAN_POINT ( 'NONE',  ( -69.85430415644619018, -295.1237833571632905, -202.7746430608542312 ) ) ;
#8056 = CARTESIAN_POINT ( 'NONE',  ( 21.73328103353280127, -274.0870780364297161, -221.2255359479905223 ) ) ;
#8057 = CARTESIAN_POINT ( 'NONE',  ( -95.11308969468898056, -291.0137705497180036, -225.7352672671156029 ) ) ;
#8058 = CARTESIAN_POINT ( 'NONE',  ( 27.47396739210304872, -283.5462114003387342, -305.4272981945176753 ) ) ;
#8059 = CARTESIAN_POINT ( 'NONE',  ( -2.554364777748514115, -276.1205098279206709, -205.2743934086977617 ) ) ;
#8060 = AXIS2_PLACEMENT_3D ( 'NONE', #85266, #71074, #64474 ) ;
#8061 = CARTESIAN_POINT ( 'NONE',  ( 37.08855623747116681, -283.3593742402736098, -286.7486451572592614 ) ) ;
#8062 = CARTESIAN_POINT ( 'NONE',  ( 26.81331540313337314, -279.8622380372074758, -234.7063218668481568 ) ) ;
#8063 = CARTESIAN_POINT ( 'NONE',  ( -26.71359343580094503, -278.9171112211891455, -344.6042590453749881 ) ) ;
#8064 = VERTEX_POINT ( 'NONE', #68138 ) ;
#8065 = CARTESIAN_POINT ( 'NONE',  ( -46.87889485985060389, -273.7675372613273908, -193.9540376748857682 ) ) ;
#8066 = CARTESIAN_POINT ( 'NONE',  ( 35.48130958705406357, -295.6727240364586464, -285.8536021694327474 ) ) ;
#8067 = CARTESIAN_POINT ( 'NONE',  ( 159.4851178187871312, 0.000000000000000000, -10.00000000000000000 ) ) ;
#8068 = ADVANCED_FACE ( 'NONE', ( #17486 ), #64264, .T. ) ;
#8069 = CARTESIAN_POINT ( 'NONE',  ( 115.2940338803257703, -299.5541904835127980, -195.3611179825600175 ) ) ;
#8070 = CARTESIAN_POINT ( 'NONE',  ( 36.25441539508127420, -291.9211693323629788, -288.4130340596161659 ) ) ;
#8071 = CARTESIAN_POINT ( 'NONE',  ( -27.27550220494214628, -273.6910477003168012, -197.9454051131689596 ) ) ;
#8072 = CARTESIAN_POINT ( 'NONE',  ( 0.000000000000000000, 3.000000000000000000, -9.000000000000001776 ) ) ;
#8073 = EDGE_CURVE ( 'NONE', #14859, #53738, #38773, .T. ) ;
#8074 = CARTESIAN_POINT ( 'NONE',  ( -56.03781801345316183, -293.3358651313317864, -196.3258327148124067 ) ) ;
#8076 = CARTESIAN_POINT ( 'NONE',  ( 6.257574296360926880, -293.8349236778196314, -207.3761039925192051 ) ) ;
#8075 = CARTESIAN_POINT ( 'NONE',  ( 10.59707575819634329, -283.1948066931273047, -210.1954327657594490 ) ) ;
#8077 = CARTESIAN_POINT ( 'NONE',  ( -17.97508163599090736, -290.8022013000285710, -342.6989315005793628 ) ) ;
#8078 = CARTESIAN_POINT ( 'NONE',  ( -21.28384270088205099, -274.8456881282380664, -343.5045865777364611 ) ) ;
#8079 = CARTESIAN_POINT ( 'NONE',  ( -97.23738653589296632, -279.8644862052773306, -314.5845220144026939 ) ) ;
#8080 = CARTESIAN_POINT ( 'NONE',  ( 6.899508285148374220, -292.5250614885724190, -330.2921079519918521 ) ) ;
#8081 = CARTESIAN_POINT ( 'NONE',  ( 0.7324147085716452565, -282.4142087380836301, -204.7982106011602070 ) ) ;
#8082 = VERTEX_POINT ( 'NONE', #3259 ) ;
#8083 = CARTESIAN_POINT ( 'NONE',  ( -58.95843874355288960, -283.0062483690753083, -340.1624237813173295 ) ) ;
#8084 = CARTESIAN_POINT ( 'NONE',  ( -92.85951881761224058, -280.3587417919036966, -217.3771528269134592 ) ) ;
#8085 = VECTOR ( 'NONE', #1720, 1000.000000000000227 ) ;
#8086 = CARTESIAN_POINT ( 'NONE',  ( -27.43871699845037782, -281.7240578219924600, -346.3743220323171954 ) ) ;
#8087 = CARTESIAN_POINT ( 'NONE',  ( 3.386854982995440633, -277.4605135324746357, -335.4929283865736807 ) ) ;
#8088 = SHAPE_REPRESENTATION_RELATIONSHIP ( 'NONE' , 'NONE' ,  #54338, #140 ) ;
#8089 = CARTESIAN_POINT ( 'NONE',  ( 29.33222022470513934, -276.5855759547884531, -233.1405731757521380 ) ) ;
#8090 = CARTESIAN_POINT ( 'NONE',  ( -102.0172624299486870, -286.6233781216988064, -301.5434626090942061 ) ) ;
#8091 = EDGE_LOOP ( 'NONE', ( #18639, #18013, #41578, #5687 ) ) ;
#8092 = CARTESIAN_POINT ( 'NONE',  ( -55.81014109018446590, -299.8146850886207631, -197.6168102559092006 ) ) ;
#8093 = AXIS2_PLACEMENT_3D ( 'NONE', #41524, #78014, #78473 ) ;
#8094 = CARTESIAN_POINT ( 'NONE',  ( -32.33486341200443803, -275.0089483619669295, -344.8889075913206170 ) ) ;
#8095 = CARTESIAN_POINT ( 'NONE',  ( -53.20001070164216372, -293.6117907162477536, -195.9938901986680833 ) ) ;
#8096 = CARTESIAN_POINT ( 'NONE',  ( -30.78958769864947342, -291.4857469110150987, -197.5534089751789395 ) ) ;
#8097 = CARTESIAN_POINT ( 'NONE',  ( -20.51597483970617475, -288.3494539409715571, -345.4918477423779564 ) ) ;
#8098 = CARTESIAN_POINT ( 'NONE',  ( 143.6449502718966755, 0.000000000000000000, 10.00000000000000178 ) ) ;
#8100 = CARTESIAN_POINT ( 'NONE',  ( -76.56943090731783741, -281.9860072957666830, -332.9325681215935901 ) ) ;
#8099 = CARTESIAN_POINT ( 'NONE',  ( 37.48859745676208632, -291.9312284321855486, -254.8362292020100028 ) ) ;
#8101 = CARTESIAN_POINT ( 'NONE',  ( -99.12578378033575177, -291.8504972091675995, -311.5375296093928910 ) ) ;
#8102 = CARTESIAN_POINT ( 'NONE',  ( -109.4020804703804117, -282.8296436716500466, -285.8486754552714046 ) ) ;
#8103 = CARTESIAN_POINT ( 'NONE',  ( 22.99917629516962947, -283.4481504871378093, -312.3161190070868543 ) ) ;
#8104 = CARTESIAN_POINT ( 'NONE',  ( -37.48906997160655408, -289.9951653540702523, -347.1387154300267639 ) ) ;
#8105 = AXIS2_PLACEMENT_3D ( 'NONE', #49950, #85929, #42850 ) ;
#8106 = CARTESIAN_POINT ( 'NONE',  ( -34.31705220668383305, -280.5835150816415648, -197.3496601180021628 ) ) ;
#8107 = CARTESIAN_POINT ( 'NONE',  ( 24.50300054096744873, -291.7438655633978328, -225.1588866379612455 ) ) ;
#8108 = CARTESIAN_POINT ( 'NONE',  ( 18.22763561303820268, -287.6270598464529940, -217.2164403377509814 ) ) ;
#8109 = CARTESIAN_POINT ( 'NONE',  ( -14.96415025754044947, -289.2623259260079180, -344.0291359362524872 ) ) ;
#8110 = CARTESIAN_POINT ( 'NONE',  ( -7.018441519922675731, -286.6281392526678360, -203.9433253405669859 ) ) ;
#8111 = ORIENTED_EDGE ( 'NONE', *, *, #51306, .T. ) ;
#8112 = CARTESIAN_POINT ( 'NONE',  ( 195.0876680567968720, 25.98883653703275343, 13.48929546537064716 ) ) ;
#8113 = CARTESIAN_POINT ( 'NONE',  ( 38.01124758832005313, -295.5189946042634119, -278.7344361196631439 ) ) ;
#8114 = CIRCLE ( 'NONE', #54944, 1.000000000000000888 ) ;
#8115 = CARTESIAN_POINT ( 'NONE',  ( -37.70356343775669927, -293.7413911527011692, -346.8801077522113019 ) ) ;
#8116 = CARTESIAN_POINT ( 'NONE',  ( -109.2766588292207075, -277.4293624597767121, -284.1667998989694297 ) ) ;
#8117 = CARTESIAN_POINT ( 'NONE',  ( -34.04404987219109557, -297.4410138449539431, -193.4634035313384004 ) ) ;
#8118 = CARTESIAN_POINT ( 'NONE',  ( 31.48276417105896030, -291.6835363480417982, -244.0191198579662455 ) ) ;
#8119 = CARTESIAN_POINT ( 'NONE',  ( -0.05486954881660670996, -276.3156775524662407, -206.4114672360272493 ) ) ;
#8120 = CARTESIAN_POINT ( 'NONE',  ( -88.81459125358490780, -295.5575627746709984, -217.1057959254890193 ) ) ;
#8121 = CARTESIAN_POINT ( 'NONE',  ( 36.01771416011681026, -294.7263899151772648, -268.0101949775855132 ) ) ;
#8122 = CARTESIAN_POINT ( 'NONE',  ( 11.12490944502650869, -293.8214164374300026, -215.2914478877239617 ) ) ;
#8123 = FACE_OUTER_BOUND ( 'NONE', #12515, .T. ) ;
#8124 = CIRCLE ( 'NONE', #3589, 0.5000000000000001110 ) ;
#8125 = CARTESIAN_POINT ( 'NONE',  ( -98.53128193849934746, -293.9586314598638523, -314.1050217684543782 ) ) ;
#8126 = CARTESIAN_POINT ( 'NONE',  ( -105.3926320780602168, -298.1367108294285231, -302.0119830350562324 ) ) ;
#8127 = CARTESIAN_POINT ( 'NONE',  ( -88.81796530879852014, -290.7383936896437717, -322.4533685666158362 ) ) ;
#8128 = CARTESIAN_POINT ( 'NONE',  ( -41.03604514216881682, -295.4331711629549204, -343.3013195127070958 ) ) ;
#8129 = CARTESIAN_POINT ( 'NONE',  ( -97.47530550890830625, -279.9137734892112235, -315.7954604370450511 ) ) ;
#8130 = CARTESIAN_POINT ( 'NONE',  ( -98.17399215065155715, -277.8597449689636392, -223.9422556973289886 ) ) ;
#8131 = TOROIDAL_SURFACE ( 'NONE', #58033, 1.000000000000000000, 0.5000000000000000000 ) ;
#8132 = CARTESIAN_POINT ( 'NONE',  ( 19.96545856242100925, -274.2037152016761183, -219.0071071626609296 ) ) ;
#8133 = CARTESIAN_POINT ( 'NONE',  ( -23.82759904544685270, -280.9579894241214220, -343.5641457005611414 ) ) ;
#8134 = CARTESIAN_POINT ( 'NONE',  ( -88.38035010239748601, -277.7507125657219831, -213.7793486349378611 ) ) ;
#8135 = CARTESIAN_POINT ( 'NONE',  ( 19.69207575226213436, -278.8748759124342200, -221.3805653360641372 ) ) ;
#8136 = ADVANCED_FACE ( 'NONE', ( #24569 ), #18400, .F. ) ;
#8137 = CARTESIAN_POINT ( 'NONE',  ( -100.3107428087508168, -295.7561046765929405, -232.3657085698484366 ) ) ;
#8138 = CARTESIAN_POINT ( 'NONE',  ( -36.30535200196021606, -276.0652672355307686, -195.3556616230930274 ) ) ;
#8139 = CARTESIAN_POINT ( 'NONE',  ( 195.8126787625682539, 24.45293242576443049, 12.34923435822822491 ) ) ;
#8140 = CARTESIAN_POINT ( 'NONE',  ( -103.1608118071919051, -289.0583347044720881, -233.6698201309343403 ) ) ;
#8141 = CARTESIAN_POINT ( 'NONE',  ( -48.86899637170681387, -289.1949671333656511, -346.5473251627266791 ) ) ;
#8142 = CARTESIAN_POINT ( 'NONE',  ( -3.408529488362511461, -276.4991874036045374, -203.2753996071324138 ) ) ;
#8143 = CARTESIAN_POINT ( 'NONE',  ( -97.88107605473174999, -271.1564458993732387, -226.0031569106832876 ) ) ;
#8144 = CARTESIAN_POINT ( 'NONE',  ( -110.0751358337139010, -283.4364597119254086, -295.1402654811672619 ) ) ;
#8145 = FACE_OUTER_BOUND ( 'NONE', #43480, .T. ) ;
#8146 = CARTESIAN_POINT ( 'NONE',  ( 23.93971589769808617, -278.9643665410040967, -227.1004771850872999 ) ) ;
#8147 = CYLINDRICAL_SURFACE ( 'NONE', #60424, 7.999911143031724237 ) ;
#8148 = CARTESIAN_POINT ( 'NONE',  ( -28.04090243351973655, -290.9676184676383741, -197.5046971835992338 ) ) ;
#8149 = CARTESIAN_POINT ( 'NONE',  ( -99.12212090931139130, -283.2536217067654434, -229.2023389870147696 ) ) ;
#8150 = LINE ( 'NONE', #35655, #7894 ) ;
#8151 = CARTESIAN_POINT ( 'NONE',  ( 221.0059830678134460, 1.828427124746190069, -9.000000000000001776 ) ) ;
#8152 = CARTESIAN_POINT ( 'NONE',  ( 5.670939392648947752, -290.6342601277420954, -208.8571153759386902 ) ) ;
#8153 = CARTESIAN_POINT ( 'NONE',  ( -98.29824191064153638, -279.5797322628210395, -311.9632865491652751 ) ) ;
#8154 = CARTESIAN_POINT ( 'NONE',  ( -67.70975448991417522, -284.6469725979753207, -340.6874288034358642 ) ) ;
#8156 = CARTESIAN_POINT ( 'NONE',  ( -91.52122179960639414, -285.2535121589745586, -221.3626210168351065 ) ) ;
#8155 = CARTESIAN_POINT ( 'NONE',  ( -12.36568005723957775, -274.8097769455103503, -341.7287714476520364 ) ) ;
#8157 = CARTESIAN_POINT ( 'NONE',  ( 36.28869640350418990, -276.9933397310216492, -271.5767323975772456 ) ) ;
#8158 = CARTESIAN_POINT ( 'NONE',  ( -66.85845467276556064, -278.2519756885929496, -337.3041006508607325 ) ) ;
#8159 = CARTESIAN_POINT ( 'NONE',  ( -109.9326084848987506, -286.3094202279793308, -289.2682818673715133 ) ) ;
#8160 = EDGE_CURVE ( 'NONE', #2170, #72022, #58227, .T. ) ;
#8161 = ORIENTED_EDGE ( 'NONE', *, *, #86265, .T. ) ;
#8162 = CIRCLE ( 'NONE', #41395, 24.49999999999999645 ) ;
#8163 = CARTESIAN_POINT ( 'NONE',  ( -112.1206950522465462, -270.5523142621871102, -270.3356552556181214 ) ) ;
#8164 = CARTESIAN_POINT ( 'NONE',  ( -92.69847972270899561, -295.6522570676820578, -323.8833279277232009 ) ) ;
#8165 = CARTESIAN_POINT ( 'NONE',  ( 20.81039032277737988, -290.1790772233784992, -317.1604895947701834 ) ) ;
#8166 = DIRECTION ( 'NONE',  ( -0.7071067811864494290, 8.659560562353731078E-17, 0.7071067811866457165 ) ) ;
#8167 = CARTESIAN_POINT ( 'NONE',  ( -72.02372285203398405, -279.9805209788415823, -342.4524372437778652 ) ) ;
#8168 = CARTESIAN_POINT ( 'NONE',  ( -82.04747367213400366, -278.3785845518816586, -208.0483077362997051 ) ) ;
#8169 = CARTESIAN_POINT ( 'NONE',  ( 12.76787395916058365, -291.1376611916884372, -212.9549249512255358 ) ) ;
#8170 = CIRCLE ( 'NONE', #85287, 1.500000000000001332 ) ;
#8171 = CARTESIAN_POINT ( 'NONE',  ( -14.36806484283705920, -287.8754864141963594, -200.2867486383720745 ) ) ;
#8172 = CARTESIAN_POINT ( 'NONE',  ( -110.9086939320789043, -280.2008211621055125, -278.9290772286676088 ) ) ;
#8173 = CARTESIAN_POINT ( 'NONE',  ( 37.97298062650322947, -288.8139260698100657, -257.3883140021017653 ) ) ;
#8174 = CARTESIAN_POINT ( 'NONE',  ( -93.13631810824165314, -285.8538830937043258, -320.4999047093288596 ) ) ;
#8175 = CARTESIAN_POINT ( 'NONE',  ( -69.01343525507078880, -277.6239253166676235, -340.5602870983317985 ) ) ;
#8176 = CARTESIAN_POINT ( 'NONE',  ( -73.62481522715789595, -295.5881481331142595, -205.1278261547325599 ) ) ;
#8177 = CARTESIAN_POINT ( 'NONE',  ( 38.21697244273757832, -291.5957320311709395, -267.5156877626960750 ) ) ;
#8178 = CARTESIAN_POINT ( 'NONE',  ( -112.0854050171260781, -278.6175655975350196, -251.8035534840315961 ) ) ;
#8179 = AXIS2_PLACEMENT_3D ( 'NONE', #70479, #40148, #83246 ) ;
#8180 = CARTESIAN_POINT ( 'NONE',  ( -100.3410428545005004, -274.9454999920176306, -231.0934685075681045 ) ) ;
#8181 = AXIS2_PLACEMENT_3D ( 'NONE', #46720, #18327, #89815 ) ;
#8182 = EDGE_CURVE ( 'NONE', #87518, #58102, #33614, .T. ) ;
#8183 = CARTESIAN_POINT ( 'NONE',  ( -37.37352853689063892, -294.5519495502701943, -195.3611179825600175 ) ) ;
#8184 = CARTESIAN_POINT ( 'NONE',  ( -38.32156247796196169, -272.2798927552709642, -194.3807660033862419 ) ) ;
#8185 = DIRECTION ( 'NONE',  ( 0.000000000000000000, 0.000000000000000000, 1.000000000000000000 ) ) ;
#8186 = CARTESIAN_POINT ( 'NONE',  ( -74.53171740694234870, -279.0509903461343697, -207.4150453568209684 ) ) ;
#8187 = VECTOR ( 'NONE', #47932, 1000.000000000000000 ) ;
#8188 = CARTESIAN_POINT ( 'NONE',  ( 16.68611286523719173, -277.5095746022453795, -324.7399367696779677 ) ) ;
#8189 = CARTESIAN_POINT ( 'NONE',  ( -50.07355810752827807, -299.3117679249257890, -197.8816401418131079 ) ) ;
#8190 = CARTESIAN_POINT ( 'NONE',  ( -67.79905309717629791, -282.5009917377072952, -340.8250794350179831 ) ) ;
#8191 = CARTESIAN_POINT ( 'NONE',  ( 34.69242566093825531, -289.5335162531466722, -287.3628454926237055 ) ) ;
#8192 = CARTESIAN_POINT ( 'NONE',  ( -110.1574025285620451, -298.3635507047486612, -247.3695676159385641 ) ) ;
#8193 = CARTESIAN_POINT ( 'NONE',  ( -9.306518152596988003, -299.6008830229522459, -193.7525902071232906 ) ) ;
#8194 = CARTESIAN_POINT ( 'NONE',  ( 21.99201416585045976, -296.1785539566021725, -315.9840673755689409 ) ) ;
#8195 = CARTESIAN_POINT ( 'NONE',  ( -4.033465500463715436, -280.6116839055916330, -337.3729821306352505 ) ) ;
#8196 = CARTESIAN_POINT ( 'NONE',  ( -72.66429445132308729, -271.6025235429034410, -204.5451790722492262 ) ) ;
#8197 = CARTESIAN_POINT ( 'NONE',  ( 24.87996056931854127, -288.5637787123874318, -226.3510703271207092 ) ) ;
#8198 = VECTOR ( 'NONE', #46, 1000.000000000000114 ) ;
#8199 = EDGE_CURVE ( 'NONE', #69835, #6120, #61050, .T. ) ;
#8200 = CARTESIAN_POINT ( 'NONE',  ( -3.234759334076432236, -287.5112433257053226, -335.3091091258291385 ) ) ;
#8201 = CARTESIAN_POINT ( 'NONE',  ( 191.2182377077906210, 270.1866636230031986, -139.4034682273137093 ) ) ;
#8202 = ORIENTED_EDGE ( 'NONE', *, *, #79416, .F. ) ;
#8203 = CARTESIAN_POINT ( 'NONE',  ( -51.59333685379478140, -287.8057490131084251, -345.4310663107943355 ) ) ;
#8204 = CARTESIAN_POINT ( 'NONE',  ( 14.09526769726614326, -287.9718319416722352, -322.1908954051531850 ) ) ;
#8205 = ORIENTED_EDGE ( 'NONE', *, *, #46440, .T. ) ;
#8206 = CARTESIAN_POINT ( 'NONE',  ( -110.6347129470287598, -285.9184972853026920, -247.6073563475782748 ) ) ;
#8207 = CARTESIAN_POINT ( 'NONE',  ( -90.98049828805513073, -278.1733347450403357, -319.9822838292565166 ) ) ;
#8208 = EDGE_CURVE ( 'NONE', #13153, #31, #3788, .T. ) ;
#8209 = CARTESIAN_POINT ( 'NONE',  ( -2.185239688717064421, -291.4267576358827228, -202.1883777198423502 ) ) ;
#8210 = CARTESIAN_POINT ( 'NONE',  ( 31.92603756300851359, -281.7731774274238887, -236.8426344075677150 ) ) ;
#8211 = CARTESIAN_POINT ( 'NONE',  ( 38.83832826753946676, -283.1383104555060868, -275.5938904056896490 ) ) ;
#8212 = CARTESIAN_POINT ( 'NONE',  ( -4.169101813171855575, -282.9599755698355921, -339.8401485919889069 ) ) ;
#8213 = CARTESIAN_POINT ( 'NONE',  ( -37.01249035395545661, -280.3896690971016596, -197.3407159855634632 ) ) ;
#8214 = CARTESIAN_POINT ( 'NONE',  ( 203.7385753312324255, 295.8239488676054521, -68.68380676480988711 ) ) ;
#8215 = CARTESIAN_POINT ( 'NONE',  ( -67.51919413461016006, -279.4491100218172051, -338.8399270025230408 ) ) ;
#8216 = CARTESIAN_POINT ( 'NONE',  ( 102.1048073347433984, 116.7066834670583688, -282.3738722355800519 ) ) ;
#8217 = CARTESIAN_POINT ( 'NONE',  ( -40.39622826133777522, -139.3177327926281919, -361.3465267510854346 ) ) ;
#8218 = CARTESIAN_POINT ( 'NONE',  ( -48.89086778907831388, -273.0985731122017341, -198.0656734554658556 ) ) ;
#8219 = CARTESIAN_POINT ( 'NONE',  ( 39.65004385586741620, -293.0592443801769491, -270.3162576741946737 ) ) ;
#8220 = CARTESIAN_POINT ( 'NONE',  ( 199.4771156391817044, 285.7106110358174647, -96.36288505241603275 ) ) ;
#8222 = CARTESIAN_POINT ( 'NONE',  ( -109.4487032702568996, -288.7462267643866198, -286.1368280742186130 ) ) ;
#8221 = CARTESIAN_POINT ( 'NONE',  ( -60.70449132435135908, -272.4402049955682514, -197.4534070751128922 ) ) ;
#8223 = CARTESIAN_POINT ( 'NONE',  ( -47.94645742184883375, -297.0487392896868641, -343.8870997488448893 ) ) ;
#8224 = CARTESIAN_POINT ( 'NONE',  ( 31.86941091889186595, -289.1942513318580836, -295.0808587808870698 ) ) ;
#8225 = VERTEX_POINT ( 'NONE', #32625 ) ;
#8226 = CARTESIAN_POINT ( 'NONE',  ( -41.91951042189564447, -296.0496237935923318, -347.0414396277783453 ) ) ;
#8227 = CARTESIAN_POINT ( 'NONE',  ( -72.40905352599041578, -286.0671283506696341, -206.2511077312405803 ) ) ;
#8228 = CARTESIAN_POINT ( 'NONE',  ( -68.70502247561516640, -272.5698384764476145, -200.3622514046079743 ) ) ;
#8229 = CARTESIAN_POINT ( 'NONE',  ( 37.91451346131207600, -294.5494031122284468, -285.8743748071310051 ) ) ;
#8230 = CARTESIAN_POINT ( 'NONE',  ( 26.43837157476315269, -293.4759869089399444, -227.2368466991587184 ) ) ;
#8231 = CARTESIAN_POINT ( 'NONE',  ( -30.80908708362613169, -292.3037082016740555, -197.6540002339139903 ) ) ;
#8232 = ORIENTED_EDGE ( 'NONE', *, *, #29223, .T. ) ;
#8233 = CARTESIAN_POINT ( 'NONE',  ( -1.997142436358078532, -276.4366632153182763, -203.5773142433344844 ) ) ;
#8234 = CARTESIAN_POINT ( 'NONE',  ( 36.20896316335802823, -274.0751114480273145, -248.7674764491355006 ) ) ;
#8235 = ORIENTED_EDGE ( 'NONE', *, *, #69736, .T. ) ;
#8236 = CARTESIAN_POINT ( 'NONE',  ( -103.3555684037344236, -278.5766898961941820, -230.7392407679122073 ) ) ;
#8237 = CARTESIAN_POINT ( 'NONE',  ( -33.98411455798402869, -272.4949557075995585, -196.6375326412457412 ) ) ;
#8238 = CARTESIAN_POINT ( 'NONE',  ( -107.4963497813586883, -273.9143837811582785, -248.9138678115826053 ) ) ;
#8239 = CARTESIAN_POINT ( 'NONE',  ( -51.61902788433417300, -274.8064208554403649, -198.4790382186501745 ) ) ;
#8240 = CARTESIAN_POINT ( 'NONE',  ( -23.56068614086864343, -299.8220829685578792, -194.1574325805405294 ) ) ;
#8241 = CARTESIAN_POINT ( 'NONE',  ( 33.19127283596517941, -273.2293864945604582, -243.8374205445818745 ) ) ;
#8242 = CARTESIAN_POINT ( 'NONE',  ( -100.2499685906837072, -296.6914469935880447, -307.6957334255300225 ) ) ;
#8243 = CARTESIAN_POINT ( 'NONE',  ( 34.34532835409838469, -292.3450716859035197, -287.0401950425402902 ) ) ;
#8244 = DIRECTION ( 'NONE',  ( 0.000000000000000000, 0.000000000000000000, 1.000000000000000000 ) ) ;
#8245 = CARTESIAN_POINT ( 'NONE',  ( 10.49270609881256355, -276.9043465753118198, -330.6902227387937501 ) ) ;
#8246 = CARTESIAN_POINT ( 'NONE',  ( -6.530911435774659601, -274.6351094645378907, -204.1818515564873167 ) ) ;
#8247 = CARTESIAN_POINT ( 'NONE',  ( -103.6049059239891648, -283.7385512346713767, -232.0133426163484671 ) ) ;
#8248 = CARTESIAN_POINT ( 'NONE',  ( -106.1064065531918033, -298.9505159643125580, -239.8770417912992059 ) ) ;
#8249 = DIRECTION ( 'NONE',  ( -1.000000000000000000, 0.000000000000000000, 0.000000000000000000 ) ) ;
#8250 = CARTESIAN_POINT ( 'NONE',  ( -97.48286507373671839, -284.3287431583534044, -228.6779405996006460 ) ) ;
#8251 = VECTOR ( 'NONE', #27083, 1000.000000000000000 ) ;
#8252 = CARTESIAN_POINT ( 'NONE',  ( -98.82303473716640951, -277.3576158127910958, -229.0631199027758385 ) ) ;
#8253 = CARTESIAN_POINT ( 'NONE',  ( -56.77309693657972645, -275.8822281979100808, -341.3914749303068561 ) ) ;
#8254 = CARTESIAN_POINT ( 'NONE',  ( -40.64440112943640315, -285.0938264587467756, -345.3010594970865554 ) ) ;
#8255 = CARTESIAN_POINT ( 'NONE',  ( 36.09638666303445831, -276.7731785992814935, -271.5763092790903102 ) ) ;
#8256 = DIRECTION ( 'NONE',  ( 0.000000000000000000, 0.000000000000000000, 1.000000000000000000 ) ) ;
#8257 = CARTESIAN_POINT ( 'NONE',  ( 36.80861786471962205, -274.1745353556555074, -287.9720487661896868 ) ) ;
#8258 = CARTESIAN_POINT ( 'NONE',  ( -87.72198962451302862, -281.3504217467373678, -214.5771162053004559 ) ) ;
#8259 = CARTESIAN_POINT ( 'NONE',  ( 197.7335303680046650, 24.96166607582781083, 12.00000000000000000 ) ) ;
#8260 = CARTESIAN_POINT ( 'NONE',  ( -77.77297098924006491, -287.4338113103829073, -206.5283165921237583 ) ) ;
#8261 = CARTESIAN_POINT ( 'NONE',  ( 155.5427215445352260, 17.93151222991595262, -8.507834038805324184 ) ) ;
#8262 = CARTESIAN_POINT ( 'NONE',  ( 2.156387640704739095, -290.5804653806386568, -206.5443217577132202 ) ) ;
#8263 = VECTOR ( 'NONE', #42060, 1000.000000000000000 ) ;
#8264 = DIRECTION ( 'NONE',  ( -0.000000000000000000, -0.000000000000000000, -1.000000000000000000 ) ) ;
#8265 = CARTESIAN_POINT ( 'NONE',  ( -84.31726006802928453, -296.1842205489926982, -213.8994950413990921 ) ) ;
#8266 = CARTESIAN_POINT ( 'NONE',  ( -110.9212095917192613, -288.8243750878549463, -260.1358897349019799 ) ) ;
#8267 = CARTESIAN_POINT ( 'NONE',  ( 6.757860130087521178, -59.91093500391586701, -350.7441993381422094 ) ) ;
#8268 = CARTESIAN_POINT ( 'NONE',  ( -35.73738983254033030, -296.0720782082398728, -195.3616562271829764 ) ) ;
#8269 = CARTESIAN_POINT ( 'NONE',  ( -48.78431811421492625, -287.6750899408974078, -345.8584267106271000 ) ) ;
#8270 = CARTESIAN_POINT ( 'NONE',  ( -33.43370511856519300, -284.6023051227076621, -344.0702867015227184 ) ) ;
#8271 = CARTESIAN_POINT ( 'NONE',  ( -64.16819136358799369, -283.9468019447569986, -199.2534442105668404 ) ) ;
#8272 = CARTESIAN_POINT ( 'NONE',  ( 18.06033515703222392, -283.6629337773714497, -318.7965327575103061 ) ) ;
#8273 = CARTESIAN_POINT ( 'NONE',  ( -106.3225653737429894, -285.0294912301480394, -294.8889956474224050 ) ) ;
#8274 = CARTESIAN_POINT ( 'NONE',  ( -88.35899231476878413, -291.7427507734794290, -325.8195952284083319 ) ) ;
#8275 = CARTESIAN_POINT ( 'NONE',  ( -85.79821248650144128, -273.7351768733041126, -210.5471505377111896 ) ) ;
#8276 = CARTESIAN_POINT ( 'NONE',  ( 9.319132046145174542, -286.4969820008562351, -329.8589765446868114 ) ) ;
#8277 = CARTESIAN_POINT ( 'NONE',  ( 16.02703672096978949, -274.7840385955083775, -214.8563620859998196 ) ) ;
#8278 = CARTESIAN_POINT ( 'NONE',  ( 35.82380454034149864, -295.3412768050098407, -255.5741056924946122 ) ) ;
#8279 = CARTESIAN_POINT ( 'NONE',  ( -48.18343439339133027, -263.2279375583058822, -443.0391293176500085 ) ) ;
#8280 = CARTESIAN_POINT ( 'NONE',  ( -4.771743288812468897, -291.1233781216987495, -337.9199732462171255 ) ) ;
#8281 = CARTESIAN_POINT ( 'NONE',  ( -71.65386404591605185, -282.2003801067847917, -335.3528011916450851 ) ) ;
#8282 = CARTESIAN_POINT ( 'NONE',  ( -64.45805579246368211, -275.4049527938127540, -340.5212201520491817 ) ) ;
#8283 = CARTESIAN_POINT ( 'NONE',  ( -92.65611466045429268, -271.7571550717036075, -217.7775872492336475 ) ) ;
#8284 = CARTESIAN_POINT ( 'NONE',  ( 33.33863155232842246, -275.1467891088194619, -289.0207905950664440 ) ) ;
#8285 = CARTESIAN_POINT ( 'NONE',  ( -41.65256892093166385, -293.5171378067259411, -196.7436581752837128 ) ) ;
#8286 = CARTESIAN_POINT ( 'NONE',  ( 4.628708955301119587, -293.5751990842128976, -210.2831850550282411 ) ) ;
#8287 = CARTESIAN_POINT ( 'NONE',  ( -107.9458880956823350, -286.0220183876300553, -292.5652314561752974 ) ) ;
#8288 = CARTESIAN_POINT ( 'NONE',  ( 37.18255999887779240, -294.7640880704538517, -253.4282480202897432 ) ) ;
#8289 = CARTESIAN_POINT ( 'NONE',  ( 29.03939691517057398, -294.3699160090109217, -232.3236597731639677 ) ) ;
#8290 = CARTESIAN_POINT ( 'NONE',  ( -101.4683276015983182, -295.9093519217059907, -305.2434294506728065 ) ) ;
#8291 = CARTESIAN_POINT ( 'NONE',  ( -83.76479713648667769, -291.6896254559972590, -329.2669471489276702 ) ) ;
#8292 = CARTESIAN_POINT ( 'NONE',  ( -113.1365919914083804, -284.5454640079326509, -284.2234378506873895 ) ) ;
#8293 = CARTESIAN_POINT ( 'NONE',  ( 96.03965234238681603, -297.7891995914106928, -194.8443227416307195 ) ) ;
#8294 = CARTESIAN_POINT ( 'NONE',  ( -69.79090538727119508, -285.4699400018363349, -200.5180403070917521 ) ) ;
#8295 = CARTESIAN_POINT ( 'NONE',  ( -104.6024050281223907, -280.1023295313847825, -302.8510595676843877 ) ) ;
#8296 = CARTESIAN_POINT ( 'NONE',  ( -71.34864170662183369, -284.3874575923714474, -205.3176061596872159 ) ) ;
#8297 = CARTESIAN_POINT ( 'NONE',  ( 35.20324031050567726, -285.7965889188588449, -289.3935184728280774 ) ) ;
#8298 = CARTESIAN_POINT ( 'NONE',  ( -42.32477241687654157, -278.1295268111490486, -194.7603608983119727 ) ) ;
#8299 = CARTESIAN_POINT ( 'NONE',  ( 204.6539576904058606, 291.1800221208779931, 7.500000000000000000 ) ) ;
#8300 = CARTESIAN_POINT ( 'NONE',  ( -109.0410930147352104, -283.8747183874442044, -284.4033934928929739 ) ) ;
#8301 = CARTESIAN_POINT ( 'NONE',  ( 14.87936773103877997, -281.9734963913975321, -214.2442732148389837 ) ) ;
#8302 = CARTESIAN_POINT ( 'NONE',  ( -89.34092821436455267, -288.8220770088713039, -326.8314685290400234 ) ) ;
#8303 = CARTESIAN_POINT ( 'NONE',  ( -90.75359746618231327, -279.3940657768375218, -324.7821109420657990 ) ) ;
#8304 = CARTESIAN_POINT ( 'NONE',  ( 0.8157055774802070003, -277.8698426935357020, -336.7334363566346838 ) ) ;
#8305 = CARTESIAN_POINT ( 'NONE',  ( -66.06774586248181436, -279.4987798963685464, -203.2370157507219801 ) ) ;
#8306 = CARTESIAN_POINT ( 'NONE',  ( -91.40490094741399218, -275.2580322838123834, -218.8738074127771256 ) ) ;
#8307 = CARTESIAN_POINT ( 'NONE',  ( 37.76130585578759735, -293.3390465869196078, -253.3155804573571288 ) ) ;
#8308 = CARTESIAN_POINT ( 'NONE',  ( -42.80900180664941246, -287.1414497675957023, -344.8571732011448603 ) ) ;
#8309 = CARTESIAN_POINT ( 'NONE',  ( -106.5425496607384304, -292.5660672429578995, -238.3341873027603981 ) ) ;
#8310 = CARTESIAN_POINT ( 'NONE',  ( 17.30183688811230525, -293.1688335152245486, -319.2503779049449122 ) ) ;
#8311 = CARTESIAN_POINT ( 'NONE',  ( -26.20836917106474928, -294.5732202134387876, -342.5285374217200456 ) ) ;
#8312 = CARTESIAN_POINT ( 'NONE',  ( -113.5048797576731801, -291.5135498281408104, -279.7800091927238668 ) ) ;
#8313 = CARTESIAN_POINT ( 'NONE',  ( 4.975421513624708858, -281.2926752247358877, -210.7527806139052302 ) ) ;
#8314 = ADVANCED_FACE ( 'NONE', ( #68606 ), #28007, .T. ) ;
#8315 = CARTESIAN_POINT ( 'NONE',  ( -3.565874001828468920, -297.3860441556971068, -193.6762481238071416 ) ) ;
#8316 = CARTESIAN_POINT ( 'NONE',  ( -8.263978578098019057, -289.3326826881709053, -341.5638405283590373 ) ) ;
#8317 = CARTESIAN_POINT ( 'NONE',  ( -76.14596299181764039, -281.7040340603282402, -335.4952581766779076 ) ) ;
#8318 = CARTESIAN_POINT ( 'NONE',  ( -43.17645838374929212, -289.4572102199495021, -347.1185273162600993 ) ) ;
#8319 = CARTESIAN_POINT ( 'NONE',  ( 13.15111011125132556, -287.1145974696386247, -217.5413515927343155 ) ) ;
#8320 = CARTESIAN_POINT ( 'NONE',  ( 201.7240241516389574, 293.7293971981536629, -83.18315247025914516 ) ) ;
#8321 = CARTESIAN_POINT ( 'NONE',  ( 63.22103669990880803, 47.92133741242891176, -316.8191042900280081 ) ) ;
#8322 = CARTESIAN_POINT ( 'NONE',  ( -55.60814623013595792, -169.4418122124796753, -360.5495281866856772 ) ) ;
#8323 = CARTESIAN_POINT ( 'NONE',  ( -110.5123360852229837, -277.7818060068988757, -267.8926382502700108 ) ) ;
#8324 = CARTESIAN_POINT ( 'NONE',  ( -107.5190650318384940, -277.7519552007705670, -249.1629216190852105 ) ) ;
#8325 = CARTESIAN_POINT ( 'NONE',  ( -1.307633499101990004, -274.1835922031394830, -202.3369286543063481 ) ) ;
#8326 = CARTESIAN_POINT ( 'NONE',  ( 175.0041629047781271, 240.4131245324038844, -177.6887199834764317 ) ) ;
#8327 = CARTESIAN_POINT ( 'NONE',  ( -113.6445838756358029, -277.0757253824085637, -274.4202094164843402 ) ) ;
#8328 = CARTESIAN_POINT ( 'NONE',  ( -2.413054757375911574, -296.3565715061034780, -337.8441806628794097 ) ) ;
#8329 = CIRCLE ( 'NONE', #61276, 24.00000000000001066 ) ;
#8330 = CARTESIAN_POINT ( 'NONE',  ( 8.882930851629504687, -293.1981947323657778, -213.7157178095656889 ) ) ;
#8331 = CARTESIAN_POINT ( 'NONE',  ( -73.84358200006384720, -274.5211940095080081, -202.7710458423248667 ) ) ;
#8332 = CARTESIAN_POINT ( 'NONE',  ( -0.7604210395519718224, -287.2405917456084694, -334.1617750186446756 ) ) ;
#8333 = CARTESIAN_POINT ( 'NONE',  ( -105.5224101039212172, -273.6642203059287226, -234.6833361348515723 ) ) ;
#8334 = CARTESIAN_POINT ( 'NONE',  ( -84.07646283080694616, -297.5557556038510256, -214.2160486507111727 ) ) ;
#8335 = ORIENTED_EDGE ( 'NONE', *, *, #50291, .T. ) ;
#8336 = CARTESIAN_POINT ( 'NONE',  ( 196.0143093133015384, 250.0000000000000568, -11.99999999999998579 ) ) ;
#8337 = CARTESIAN_POINT ( 'NONE',  ( -110.3461926727412248, -280.7214898202737459, -250.8262824034354708 ) ) ;
#8338 = CARTESIAN_POINT ( 'NONE',  ( -59.84152288778496143, -280.8334954296590809, -200.5366440328770068 ) ) ;
#8339 = CARTESIAN_POINT ( 'NONE',  ( -113.2005444345684992, -280.3681265287311248, -265.9554679596756159 ) ) ;
#8340 = CARTESIAN_POINT ( 'NONE',  ( 19.54630740871675343, -273.3744187275711397, -223.5160290947762576 ) ) ;
#8341 = DIRECTION ( 'NONE',  ( 0.000000000000000000, 1.000000000000000000, 0.000000000000000000 ) ) ;
#8342 = CARTESIAN_POINT ( 'NONE',  ( 204.6539576904058606, 293.9636489450775230, 0.000000000000000000 ) ) ;
#8343 = CARTESIAN_POINT ( 'NONE',  ( -22.19647948440641727, -280.4181250650603943, -198.8976211804902903 ) ) ;
#8344 = CARTESIAN_POINT ( 'NONE',  ( 24.34411847373105431, -275.7445173515255306, -224.5460701886739514 ) ) ;
#8345 = CARTESIAN_POINT ( 'NONE',  ( 13.54539285635240731, -278.3402571773850127, -325.5272365306250322 ) ) ;
#8346 = CARTESIAN_POINT ( 'NONE',  ( -111.6068383973752987, -276.8995921752079994, -288.3963945737141898 ) ) ;
#8347 = ORIENTED_EDGE ( 'NONE', *, *, #81598, .F. ) ;
#8348 = CARTESIAN_POINT ( 'NONE',  ( 140.6539576904058606, 276.0000000000000568, 12.00000000000000000 ) ) ;
#8349 = CARTESIAN_POINT ( 'NONE',  ( 21.26040569712759165, -284.1812917122802560, -317.7544739925014596 ) ) ;
#8350 = CARTESIAN_POINT ( 'NONE',  ( -70.28429003828244959, -290.8035571044527501, -205.0358740298112252 ) ) ;
#8351 = CARTESIAN_POINT ( 'NONE',  ( -18.19937023769119833, -285.6410405840448448, -195.8286810658755428 ) ) ;
#8352 = CARTESIAN_POINT ( 'NONE',  ( -95.08954205613500221, -282.1465896852297419, -316.6755718151316614 ) ) ;
#8354 = CARTESIAN_POINT ( 'NONE',  ( -8.921422392047762884, -284.5066286355018406, -201.5461639253691715 ) ) ;
#8353 = CARTESIAN_POINT ( 'NONE',  ( 5.923989895202256939, -281.0270416693567199, -329.8880445152174730 ) ) ;
#8355 = CARTESIAN_POINT ( 'NONE',  ( -67.48330849950752963, -280.8528163151304966, -203.4249888109294773 ) ) ;
#8356 = DIRECTION ( 'NONE',  ( -0.9393874931428880526, 0.000000000000000000, -0.3428573139466629116 ) ) ;
#8357 = CARTESIAN_POINT ( 'NONE',  ( -4.526998554563204991, -281.0268790313537011, -339.1478018420622789 ) ) ;
#8358 = CARTESIAN_POINT ( 'NONE',  ( -25.20566982056843841, -296.8977247283833094, -344.4253852945511198 ) ) ;
#8359 = CARTESIAN_POINT ( 'NONE',  ( -97.07067353381347630, -278.9032966661787896, -312.7604598173548993 ) ) ;
#8360 = CARTESIAN_POINT ( 'NONE',  ( -65.22161571679001213, -287.6888408989054824, -200.5422930956303276 ) ) ;
#8361 = EDGE_CURVE ( 'NONE', #36764, #61449, #64332, .T. ) ;
#8362 = ADVANCED_FACE ( 'NONE', ( #11305 ), #62694, .F. ) ;
#8363 = CARTESIAN_POINT ( 'NONE',  ( 128.9467878515196162, -299.5541904835127980, -195.3611179825600175 ) ) ;
#8364 = CARTESIAN_POINT ( 'NONE',  ( -2.737519560770817595, -294.4260979987192854, -203.1762019396395544 ) ) ;
#8365 = CARTESIAN_POINT ( 'NONE',  ( 6.547080839558873322, -274.4559378005754411, -331.2427951825577566 ) ) ;
#8366 = CARTESIAN_POINT ( 'NONE',  ( 28.75961725698642013, -287.2608121016148175, -309.5373181568937184 ) ) ;
#8367 = CARTESIAN_POINT ( 'NONE',  ( -9.405963006380487101, -290.8231915656431852, -201.9983542393699736 ) ) ;
#8368 = CARTESIAN_POINT ( 'NONE',  ( -93.99683139834648671, -276.5776266211051393, -317.1936558139399267 ) ) ;
#8369 = CARTESIAN_POINT ( 'NONE',  ( -100.9430361440342381, -295.2109505874921069, -231.9762781301447774 ) ) ;
#8370 = CARTESIAN_POINT ( 'NONE',  ( -109.1962319081563635, -292.0695460811627413, -254.9283689660583150 ) ) ;
#8371 = CARTESIAN_POINT ( 'NONE',  ( 158.6539576904058606, 293.9636489450775230, -11.60392986742922261 ) ) ;
#8372 = CARTESIAN_POINT ( 'NONE',  ( 219.8344101925596021, 35.72494958537217968, 7.000000000000000000 ) ) ;
#8373 = CARTESIAN_POINT ( 'NONE',  ( -93.19529745392752318, -294.3167414348046691, -322.3715539003737831 ) ) ;
#8374 = CARTESIAN_POINT ( 'NONE',  ( 13.67805720154488291, -288.3812406307868059, -216.9668605901659362 ) ) ;
#8375 = CARTESIAN_POINT ( 'NONE',  ( -106.3308848451127204, -289.2063383509611185, -238.3851461425439879 ) ) ;
#8376 = CARTESIAN_POINT ( 'NONE',  ( 33.65517424816048475, -289.2333833429689207, -289.9106266486477921 ) ) ;
#8377 = DIRECTION ( 'NONE',  ( -1.000000000000000000, -0.000000000000000000, -0.000000000000000000 ) ) ;
#8378 = CARTESIAN_POINT ( 'NONE',  ( -26.44075465362175237, -289.7128606397769204, -342.7570880605549064 ) ) ;
#8379 = DIRECTION ( 'NONE',  ( 0.000000000000000000, 1.000000000000000000, 0.000000000000000000 ) ) ;
#8380 = CARTESIAN_POINT ( 'NONE',  ( 0.5363793263533368494, -289.7644264455269649, -337.0037948326392439 ) ) ;
#8381 = CARTESIAN_POINT ( 'NONE',  ( -74.18133490481001502, -277.5851011519008011, -204.6249170475634003 ) ) ;
#8382 = CARTESIAN_POINT ( 'NONE',  ( -8.872877414587117428, -280.7478352631193275, -198.8399992494221635 ) ) ;
#8383 = CARTESIAN_POINT ( 'NONE',  ( -2.395947042261342474, -280.1684228281034166, -201.7567546120976090 ) ) ;
#8384 = PRODUCT_DEFINITION_FORMATION_WITH_SPECIFIED_SOURCE ( 'ANY', '', #15547, .NOT_KNOWN. ) ;
#8385 = CARTESIAN_POINT ( 'NONE',  ( 24.38176773647593976, -286.1298346619964263, -312.9890750372579191 ) ) ;
#8386 = DIRECTION ( 'NONE',  ( -1.000000000000000000, 0.000000000000000000, 0.000000000000000000 ) ) ;
#8387 = CARTESIAN_POINT ( 'NONE',  ( -72.69748089556026116, -277.7182422316141128, -205.0860519294942605 ) ) ;
#8388 = CARTESIAN_POINT ( 'NONE',  ( -75.75599263695316665, -281.5643120534864465, -334.8367351056810435 ) ) ;
#8389 = CARTESIAN_POINT ( 'NONE',  ( 85.24291055932573613, 81.26895824411224112, -298.9807373830735742 ) ) ;
#8390 = CARTESIAN_POINT ( 'NONE',  ( -112.1181239977252346, -276.8393319260856629, -285.6308420171541229 ) ) ;
#8391 = AXIS2_PLACEMENT_3D ( 'NONE', #85547, #6957, #19286 ) ;
#8392 = CARTESIAN_POINT ( 'NONE',  ( -100.7331994143008558, -284.0450582960532415, -227.1047287568084130 ) ) ;
#8393 = CARTESIAN_POINT ( 'NONE',  ( -35.15089380731298263, -299.0214930645661298, -197.1254609449464965 ) ) ;
#8394 = CARTESIAN_POINT ( 'NONE',  ( -108.6235390214026637, -274.3303832631097521, -242.6925605078068031 ) ) ;
#8395 = CARTESIAN_POINT ( 'NONE',  ( 33.91296414719582231, -275.4301550202109752, -286.3823058924789393 ) ) ;
#8396 = CARTESIAN_POINT ( 'NONE',  ( -2.184280600849622278, -296.5868824753964077, -336.6103180035956370 ) ) ;
#8397 = CARTESIAN_POINT ( 'NONE',  ( -37.49945962628935803, -289.2207188155298923, -347.3740282608129064 ) ) ;
#8398 = CARTESIAN_POINT ( 'NONE',  ( 35.94075556086367840, -279.3972474518482727, -251.9492769681368998 ) ) ;
#8399 = CARTESIAN_POINT ( 'NONE',  ( 33.32523746210740967, -292.9957822347540173, -239.7803407506089002 ) ) ;
#8400 = CARTESIAN_POINT ( 'NONE',  ( -92.59712090189616163, -288.9271287212538368, -318.5019460893274186 ) ) ;
#8401 = CARTESIAN_POINT ( 'NONE',  ( 21.55379671925705054, -290.9141717075581823, -223.9043814857781740 ) ) ;
#8402 = VERTEX_POINT ( 'NONE', #5148 ) ;
#8403 = CARTESIAN_POINT ( 'NONE',  ( 198.5371898822048990, 65.94618789579841689, 10.76511267510459824 ) ) ;
#8404 = CARTESIAN_POINT ( 'NONE',  ( -92.59893437561237306, -290.7403210453661018, -222.5633512448363547 ) ) ;
#8405 = CYLINDRICAL_SURFACE ( 'NONE', #30851, 9.550761578869391144 ) ;
#8406 = CARTESIAN_POINT ( 'NONE',  ( -1.091284337424976991, -287.4625440613063461, -202.6948223219712304 ) ) ;
#8407 = CARTESIAN_POINT ( 'NONE',  ( 7.450504543161046378, -296.9090924074130839, -326.4764044574609443 ) ) ;
#8408 = CARTESIAN_POINT ( 'NONE',  ( 26.30992240531349680, -293.1780110962217805, -313.2713867045764573 ) ) ;
#8409 = CARTESIAN_POINT ( 'NONE',  ( -31.65611837700087250, -284.2969967563731188, -346.6695985675668226 ) ) ;
#8410 = CARTESIAN_POINT ( 'NONE',  ( -109.8729977947918286, -284.2707679874577025, -279.0562481778311508 ) ) ;
#8411 = CARTESIAN_POINT ( 'NONE',  ( 25.80781410736804560, -277.3807122431420566, -307.9560954270891671 ) ) ;
#8412 = CARTESIAN_POINT ( 'NONE',  ( 37.28529766639027088, -291.6138401943479153, -273.5845930215531894 ) ) ;
#8413 = CARTESIAN_POINT ( 'NONE',  ( -68.43690893236576755, -272.4292298983943965, -203.8626229172665774 ) ) ;
#8414 = ORIENTED_EDGE ( 'NONE', *, *, #71951, .F. ) ;
#8415 = CARTESIAN_POINT ( 'NONE',  ( -104.9628119525177112, -256.0684274861638983, -326.9234398911233939 ) ) ;
#8416 = CARTESIAN_POINT ( 'NONE',  ( 24.00955426602381948, -293.8384824104831523, -316.8559335633037790 ) ) ;
#8417 = CARTESIAN_POINT ( 'NONE',  ( 20.62134535090654452, -288.8244461877017670, -223.6333331477684396 ) ) ;
#8418 = CARTESIAN_POINT ( 'NONE',  ( -110.0482693383470263, -297.3233503965265641, -294.7588085118717345 ) ) ;
#8419 = CARTESIAN_POINT ( 'NONE',  ( 31.06705521557221417, -287.8584378253083287, -244.4474542360500777 ) ) ;
#8420 = CARTESIAN_POINT ( 'NONE',  ( -104.5816995602165065, -278.0920755391292118, -233.3259632141318036 ) ) ;
#8421 = CARTESIAN_POINT ( 'NONE',  ( -70.75606971522442734, -296.1326914751398931, -339.6344899498650989 ) ) ;
#8422 = CARTESIAN_POINT ( 'NONE',  ( 7.189072363802494259, -286.5926370044257396, -331.7227481071446391 ) ) ;
#8423 = CARTESIAN_POINT ( 'NONE',  ( -16.50852077234483062, -295.1235046919684919, -344.5224964348305434 ) ) ;
#8424 = CARTESIAN_POINT ( 'NONE',  ( -25.40981683922824885, -292.5415750500928311, -198.2699299406296518 ) ) ;
#8425 = LINE ( 'NONE', #65768, #63973 ) ;
#8426 = DIRECTION ( 'NONE',  ( 1.000000000000000000, 0.000000000000000000, 0.000000000000000000 ) ) ;
#8427 = CARTESIAN_POINT ( 'NONE',  ( -107.1748277085172987, -264.8307257489187236, -305.4825756969687518 ) ) ;
#8428 = CARTESIAN_POINT ( 'NONE',  ( 36.01922953829974006, -288.8045206300831182, -249.1764845995975577 ) ) ;
#8429 = CARTESIAN_POINT ( 'NONE',  ( -111.2869819898779866, -281.6237833571633473, -305.9350535429201159 ) ) ;
#8430 = ORIENTED_EDGE ( 'NONE', *, *, #78193, .F. ) ;
#8431 = CARTESIAN_POINT ( 'NONE',  ( -67.31506793197156924, -279.0178491600407824, -199.5450886581959935 ) ) ;
#8432 = CARTESIAN_POINT ( 'NONE',  ( 19.33683420826664090, -282.8732092295673510, -221.4786666618553852 ) ) ;
#8433 = CARTESIAN_POINT ( 'NONE',  ( 191.3098834081771997, 269.0209914007751308, -138.7723537854704148 ) ) ;
#8434 = CARTESIAN_POINT ( 'NONE',  ( -93.47445018655095339, -283.8389138508416067, -218.4403628813092837 ) ) ;
#8435 = CARTESIAN_POINT ( 'NONE',  ( 35.41296738518497023, -285.8364764181033593, -286.1711271937955416 ) ) ;
#8436 = CARTESIAN_POINT ( 'NONE',  ( -31.38124961174612437, -275.9870526523563967, -194.8180655509988242 ) ) ;
#8437 = CARTESIAN_POINT ( 'NONE',  ( -108.2361819950270387, -297.2779933882924297, -252.6474665598731235 ) ) ;
#8438 = CARTESIAN_POINT ( 'NONE',  ( 28.83134217002636746, -292.6681936955410492, -302.4529762751967610 ) ) ;
#8439 = CARTESIAN_POINT ( 'NONE',  ( -109.5134036462223435, -279.5412097394954003, -243.6638293505802721 ) ) ;
#8440 = CARTESIAN_POINT ( 'NONE',  ( 31.26176204935996594, -275.8863599465067864, -295.4592619193037422 ) ) ;
#8441 = CARTESIAN_POINT ( 'NONE',  ( -67.42709771540076247, -274.7463377502214144, -199.8177883026089035 ) ) ;
#8442 = CARTESIAN_POINT ( 'NONE',  ( -68.90078820814900951, -276.3777754378377267, -340.2719358146214859 ) ) ;
#8443 = CARTESIAN_POINT ( 'NONE',  ( 175.2296996224750103, 149.6461846693799487, 0.000000000000000000 ) ) ;
#8444 = CARTESIAN_POINT ( 'NONE',  ( -43.31028530026550527, -275.1272398593608273, -345.1739368166437885 ) ) ;
#8445 = CARTESIAN_POINT ( 'NONE',  ( -113.6442382214117117, -297.9149350527327442, -275.3193654817033007 ) ) ;
#8446 = CARTESIAN_POINT ( 'NONE',  ( -95.99890600148557951, -275.6948066931273615, -223.6242672951989618 ) ) ;
#8447 = CARTESIAN_POINT ( 'NONE',  ( 168.8235619055982113, 230.3815547064285738, -190.2228674158758395 ) ) ;
#8448 = CARTESIAN_POINT ( 'NONE',  ( -96.02159608354469356, -286.2460113764979610, -226.4191575681084885 ) ) ;
#8449 = CARTESIAN_POINT ( 'NONE',  ( -92.67802161734913113, -285.5918050138986928, -322.4557623740048484 ) ) ;
#8450 = CARTESIAN_POINT ( 'NONE',  ( -25.11661920508774415, -285.5606085391307261, -198.2372836293438354 ) ) ;
#8451 = CARTESIAN_POINT ( 'NONE',  ( -95.40780278049497554, -277.5875278856383375, -224.7911629146941266 ) ) ;
#8452 = CARTESIAN_POINT ( 'NONE',  ( -109.2845303047393770, -286.1749746913413901, -288.6667091822764633 ) ) ;
#8453 = CARTESIAN_POINT ( 'NONE',  ( -108.9589396283162728, -277.2590362881911119, -252.9922158627122428 ) ) ;
#8454 = CARTESIAN_POINT ( 'NONE',  ( -54.01091033362814642, -278.3507675604900555, -341.8022966407779109 ) ) ;
#8455 = CARTESIAN_POINT ( 'NONE',  ( 198.0541817046291726, 70.37814311852002902, -10.52985504265800643 ) ) ;
#8456 = CARTESIAN_POINT ( 'NONE',  ( -110.2506496594334919, -273.1162838474767227, -264.9151045739267261 ) ) ;
#8457 = CONICAL_SURFACE ( 'NONE', #71822, 9.550761578869391144, 0.7853981633974327359 ) ;
#8458 = CARTESIAN_POINT ( 'NONE',  ( 38.63349031472916550, -282.2067100469844831, -258.5302816038997094 ) ) ;
#8459 = CARTESIAN_POINT ( 'NONE',  ( 39.12088293316512022, -281.9317231116910989, -261.3509419643702358 ) ) ;
#8460 = ORIENTED_EDGE ( 'NONE', *, *, #28009, .F. ) ;
#8461 = ORIENTED_EDGE ( 'NONE', *, *, #84910, .T. ) ;
#8462 = CARTESIAN_POINT ( 'NONE',  ( 196.4653187812577926, 42.25725872477071476, 13.19426264048105146 ) ) ;
#8463 = CARTESIAN_POINT ( 'NONE',  ( 30.30808499766753883, -288.9664049285214560, -236.2464283276986237 ) ) ;
#8464 = CARTESIAN_POINT ( 'NONE',  ( -106.0778620103985901, -288.8014437903967178, -304.0768052511444921 ) ) ;
#8465 = CARTESIAN_POINT ( 'NONE',  ( -71.73188240598024379, -296.7826183578704331, -205.7719944301186956 ) ) ;
#8466 = CARTESIAN_POINT ( 'NONE',  ( 21.23819028622834537, -292.2280225474484610, -220.5242421328150328 ) ) ;
#8467 = CARTESIAN_POINT ( 'NONE',  ( 34.67767361159377515, -285.8279410744211759, -254.7432576713999310 ) ) ;
#8468 = CARTESIAN_POINT ( 'NONE',  ( 1.608192231784646431, -287.0949351505607297, -332.7973318479549789 ) ) ;
#8469 = CARTESIAN_POINT ( 'NONE',  ( -14.45668811898826789, -287.5604909296918663, -200.5696858399135465 ) ) ;
#8470 = CARTESIAN_POINT ( 'NONE',  ( -112.3841908609287543, -276.5367145900733021, -271.5505799756937790 ) ) ;
#8471 = CARTESIAN_POINT ( 'NONE',  ( 37.63997241300206298, -289.5310266062551250, -268.7029778690200601 ) ) ;
#8472 = CARTESIAN_POINT ( 'NONE',  ( -106.0657691578680470, -288.1525095454317693, -300.9364141708742295 ) ) ;
#8473 = CARTESIAN_POINT ( 'NONE',  ( -91.83212262548094884, -284.7951455964642946, -319.3105709106018821 ) ) ;
#8474 = CARTESIAN_POINT ( 'NONE',  ( -102.2032465073414897, -292.0446285120938796, -308.4509585775351184 ) ) ;
#8475 = CARTESIAN_POINT ( 'NONE',  ( -48.18343439339133027, -283.1093320178187582, -435.6442049081568939 ) ) ;
#8476 = EDGE_CURVE ( 'NONE', #10127, #10282, #49163, .T. ) ;
#8477 = DIRECTION ( 'NONE',  ( 1.000000000000000000, 0.000000000000000000, 0.000000000000000000 ) ) ;
#8478 = CARTESIAN_POINT ( 'NONE',  ( -63.02080052824070577, -275.6992839420630048, -199.5162832753156863 ) ) ;
#8479 = CARTESIAN_POINT ( 'NONE',  ( -11.67694546944097311, -279.5921199740473639, -201.7953349648843187 ) ) ;
#8480 = CARTESIAN_POINT ( 'NONE',  ( 4.485042898639600040, -280.4881251836865772, -332.6776331543525771 ) ) ;
#8481 = CARTESIAN_POINT ( 'NONE',  ( -39.11438272366691393, -294.2710400302972289, -347.1791914907149703 ) ) ;
#8482 = CARTESIAN_POINT ( 'NONE',  ( -89.94686466845699613, -271.5363821796510138, -218.2970163721493293 ) ) ;
#8483 = CARTESIAN_POINT ( 'NONE',  ( -21.36738178200117133, -274.9256816697155728, -343.1199456173536646 ) ) ;
#8484 = CARTESIAN_POINT ( 'NONE',  ( -109.7646638889822128, -298.0310712164553024, -257.8648065737219213 ) ) ;
#8485 = LINE ( 'NONE', #29817, #24717 ) ;
#8486 = CARTESIAN_POINT ( 'NONE',  ( -102.2616301707950157, -294.2695249540354894, -309.8500619489861947 ) ) ;
#8487 = CARTESIAN_POINT ( 'NONE',  ( 36.23181522101855023, -295.0184566641829633, -273.4961155717368797 ) ) ;
#8488 = FACE_OUTER_BOUND ( 'NONE', #40766, .T. ) ;
#8489 = CARTESIAN_POINT ( 'NONE',  ( -18.16836128501384806, -295.6014577201963789, -340.9655428019839292 ) ) ;
#8490 = CARTESIAN_POINT ( 'NONE',  ( 113.5000000000000568, -296.0521521680024080, -537.7509286889328450 ) ) ;
#8492 = CARTESIAN_POINT ( 'NONE',  ( -96.88273702143361277, -297.1419161421789568, -228.1252928377322746 ) ) ;
#8491 = CARTESIAN_POINT ( 'NONE',  ( -40.71700741363184051, -284.0301395286036268, -195.0304658060662462 ) ) ;
#8493 = CARTESIAN_POINT ( 'NONE',  ( -79.15972554674409878, -283.5997481412384218, -335.0159921227520385 ) ) ;
#8494 = CARTESIAN_POINT ( 'NONE',  ( -21.99413509095603558, -284.7771447667798839, -344.3460248394388259 ) ) ;
#8495 = CARTESIAN_POINT ( 'NONE',  ( 21.47012229830211893, -287.8882004341004404, -320.0291543288612957 ) ) ;
#8496 = CARTESIAN_POINT ( 'NONE',  ( 34.39366436981235609, -291.2748186313027645, -248.8735217326230611 ) ) ;
#8497 = CARTESIAN_POINT ( 'NONE',  ( -113.9782757722468745, -277.8136749155742677, -277.3135967240182822 ) ) ;
#8498 = CARTESIAN_POINT ( 'NONE',  ( -85.33152481854862970, -275.1952119285918457, -330.4860931364851808 ) ) ;
#8499 = CARTESIAN_POINT ( 'NONE',  ( -48.18343439339133027, -268.0622923073750030, -498.6988577444290627 ) ) ;
#8500 = CARTESIAN_POINT ( 'NONE',  ( 18.08607435315859036, -285.6649154893116815, -222.2477900817396517 ) ) ;
#8501 = CARTESIAN_POINT ( 'NONE',  ( -108.0767089125435660, -289.8509105964187711, -240.7291919360389727 ) ) ;
#8502 = CARTESIAN_POINT ( 'NONE',  ( -48.18343439339133027, -296.0521521680024080, -507.6442049081570076 ) ) ;
#8503 = CARTESIAN_POINT ( 'NONE',  ( -110.0999810773095788, -279.6797307292029586, -293.8731295310336691 ) ) ;
#8505 = CARTESIAN_POINT ( 'NONE',  ( 35.54122530967838145, -281.1596458456153300, -265.8703868246133766 ) ) ;
#8504 = CARTESIAN_POINT ( 'NONE',  ( -63.71466804734471623, -293.4143918343031032, -340.9505886250406661 ) ) ;
#8506 = CARTESIAN_POINT ( 'NONE',  ( -61.58955177424697069, -295.5252286361533720, -343.4992870877245537 ) ) ;
#8507 = CARTESIAN_POINT ( 'NONE',  ( 28.88151341569323804, -285.1505904973551537, -233.8684258384276404 ) ) ;
#8508 = CARTESIAN_POINT ( 'NONE',  ( -98.62973332764182999, -281.1395390396712060, -227.1317571657514804 ) ) ;
#8509 = CARTESIAN_POINT ( 'NONE',  ( -10.41460458241496490, -293.7506915505009033, -338.4664773442113983 ) ) ;
#8510 = CARTESIAN_POINT ( 'NONE',  ( -33.43817532355726740, -296.1008595978869380, -195.3624401095650853 ) ) ;
#8511 = ORIENTED_EDGE ( 'NONE', *, *, #62646, .F. ) ;
#8512 = CARTESIAN_POINT ( 'NONE',  ( 170.2305261370685798, 214.9910457053126720, -24.90909090909089940 ) ) ;
#8513 = CARTESIAN_POINT ( 'NONE',  ( 30.82662058890845103, -283.9340214632740640, -300.9007367978998104 ) ) ;
#8514 = CARTESIAN_POINT ( 'NONE',  ( -107.6637421984649166, -295.7980334214305458, -290.1802713656869059 ) ) ;
#8515 = LINE ( 'NONE', #80958, #86658 ) ;
#8516 = CARTESIAN_POINT ( 'NONE',  ( -110.4683760289727132, -275.8380690714489560, -287.0191576251351080 ) ) ;
#8517 = CARTESIAN_POINT ( 'NONE',  ( -15.81278041597468409, -273.5207998835425656, -196.5450327971991840 ) ) ;
#8518 = CARTESIAN_POINT ( 'NONE',  ( -102.8463662289646692, -289.9488796982461736, -302.5812781853688875 ) ) ;
#8519 = CARTESIAN_POINT ( 'NONE',  ( -109.2878386642281470, -280.2814157945992406, -254.3514499904401873 ) ) ;
#8520 = CARTESIAN_POINT ( 'NONE',  ( -72.30452460671274650, -275.1819656868574384, -205.3115447985777848 ) ) ;
#8521 = CARTESIAN_POINT ( 'NONE',  ( 19.20369637442949440, -283.8538039479970507, -321.5172843107293374 ) ) ;
#8522 = CARTESIAN_POINT ( 'NONE',  ( -14.16904126558389621, -279.1542827669932763, -200.6643054074703514 ) ) ;
#8523 = CARTESIAN_POINT ( 'NONE',  ( -71.33719196742354995, -279.5012423309570408, -337.2139951600037762 ) ) ;
#8524 = ORIENTED_EDGE ( 'NONE', *, *, #72006, .F. ) ;
#8525 = CARTESIAN_POINT ( 'NONE',  ( -36.93760085196832677, -273.8904336506888058, -193.3491261987479390 ) ) ;
#8526 = CARTESIAN_POINT ( 'NONE',  ( -94.56212658089165757, -293.1349209898801860, -222.7267480702109310 ) ) ;
#8527 = DIRECTION ( 'NONE',  ( -0.000000000000000000, 0.000000000000000000, 1.000000000000000000 ) ) ;
#8528 = CARTESIAN_POINT ( 'NONE',  ( 129.8975571001389540, -299.5541904835127980, -195.3611179825600175 ) ) ;
#8529 = CARTESIAN_POINT ( 'NONE',  ( 38.00600409903060495, -291.7987623753188586, -278.7815107990267620 ) ) ;
#8530 = CARTESIAN_POINT ( 'NONE',  ( -5.275392787371918857, -273.9935598726879675, -204.6986685928319787 ) ) ;
#8531 = CARTESIAN_POINT ( 'NONE',  ( 160.5350683151633291, 250.0000000000000568, 20.22542485937379908 ) ) ;
#8532 = CARTESIAN_POINT ( 'NONE',  ( 34.79080259566576672, -294.7538256067413727, -245.3093311926543265 ) ) ;
#8534 = CARTESIAN_POINT ( 'NONE',  ( -36.39875151458510061, -293.2687978539395885, -193.7510280396973030 ) ) ;
#8533 = CARTESIAN_POINT ( 'NONE',  ( -110.4542110544635705, -280.8376638359844719, -287.0812184334320705 ) ) ;
#8535 = CARTESIAN_POINT ( 'NONE',  ( 34.01424054599034719, -289.2602468523275547, -247.7714660062942187 ) ) ;
#8536 = CARTESIAN_POINT ( 'NONE',  ( 36.84118362251066969, -273.4252965534334407, -260.5159067252370733 ) ) ;
#8537 = CARTESIAN_POINT ( 'NONE',  ( 12.73412476348975986, -278.2678016501989191, -325.5103546945414337 ) ) ;
#8538 = CARTESIAN_POINT ( 'NONE',  ( 21.64969254740626425, -292.2588737147723918, -315.7838498414823221 ) ) ;
#8539 = CARTESIAN_POINT ( 'NONE',  ( -17.34123119427936999, -282.1680077757955019, -197.2838525683130513 ) ) ;
#8540 = ORIENTED_EDGE ( 'NONE', *, *, #48693, .T. ) ;
#8541 = CARTESIAN_POINT ( 'NONE',  ( -32.14843171769513219, -282.6515559556271455, -343.1973551863935654 ) ) ;
#8542 = CARTESIAN_POINT ( 'NONE',  ( -100.0043843694782169, -280.2191986184222401, -226.1470872486226824 ) ) ;
#8543 = CARTESIAN_POINT ( 'NONE',  ( -13.55985214278771167, -281.5450195675607574, -343.1789209173725226 ) ) ;
#8544 = CARTESIAN_POINT ( 'NONE',  ( 19.71038571434487707, -277.1928535865182539, -321.7410865202629680 ) ) ;
#8545 = CARTESIAN_POINT ( 'NONE',  ( 19.37495490397807174, -277.7716300887892658, -321.4289768659267565 ) ) ;
#8546 = CARTESIAN_POINT ( 'NONE',  ( 17.40634833298267736, -284.6948066931273047, -313.9805196606274080 ) ) ;
#8547 = ORIENTED_EDGE ( 'NONE', *, *, #17570, .F. ) ;
#8548 = ORIENTED_EDGE ( 'NONE', *, *, #29467, .T. ) ;
#8549 = CARTESIAN_POINT ( 'NONE',  ( -35.78852967049083844, -300.0717513479477816, -195.3605797401941118 ) ) ;
#8550 = CARTESIAN_POINT ( 'NONE',  ( -107.6958101301144950, -291.9037945579524376, -249.7125039511552416 ) ) ;
#8551 = CARTESIAN_POINT ( 'NONE',  ( -111.9953503259433347, -276.6049358226782715, -267.8278428600737584 ) ) ;
#8552 = CARTESIAN_POINT ( 'NONE',  ( -96.48701543572346395, -291.6639952600055494, -318.0870361192027076 ) ) ;
#8553 = CARTESIAN_POINT ( 'NONE',  ( 12.97932452968493244, -292.1263441446682236, -217.3357736142462784 ) ) ;
#8554 = CARTESIAN_POINT ( 'NONE',  ( 39.28559346629512561, -287.1463276615442624, -277.2737715623856616 ) ) ;
#8555 = DIRECTION ( 'NONE',  ( 0.000000000000000000, -0.000000000000000000, 1.000000000000000000 ) ) ;
#8556 = CARTESIAN_POINT ( 'NONE',  ( -108.7982112931249219, -283.1929420817123173, -251.9109844030388956 ) ) ;
#8557 = CARTESIAN_POINT ( 'NONE',  ( -111.4807276213506952, -292.4732866331131618, -265.6809624300449855 ) ) ;
#8558 = CARTESIAN_POINT ( 'NONE',  ( -110.1026317070394214, -283.1857713856381338, -258.5956585211296215 ) ) ;
#8559 = CARTESIAN_POINT ( 'NONE',  ( -32.95016836994529541, -281.4238135536698451, -196.9992891652491380 ) ) ;
#8560 = ORIENTED_EDGE ( 'NONE', *, *, #77692, .F. ) ;
#8561 = CARTESIAN_POINT ( 'NONE',  ( -100.4802292629586873, -290.9150069585285792, -314.0228443770856188 ) ) ;
#8562 = CARTESIAN_POINT ( 'NONE',  ( 34.12407828448477431, -281.8435774252426427, -255.1149938951859326 ) ) ;
#8563 = CARTESIAN_POINT ( 'NONE',  ( -36.36792057564785097, -290.8590369371053157, -193.7514131717549901 ) ) ;
#8564 = CARTESIAN_POINT ( 'NONE',  ( 39.18753752156337811, -288.4412987802419366, -277.2483964668076055 ) ) ;
#8565 = CARTESIAN_POINT ( 'NONE',  ( 33.80012921578681073, -287.6703157568388178, -240.9240623464333737 ) ) ;
#8566 = CARTESIAN_POINT ( 'NONE',  ( -81.48026296028501747, -285.5989772554643196, -212.2165801858669170 ) ) ;
#8567 = ORIENTED_EDGE ( 'NONE', *, *, #20400, .F. ) ;
#8568 = CARTESIAN_POINT ( 'NONE',  ( 185.4166944662832179, 275.5000000000000568, 23.37680765314684450 ) ) ;
#8569 = CARTESIAN_POINT ( 'NONE',  ( -27.87824375417724809, -296.7937706180347845, -345.5850169843606068 ) ) ;
#8570 = CARTESIAN_POINT ( 'NONE',  ( -86.09403039252175915, -294.3968788215267978, -329.3230426901273518 ) ) ;
#8571 = CARTESIAN_POINT ( 'NONE',  ( -27.00009642510053354, -275.9761725206695928, -342.8625640407503283 ) ) ;
#8572 = ADVANCED_FACE ( 'NONE', ( #49622 ), #42507, .F. ) ;
#8573 = CARTESIAN_POINT ( 'NONE',  ( -20.52926933915206220, -297.6060565333928594, -193.4648508431261007 ) ) ;
#8574 = CARTESIAN_POINT ( 'NONE',  ( 35.16882939122410789, -291.8592658757383447, -257.1405311304141605 ) ) ;
#8575 = CARTESIAN_POINT ( 'NONE',  ( -110.1428868112222403, -294.6175229179860935, -283.7716515658402727 ) ) ;
#8576 = CARTESIAN_POINT ( 'NONE',  ( 9.088221398714868116, -293.9108085946446636, -213.4498648993220513 ) ) ;
#8577 = CARTESIAN_POINT ( 'NONE',  ( 18.70406148533283996, -293.9632502869982318, -223.1054444647598700 ) ) ;
#8578 = DIRECTION ( 'NONE',  ( -0.000000000000000000, 1.000000000000000000, -0.000000000000000000 ) ) ;
#8579 = CARTESIAN_POINT ( 'NONE',  ( 22.55234686636103802, -292.1718727129482431, -315.7784226645349577 ) ) ;
#8580 = CARTESIAN_POINT ( 'NONE',  ( -60.29593098400137308, -299.7548470042601707, -198.9062182013545907 ) ) ;
#8581 = CARTESIAN_POINT ( 'NONE',  ( -58.74648930122697976, -290.2770122978339487, -340.4515322190196684 ) ) ;
#8582 = CARTESIAN_POINT ( 'NONE',  ( -3.130094142473434538, -294.9202725909191827, -334.8719969311759996 ) ) ;
#8583 = CARTESIAN_POINT ( 'NONE',  ( -83.83139389325179991, -279.6663365261928220, -329.7326753621404123 ) ) ;
#8584 = CARTESIAN_POINT ( 'NONE',  ( -31.09719897742591854, -278.8141786934916126, -194.0571780743866555 ) ) ;
#8585 = ORIENTED_EDGE ( 'NONE', *, *, #72108, .F. ) ;
#8586 = CARTESIAN_POINT ( 'NONE',  ( -110.0028304246662429, -272.2185276980334265, -245.1882569914864689 ) ) ;
#8587 = CARTESIAN_POINT ( 'NONE',  ( 28.10978045569169126, -280.1064891649999140, -305.8212065982333456 ) ) ;
#8588 = CARTESIAN_POINT ( 'NONE',  ( -113.4342314520543908, -276.9008974433064623, -274.4067440580694210 ) ) ;
#8589 = CARTESIAN_POINT ( 'NONE',  ( -106.8084080859245404, -276.9258367053010943, -241.6486658152932421 ) ) ;
#8590 = EDGE_CURVE ( 'NONE', #43024, #6020, #40054, .T. ) ;
#8591 = CARTESIAN_POINT ( 'NONE',  ( -41.88219090209978646, -296.6785613736013829, -197.0083578293589994 ) ) ;
#8592 = CYLINDRICAL_SURFACE ( 'NONE', #83655, 1.000000000000000888 ) ;
#8593 = CARTESIAN_POINT ( 'NONE',  ( 165.0427047786672290, 276.0000000000000568, 23.37680765314704701 ) ) ;
#8594 = CARTESIAN_POINT ( 'NONE',  ( -94.39865646931430376, -289.2516887158759573, -221.1183341442224446 ) ) ;
#8595 = CARTESIAN_POINT ( 'NONE',  ( -113.1720195082019842, -290.7193651635979563, -256.9909024753625317 ) ) ;
#8596 = CARTESIAN_POINT ( 'NONE',  ( -27.26805092027870714, -276.1799215185916410, -195.8203715622629772 ) ) ;
#8597 = CARTESIAN_POINT ( 'NONE',  ( -66.25819306634969053, -295.6725654145596991, -201.3403612176760191 ) ) ;
#8598 = CARTESIAN_POINT ( 'NONE',  ( -24.57050823684281937, -282.0904470567856492, -346.1848723641564902 ) ) ;
#8599 = DIRECTION ( 'NONE',  ( 0.000000000000000000, 0.000000000000000000, -1.000000000000000000 ) ) ;
#8600 = CARTESIAN_POINT ( 'NONE',  ( 30.08590757004203908, -279.9861861303398882, -303.3190077482742595 ) ) ;
#8601 = CARTESIAN_POINT ( 'NONE',  ( 175.2296996224750103, 250.0000000000000568, 0.000000000000000000 ) ) ;
#8602 = CARTESIAN_POINT ( 'NONE',  ( -52.43652374490492463, -290.6495580378345380, -198.4808312817270064 ) ) ;
#8603 = CARTESIAN_POINT ( 'NONE',  ( -55.02804012543816725, -283.9620341050729166, -198.2103743442108907 ) ) ;
#8604 = CARTESIAN_POINT ( 'NONE',  ( 104.1964229570258311, -299.5541904835127980, -193.4651424135224147 ) ) ;
#8605 = EDGE_CURVE ( 'NONE', #86359, #36583, #93010, .T. ) ;
#8606 = FACE_BOUND ( 'NONE', #32045, .T. ) ;
#8607 = CARTESIAN_POINT ( 'NONE',  ( 20.02231082032096054, -290.8839164988875154, -222.0457901881875387 ) ) ;
#8608 = CARTESIAN_POINT ( 'NONE',  ( -74.39753248658713858, -279.1539399645397452, -334.1835725237709198 ) ) ;
#8609 = CARTESIAN_POINT ( 'NONE',  ( -99.45744512396487380, -285.1587094193211556, -315.2787817480978561 ) ) ;
#8611 = CARTESIAN_POINT ( 'NONE',  ( -25.14182038879835090, -286.2119169001420005, -198.3364711641547729 ) ) ;
#8610 = CARTESIAN_POINT ( 'NONE',  ( -18.87773257458828269, -272.3677574155432239, -197.0377734563224124 ) ) ;
#8612 = CARTESIAN_POINT ( 'NONE',  ( 36.19168952555523333, -277.0293220700342545, -274.3264308221850456 ) ) ;
#8613 = CARTESIAN_POINT ( 'NONE',  ( -53.98073997701444426, -278.0739732817420986, -341.6576290220816645 ) ) ;
#8614 = CARTESIAN_POINT ( 'NONE',  ( -92.90001816390980593, -285.8494174581897482, -320.7614435924210170 ) ) ;
#8615 = ORIENTED_EDGE ( 'NONE', *, *, #41537, .T. ) ;
#8616 = FACE_OUTER_BOUND ( 'NONE', #22304, .T. ) ;
#8617 = CARTESIAN_POINT ( 'NONE',  ( -110.8004322634721035, -296.0949207064991811, -293.4880331806546110 ) ) ;
#8618 = CARTESIAN_POINT ( 'NONE',  ( -14.07677004862288861, -288.3351825727351638, -199.3802610569312606 ) ) ;
#8619 = LINE ( 'NONE', #17606, #23128 ) ;
#8620 = CARTESIAN_POINT ( 'NONE',  ( -37.30987171927208834, -295.5523547857347353, -190.3611179825600175 ) ) ;
#8621 = CARTESIAN_POINT ( 'NONE',  ( -45.22785470368222605, -278.8749529551315618, -194.0239970231942550 ) ) ;
#8622 = CARTESIAN_POINT ( 'NONE',  ( -73.04069625457167092, -289.9870104868959402, -203.0260799935663556 ) ) ;
#8623 = CARTESIAN_POINT ( 'NONE',  ( -109.6561591126852591, -285.8868621229585187, -284.5500846738510177 ) ) ;
#8624 = CARTESIAN_POINT ( 'NONE',  ( -75.04098038060307374, -281.3031154322780480, -206.6096716857336730 ) ) ;
#8625 = CARTESIAN_POINT ( 'NONE',  ( 29.85324596469640568, -289.4528955526334357, -306.8510135246826849 ) ) ;
#8626 = CARTESIAN_POINT ( 'NONE',  ( 37.01219629029702674, -283.4212380202898771, -260.1525991322405957 ) ) ;
#8627 = CARTESIAN_POINT ( 'NONE',  ( -7.882673134869967235, -276.8433798928666079, -341.5172732836531395 ) ) ;
#8628 = CARTESIAN_POINT ( 'NONE',  ( -98.20968232412593579, -295.1623437260620335, -227.1530684139967491 ) ) ;
#8629 = CARTESIAN_POINT ( 'NONE',  ( -86.80309730374099786, -279.2196916953470804, -211.2783179846476571 ) ) ;
#8630 = CARTESIAN_POINT ( 'NONE',  ( -58.33382395624661143, -299.6988598215668844, -198.9423184080384601 ) ) ;
#8631 = CARTESIAN_POINT ( 'NONE',  ( 197.1659783536655937, 296.4152130614111798, -7.628516150743300805 ) ) ;
#8632 = CARTESIAN_POINT ( 'NONE',  ( -54.49178911615187815, -294.3376638359846424, -195.3683826091709363 ) ) ;
#8633 = CARTESIAN_POINT ( 'NONE',  ( -21.54330697732822131, -272.4918891999190009, -196.0349127440500752 ) ) ;
#8634 = DIRECTION ( 'NONE',  ( 0.000000000000000000, 0.000000000000000000, -1.000000000000000000 ) ) ;
#8635 = CARTESIAN_POINT ( 'NONE',  ( -108.0305307688355470, -278.3040167540164020, -251.8437045672945942 ) ) ;
#8636 = CARTESIAN_POINT ( 'NONE',  ( 34.83205540677287360, -277.0846484153361189, -296.1877306781838683 ) ) ;
#8637 = CARTESIAN_POINT ( 'NONE',  ( -74.17366008294015955, -282.5877494812569921, -337.7719499203433884 ) ) ;
#8638 = CARTESIAN_POINT ( 'NONE',  ( -18.18997404698201947, -290.5622206765494298, -341.9069929114824617 ) ) ;
#8639 = CARTESIAN_POINT ( 'NONE',  ( -3.809375465612989231, -299.9848854821569262, -194.0459541100681236 ) ) ;
#8640 = CARTESIAN_POINT ( 'NONE',  ( -108.5253362119391483, -298.1196808925650998, -241.9183460448227834 ) ) ;
#8641 = CARTESIAN_POINT ( 'NONE',  ( -39.72247161212852973, -297.0822525065316881, -345.1693177223515931 ) ) ;
#8642 = CARTESIAN_POINT ( 'NONE',  ( 34.71812903033746522, -279.8122422826048137, -290.5455042772341017 ) ) ;
#8643 = CARTESIAN_POINT ( 'NONE',  ( 8.357346866369255167, -272.7013091175344357, -211.3404105707781468 ) ) ;
#8644 = CARTESIAN_POINT ( 'NONE',  ( -105.9675634679459506, -286.5816652309669621, -237.2411648689164565 ) ) ;
#8645 = CARTESIAN_POINT ( 'NONE',  ( 3.776662570077772063, -287.4049043132056909, -331.1142189481298033 ) ) ;
#8646 = CARTESIAN_POINT ( 'NONE',  ( 162.7515160168861428, 219.2654253216233542, -204.9874331692004432 ) ) ;
#8647 = ORIENTED_EDGE ( 'NONE', *, *, #11869, .T. ) ;
#8648 = CARTESIAN_POINT ( 'NONE',  ( 36.21224550453401747, -286.3888206581659688, -291.1074510879297463 ) ) ;
#8649 = CARTESIAN_POINT ( 'NONE',  ( -63.83252280476894924, -289.0739064444559858, -338.4618027553802904 ) ) ;
#8650 = ORIENTED_EDGE ( 'NONE', *, *, #84782, .F. ) ;
#8651 = CARTESIAN_POINT ( 'NONE',  ( -78.36875182783701632, -286.5934641132845968, -205.5670323099561188 ) ) ;
#8652 = CARTESIAN_POINT ( 'NONE',  ( 22.29564931330443045, -275.2971930838963317, -228.2031003941001757 ) ) ;
#8653 = CARTESIAN_POINT ( 'NONE',  ( -7.298571768429359174, -291.3573588888247627, -199.7855107588698615 ) ) ;
#8654 = CARTESIAN_POINT ( 'NONE',  ( 38.77155861461756814, -282.3407936067129640, -281.3194312715824594 ) ) ;
#8655 = CARTESIAN_POINT ( 'NONE',  ( 38.59024674462135351, -283.1740488553423347, -278.4258361406720610 ) ) ;
#8656 = CARTESIAN_POINT ( 'NONE',  ( 11.48246731664224107, -282.7297812828086876, -329.9443407566290034 ) ) ;
#8657 = CARTESIAN_POINT ( 'NONE',  ( 34.08498995237063411, -281.6845371941750500, -255.1254107772410009 ) ) ;
#8658 = CARTESIAN_POINT ( 'NONE',  ( -20.25526795762938548, -274.3380690714490697, -345.3683826091709648 ) ) ;
#8659 = CARTESIAN_POINT ( 'NONE',  ( -95.38918660201169075, -240.2644329508013357, -341.8810175719231097 ) ) ;
#8660 = ORIENTED_EDGE ( 'NONE', *, *, #28307, .T. ) ;
#8661 = CARTESIAN_POINT ( 'NONE',  ( -26.73715559290007704, -278.9171112223259001, -344.4392663105000452 ) ) ;
#8662 = CARTESIAN_POINT ( 'NONE',  ( 4.645253263068006788, -57.92935080797366254, -354.0998759884595302 ) ) ;
#8663 = CARTESIAN_POINT ( 'NONE',  ( 101.6986848688134586, 115.4960904796168393, -279.9121412288012039 ) ) ;
#8664 = CARTESIAN_POINT ( 'NONE',  ( -110.3135459398219922, -295.9581595143036452, -266.0019452707307437 ) ) ;
#8665 = CARTESIAN_POINT ( 'NONE',  ( 36.64671156940783447, -292.7945491653310341, -249.2123443802435929 ) ) ;
#8666 = CARTESIAN_POINT ( 'NONE',  ( 26.38539103948928499, -24.50260877297474948, -341.6991638436127232 ) ) ;
#8668 = CARTESIAN_POINT ( 'NONE',  ( -76.30824931387375898, -287.9825075597531736, -333.0352630439224413 ) ) ;
#8667 = CARTESIAN_POINT ( 'NONE',  ( -99.43208137315983208, -295.7216227387097547, -225.8258415100113723 ) ) ;
#8669 = CARTESIAN_POINT ( 'NONE',  ( -53.39376664352313639, -297.1205017808284197, -342.8929181222869715 ) ) ;
#8670 = CARTESIAN_POINT ( 'NONE',  ( 8.299210339719618190, -289.7275113414931980, -327.9645099680136013 ) ) ;
#8671 = ORIENTED_EDGE ( 'NONE', *, *, #12784, .F. ) ;
#8672 = CARTESIAN_POINT ( 'NONE',  ( -34.85023741128619434, -295.9628159430980645, -347.0853829001013082 ) ) ;
#8673 = CARTESIAN_POINT ( 'NONE',  ( -74.75700363222532019, -286.0317908867681354, -207.6069666827362425 ) ) ;
#8674 = CARTESIAN_POINT ( 'NONE',  ( -98.76481319911852097, -295.9593143616284578, -224.5657682304249363 ) ) ;
#8675 = CARTESIAN_POINT ( 'NONE',  ( -37.80433812347801847, -292.8493236978347909, -193.5239864155846305 ) ) ;
#8676 = CARTESIAN_POINT ( 'NONE',  ( 37.03868280770084453, -294.2910009028161085, -290.0356074990441471 ) ) ;
#8677 = CARTESIAN_POINT ( 'NONE',  ( -109.2771301956596943, -290.8865011739408715, -257.6509473832102799 ) ) ;
#8678 = ORIENTED_EDGE ( 'NONE', *, *, #608, .T. ) ;
#8679 = DIRECTION ( 'NONE',  ( 0.000000000000000000, 0.000000000000000000, 1.000000000000000000 ) ) ;
#8680 = CARTESIAN_POINT ( 'NONE',  ( -38.36294310990003709, -275.9595924577715209, -194.8080156985693066 ) ) ;
#8681 = CARTESIAN_POINT ( 'NONE',  ( 32.65071107476301648, -274.7464654801361235, -301.4910246883414402 ) ) ;
#8682 = ORIENTED_EDGE ( 'NONE', *, *, #9521, .T. ) ;
#8683 = EDGE_CURVE ( 'NONE', #15791, #85642, #28371, .T. ) ;
#8684 = CARTESIAN_POINT ( 'NONE',  ( -65.07874458106763882, -276.9125228242414778, -342.1821386233470434 ) ) ;
#8685 = CARTESIAN_POINT ( 'NONE',  ( -43.52910050740107550, -272.3726998332504650, -196.7696826814672306 ) ) ;
#8686 = CARTESIAN_POINT ( 'NONE',  ( -46.07656276909249016, -275.3035396841446527, -344.1321212506566667 ) ) ;
#8687 = CARTESIAN_POINT ( 'NONE',  ( -54.29631431284116161, -274.9088878367037410, -199.0395424918422691 ) ) ;
#8688 = CARTESIAN_POINT ( 'NONE',  ( -93.96792944599680197, -274.1493470417372578, -223.8992986894124897 ) ) ;
#8689 = CARTESIAN_POINT ( 'NONE',  ( -100.3805962421122331, -274.8797411425118185, -227.8401535387212675 ) ) ;
#8690 = CARTESIAN_POINT ( 'NONE',  ( -84.75339119934942289, -271.4223757795686538, -211.7903202288688931 ) ) ;
#8691 = CARTESIAN_POINT ( 'NONE',  ( -66.08558870448167966, -296.0899854878438759, -337.5748185049633321 ) ) ;
#8692 = CARTESIAN_POINT ( 'NONE',  ( 24.91614604700444957, -292.6656620354552842, -309.6911681145660395 ) ) ;
#8693 = DIRECTION ( 'NONE',  ( -1.000000000000000000, 0.000000000000000000, -5.880589007913310608E-16 ) ) ;
#8694 = CARTESIAN_POINT ( 'NONE',  ( -68.98433154738133055, -277.9495398045638694, -340.5058945935911652 ) ) ;
#8695 = CARTESIAN_POINT ( 'NONE',  ( 35.64286128180913948, -275.6990291148887309, -268.8598517539333557 ) ) ;
#8696 = CARTESIAN_POINT ( 'NONE',  ( -110.2209199239085251, -282.9419378392214526, -293.6834746463918009 ) ) ;
#8697 = CARTESIAN_POINT ( 'NONE',  ( -105.4931686752748305, -298.1365789482953232, -302.0692519284278319 ) ) ;
#8698 = FACE_OUTER_BOUND ( 'NONE', #73906, .T. ) ;
#8699 = CARTESIAN_POINT ( 'NONE',  ( -42.67572212288514777, -285.1803338228510825, -197.3816916267900865 ) ) ;
#8700 = EDGE_CURVE ( 'NONE', #32853, #8064, #59421, .T. ) ;
#8701 = EDGE_CURVE ( 'NONE', #20790, #57747, #14610, .T. ) ;
#8702 = CARTESIAN_POINT ( 'NONE',  ( -110.9718130055678103, -276.8962461782848550, -262.3493589867784408 ) ) ;
#8703 = CARTESIAN_POINT ( 'NONE',  ( -45.99525885316750617, -275.7386132035457535, -343.4908149029940319 ) ) ;
#8704 = CARTESIAN_POINT ( 'NONE',  ( -111.2793011175721034, -286.7147948671331505, -257.7066023417874021 ) ) ;
#8705 = CARTESIAN_POINT ( 'NONE',  ( -21.86518396271576137, -275.4600181604830027, -198.6142856413370623 ) ) ;
#8706 = DIRECTION ( 'NONE',  ( -0.000000000000000000, -0.000000000000000000, -1.000000000000000000 ) ) ;
#8707 = CARTESIAN_POINT ( 'NONE',  ( 38.52290734758198454, -273.8549722713872825, -262.6814432798924486 ) ) ;
#8708 = CARTESIAN_POINT ( 'NONE',  ( -97.13388025945299376, -281.1745431911787136, -224.7888128637086709 ) ) ;
#8709 = DIRECTION ( 'NONE',  ( -0.000000000000000000, -0.000000000000000000, 1.000000000000000000 ) ) ;
#8710 = CARTESIAN_POINT ( 'NONE',  ( -65.36643516044743762, -287.6088473957584597, -200.1765167969331003 ) ) ;
#8711 = FILL_AREA_STYLE ('',( #22463 ) ) ;
#8712 = CARTESIAN_POINT ( 'NONE',  ( -73.02013669791863038, -289.5792140193086652, -204.3766296577742025 ) ) ;
#8713 = CARTESIAN_POINT ( 'NONE',  ( 82.14177983934591509, -300.1103622902044208, -197.2983025311162066 ) ) ;
#8714 = CARTESIAN_POINT ( 'NONE',  ( -91.47451648554300618, -271.9458055172195827, -220.6345298867763631 ) ) ;
#8715 = CARTESIAN_POINT ( 'NONE',  ( -84.59740556197802164, -289.5326553064027166, -213.1093600932679806 ) ) ;
#8716 = CARTESIAN_POINT ( 'NONE',  ( -112.8392349625790274, -266.9846182459017427, -270.2902299390011081 ) ) ;
#8717 = DIRECTION ( 'NONE',  ( 0.4995866236608238475, 0.04065491159389757192, -0.8653094149623422604 ) ) ;
#8718 = CARTESIAN_POINT ( 'NONE',  ( -4.647837540224855957, -287.1091599749095167, -339.3234098850159057 ) ) ;
#8719 = CARTESIAN_POINT ( 'NONE',  ( -100.1461425751381142, -283.3646982768908629, -227.4946649935920391 ) ) ;
#8720 = CARTESIAN_POINT ( 'NONE',  ( -105.7106420440656933, -290.8952156425477256, -244.6308149921879078 ) ) ;
#8721 = CARTESIAN_POINT ( 'NONE',  ( 22.58284863146822019, -282.3855036991515135, -227.6478486870835525 ) ) ;
#8722 = EDGE_CURVE ( 'NONE', #19459, #80899, #30756, .T. ) ;
#8723 = CARTESIAN_POINT ( 'NONE',  ( 34.49083719769880929, -282.1714070554660907, -256.4139442942782239 ) ) ;
#8724 = CARTESIAN_POINT ( 'NONE',  ( -90.42165271232587997, -291.7784773398208813, -323.9221152937140573 ) ) ;
#8725 = CARTESIAN_POINT ( 'NONE',  ( -34.76156588297511263, -298.2502992953101284, -193.3610472403868243 ) ) ;
#8726 = ORIENTED_EDGE ( 'NONE', *, *, #56813, .T. ) ;
#8727 = CARTESIAN_POINT ( 'NONE',  ( -79.75296315849625728, -287.7000329597065047, -332.9591212113024881 ) ) ;
#8728 = CARTESIAN_POINT ( 'NONE',  ( -1.301494443111259391, -274.5168195144583478, -202.3162535607312691 ) ) ;
#8729 = CARTESIAN_POINT ( 'NONE',  ( -34.82655734279133952, -294.0638002857967876, -195.7586993748782902 ) ) ;
#8730 = CYLINDRICAL_SURFACE ( 'NONE', #13741, 1.000000000000000888 ) ;
#8731 = CARTESIAN_POINT ( 'NONE',  ( -20.25526795762937127, -276.7662352645559167, -195.3538533559490702 ) ) ;
#8732 = CARTESIAN_POINT ( 'NONE',  ( -51.12670898422591392, -281.9167209665001224, -342.6018041981239435 ) ) ;
#8733 = CARTESIAN_POINT ( 'NONE',  ( -112.3791529965137101, -276.6084302471541605, -265.9555429921563814 ) ) ;
#8734 = DIRECTION ( 'NONE',  ( -0.000000000000000000, -1.000000000000000000, -0.000000000000000000 ) ) ;
#8735 = CARTESIAN_POINT ( 'NONE',  ( -36.17886483558234545, -296.4663592219857264, -194.1614229672849206 ) ) ;
#8736 = CARTESIAN_POINT ( 'NONE',  ( 20.91313319842510410, -275.5204868133725427, -314.5229460991500900 ) ) ;
#8737 = CARTESIAN_POINT ( 'NONE',  ( 19.87194822981332010, -294.4210761875629032, -223.8943565759877004 ) ) ;
#8738 = CARTESIAN_POINT ( 'NONE',  ( -62.89401960208366660, -292.6523717872654515, -201.7281272448653908 ) ) ;
#8739 = CARTESIAN_POINT ( 'NONE',  ( -95.77064682945967888, -286.9438338828415453, -224.9089101291104100 ) ) ;
#8740 = CARTESIAN_POINT ( 'NONE',  ( 39.01871031866595274, -295.0123809232335361, -273.1349254321697231 ) ) ;
#8741 = CARTESIAN_POINT ( 'NONE',  ( 38.12264967627783108, -295.0267536753127615, -283.0275053719837501 ) ) ;
#8742 = CARTESIAN_POINT ( 'NONE',  ( -58.41026653058792562, -295.1655507889832393, -340.2547193651718658 ) ) ;
#8743 = CARTESIAN_POINT ( 'NONE',  ( 37.54808777759830463, -289.4890081764498859, -265.4305154974574066 ) ) ;
#8744 = CARTESIAN_POINT ( 'NONE',  ( -113.5990700524482548, -284.5807002303261584, -281.4059909135083331 ) ) ;
#8745 = CARTESIAN_POINT ( 'NONE',  ( -43.15412129400511532, -296.0592921269231965, -194.9727899944366527 ) ) ;
#8746 = CARTESIAN_POINT ( 'NONE',  ( -102.9191899554285925, -283.8580215166877565, -310.7169457208166818 ) ) ;
#8747 = CARTESIAN_POINT ( 'NONE',  ( -98.21270316857264504, -279.9417691240291219, -313.5871004770190780 ) ) ;
#8748 = CARTESIAN_POINT ( 'NONE',  ( -87.95729433502280870, -284.1198129014680944, -217.2085815685039165 ) ) ;
#8749 = CARTESIAN_POINT ( 'NONE',  ( 36.69635282843014323, -285.7097769775011784, -282.6498183180680144 ) ) ;
#8750 = CARTESIAN_POINT ( 'NONE',  ( -76.82821360252853538, -277.6693978044604023, -205.6388062164121493 ) ) ;
#8751 = CARTESIAN_POINT ( 'NONE',  ( -107.3349855510151656, -256.5393008024622077, -313.9713749062190686 ) ) ;
#8752 = CARTESIAN_POINT ( 'NONE',  ( -95.00176195320742067, -284.6917100414731294, -225.4709301275851487 ) ) ;
#8753 = CARTESIAN_POINT ( 'NONE',  ( 28.93531533436184944, -282.2551111191983750, -231.9506254171920716 ) ) ;
#8754 = CARTESIAN_POINT ( 'NONE',  ( 0.5925549777742314950, -287.6184451414697492, -337.1580722811984288 ) ) ;
#8755 = CARTESIAN_POINT ( 'NONE',  ( -35.70801684808192533, -278.6321335968947324, -346.5565930846804008 ) ) ;
#8756 = CARTESIAN_POINT ( 'NONE',  ( -79.93762903577183465, -278.9301144844627629, -333.9771067792736972 ) ) ;
#8757 = CARTESIAN_POINT ( 'NONE',  ( -108.2891668587348022, -278.6122591604276977, -253.1722562099525931 ) ) ;
#8758 = CARTESIAN_POINT ( 'NONE',  ( 18.49961812233036440, -276.8390932206337425, -220.7507943679397044 ) ) ;
#8759 = CARTESIAN_POINT ( 'NONE',  ( 30.89892398482169611, -293.0906787496973607, -234.5781795128535236 ) ) ;
#8760 = CARTESIAN_POINT ( 'NONE',  ( 34.84375156129817697, -285.8085040057915194, -290.2835716721302788 ) ) ;
#8761 = CARTESIAN_POINT ( 'NONE',  ( -56.01269552987617573, -293.4158586769929116, -196.4295796115042947 ) ) ;
#8762 = CARTESIAN_POINT ( 'NONE',  ( -31.59176960551908664, -293.8983255112391362, -343.4947136604575348 ) ) ;
#8763 = CARTESIAN_POINT ( 'NONE',  ( -18.21904986708069885, -294.4655268256878458, -340.8338909781096504 ) ) ;
#8764 = CARTESIAN_POINT ( 'NONE',  ( -53.33831859497281158, -292.9314303861448252, -195.3028325744306528 ) ) ;
#8765 = CARTESIAN_POINT ( 'NONE',  ( 25.65107458195391388, -282.7135141998683139, -307.5529823898622794 ) ) ;
#8766 = EDGE_CURVE ( 'NONE', #46489, #88967, #57675, .T. ) ;
#8767 = CARTESIAN_POINT ( 'NONE',  ( -105.3947844530108426, -272.0718114215542300, -234.7272850809890485 ) ) ;
#8768 = CARTESIAN_POINT ( 'NONE',  ( 25.45706201712810213, -287.6152167461628437, -225.9579244848563064 ) ) ;
#8769 = CARTESIAN_POINT ( 'NONE',  ( -48.86163953578493846, -289.5281946450620012, -346.5270388850194081 ) ) ;
#8771 = CARTESIAN_POINT ( 'NONE',  ( 9.040652902875526920, -287.0427918944928933, -213.9628483815318418 ) ) ;
#8770 = VECTOR ( 'NONE', #47401, 1000.000000000000000 ) ;
#8772 = PLANE ( 'NONE',  #50500 ) ;
#8773 = CARTESIAN_POINT ( 'NONE',  ( 151.8583176937316068, 206.6135508955686078, -215.5781253388939263 ) ) ;
#8774 = CARTESIAN_POINT ( 'NONE',  ( 196.0033876829498070, 282.0444326092349456, -110.2343316263346225 ) ) ;
#8775 = CARTESIAN_POINT ( 'NONE',  ( -1.399799699311389034, -275.7600219461334063, -334.1427038040458228 ) ) ;
#8776 = CARTESIAN_POINT ( 'NONE',  ( -103.4155531380339852, -277.0432582185592878, -302.2350717642920586 ) ) ;
#8777 = CARTESIAN_POINT ( 'NONE',  ( -94.12679818157711509, -272.9261527909770280, -218.3686165279408442 ) ) ;
#8778 = CARTESIAN_POINT ( 'NONE',  ( -75.53332942106331416, -209.1016162018847240, -354.5739361953594653 ) ) ;
#8779 = CARTESIAN_POINT ( 'NONE',  ( -101.6913368279449656, -276.6894594216915380, -311.8392469835088150 ) ) ;
#8780 = CARTESIAN_POINT ( 'NONE',  ( 32.49423713272408776, -295.7003341314283489, -300.4426475121769613 ) ) ;
#8781 = CARTESIAN_POINT ( 'NONE',  ( -7.250624518972343502, -292.9501922423569908, -203.7839776825608169 ) ) ;
#8782 = CARTESIAN_POINT ( 'NONE',  ( -62.80120326237123862, -298.5318025517080969, -197.8630316601054631 ) ) ;
#8783 = CARTESIAN_POINT ( 'NONE',  ( -72.61013518624845631, -288.2143746204559989, -334.8388735834182626 ) ) ;
#8784 = CARTESIAN_POINT ( 'NONE',  ( -26.22707059741377833, -298.6801596957266156, -193.4217551796634496 ) ) ;
#8785 = CARTESIAN_POINT ( 'NONE',  ( -90.04733525985048459, -297.4484094351386716, -219.7802008165302254 ) ) ;
#8786 = ORIENTED_EDGE ( 'NONE', *, *, #78611, .F. ) ;
#8787 = DIRECTION ( 'NONE',  ( 0.9998346970812741485, 0.000000000000000000, -0.01818181818182024179 ) ) ;
#8788 = CARTESIAN_POINT ( 'NONE',  ( -98.28127178982454382, -281.0771087560849537, -225.6662065153367678 ) ) ;
#8789 = CARTESIAN_POINT ( 'NONE',  ( -91.53455490465863420, -280.3367473239707692, -220.9914859695152813 ) ) ;
#8790 = CARTESIAN_POINT ( 'NONE',  ( -94.43441569393428381, -279.6246213802590432, -320.5048697812906653 ) ) ;
#8791 = CARTESIAN_POINT ( 'NONE',  ( -38.06997183454770095, -272.5227396771578583, -196.6713807399352731 ) ) ;
#8792 = DIRECTION ( 'NONE',  ( 0.000000000000000000, 0.000000000000000000, 1.000000000000000000 ) ) ;
#8793 = CARTESIAN_POINT ( 'NONE',  ( 152.4536156746142410, 250.5000000000000568, -12.49999999999999289 ) ) ;
#8794 = CARTESIAN_POINT ( 'NONE',  ( -69.74220494141258087, -279.7799096825131073, -204.9316220995302160 ) ) ;
#8795 = CARTESIAN_POINT ( 'NONE',  ( 39.54591934718346380, -276.3649922940036845, -271.1597390275266548 ) ) ;
#8796 = CARTESIAN_POINT ( 'NONE',  ( 34.16371971671559038, -277.8442825702844630, -292.9879954013105134 ) ) ;
#8797 = CARTESIAN_POINT ( 'NONE',  ( -104.4666875413394820, -276.6508195428239674, -306.8692315493541400 ) ) ;
#8798 = ORIENTED_EDGE ( 'NONE', *, *, #42527, .T. ) ;
#8799 = FACE_OUTER_BOUND ( 'NONE', #26686, .T. ) ;
#8800 = CARTESIAN_POINT ( 'NONE',  ( 37.24687449644227399, -283.6690582316879841, -281.0826541780784851 ) ) ;
#8801 = CARTESIAN_POINT ( 'NONE',  ( -34.84154728004926938, -291.2815254128081506, -197.2423723484104698 ) ) ;
#8802 = CARTESIAN_POINT ( 'NONE',  ( 37.62212644343407675, -286.6854549103712770, -253.1638780941509594 ) ) ;
#8803 = CARTESIAN_POINT ( 'NONE',  ( -69.46902822664068822, -281.7207405807442910, -337.0520136108823408 ) ) ;
#8805 = CARTESIAN_POINT ( 'NONE',  ( 17.97679359525062992, -284.9324314844240575, -220.5306518247968199 ) ) ;
#8804 = CARTESIAN_POINT ( 'NONE',  ( -71.69994364539020637, -282.0902996228408028, -335.4371198632049982 ) ) ;
#8806 = CARTESIAN_POINT ( 'NONE',  ( 25.46818044768311395, -282.2361618086653152, -232.2883337444480674 ) ) ;
#8807 = CARTESIAN_POINT ( 'NONE',  ( 5.216658706816619251, -58.13088329177625013, -354.5881770784516220 ) ) ;
#8808 = CARTESIAN_POINT ( 'NONE',  ( 19.17630823742029023, -280.6540638180429710, -321.5475374455423321 ) ) ;
#8809 = CARTESIAN_POINT ( 'NONE',  ( -9.116443863000283088, -296.6833939340781967, -339.9023675921752670 ) ) ;
#8810 = CARTESIAN_POINT ( 'NONE',  ( -94.52759281103743660, -278.5611422399646813, -315.9186369926540578 ) ) ;
#8811 = CARTESIAN_POINT ( 'NONE',  ( -99.49526654323518926, -287.1243932118238718, -227.9966482142457664 ) ) ;
#8812 = CARTESIAN_POINT ( 'NONE',  ( -17.03751392358046601, -294.2324725654883082, -197.5802536154615154 ) ) ;
#8813 = CARTESIAN_POINT ( 'NONE',  ( 37.34335267491378829, -273.6401488032504403, -277.2272329538114946 ) ) ;
#8814 = EDGE_CURVE ( 'NONE', #10408, #37463, #89190, .T. ) ;
#8815 = CARTESIAN_POINT ( 'NONE',  ( -78.05952675160035881, -288.7814817325821082, -335.5861958324853163 ) ) ;
#8816 = CARTESIAN_POINT ( 'NONE',  ( 19.10145958894884544, -291.2838839168877598, -222.8152439431893299 ) ) ;
#8817 = CARTESIAN_POINT ( 'NONE',  ( -48.18343439339132317, -274.0269255681727145, -431.9367980400547253 ) ) ;
#8818 = CARTESIAN_POINT ( 'NONE',  ( -110.6493762780347083, -277.3053443508624696, -265.1430633173523006 ) ) ;
#8819 = CARTESIAN_POINT ( 'NONE',  ( -88.96802036710012374, -295.4573042168419761, -216.9453142737689291 ) ) ;
#8820 = CARTESIAN_POINT ( 'NONE',  ( -68.95503579391693449, -290.7920145428935257, -336.7074855378030520 ) ) ;
#8821 = LINE ( 'NONE', #1729, #15468 ) ;
#8822 = DIRECTION ( 'NONE',  ( -0.000000000000000000, -0.000000000000000000, -1.000000000000000000 ) ) ;
#8823 = CARTESIAN_POINT ( 'NONE',  ( 37.10319471813262737, -292.2442045832531221, -287.1731007256407793 ) ) ;
#8824 = CARTESIAN_POINT ( 'NONE',  ( 20.96026054497454183, -288.5218459346884856, -225.1137777390445649 ) ) ;
#8825 = CARTESIAN_POINT ( 'NONE',  ( -79.01963551630201721, -289.7387365723944868, -206.7614420887572919 ) ) ;
#8826 = CARTESIAN_POINT ( 'NONE',  ( 36.13983601538115664, -288.9142125528392171, -265.5300800589415076 ) ) ;
#8827 = ADVANCED_FACE ( 'NONE', ( #53218 ), #76107, .T. ) ;
#8828 = CARTESIAN_POINT ( 'NONE',  ( 209.1374487190023501, 30.94653725228601715, 14.00000000000000000 ) ) ;
#8829 = CARTESIAN_POINT ( 'NONE',  ( 3.713658600522237840, -289.2871051723014375, -330.9784599611290332 ) ) ;
#8830 = CARTESIAN_POINT ( 'NONE',  ( -0.2467297892711489415, -296.5413047835233442, -335.9684294254646488 ) ) ;
#8831 = CARTESIAN_POINT ( 'NONE',  ( -43.18343439339132317, -283.1093320178187582, -502.6442049081569508 ) ) ;
#8832 = VECTOR ( 'NONE', #60146, 1000.000000000000000 ) ;
#8833 = CARTESIAN_POINT ( 'NONE',  ( -71.71447333732866980, -290.7013379670577820, -338.8192890217146669 ) ) ;
#8834 = CARTESIAN_POINT ( 'NONE',  ( -85.72884325207586187, -277.4067713215529807, -212.5255641192478038 ) ) ;
#8835 = CARTESIAN_POINT ( 'NONE',  ( -113.6966930768198978, -279.0128603038735946, -260.1748714753144895 ) ) ;
#8836 = CARTESIAN_POINT ( 'NONE',  ( -73.75189508746018419, -279.2490262573203381, -202.5225623299791664 ) ) ;
#8837 = CARTESIAN_POINT ( 'NONE',  ( -46.95670227955788789, -283.9300092139282583, -195.9278233555905899 ) ) ;
#8838 = DIRECTION ( 'NONE',  ( 0.000000000000000000, 0.000000000000000000, 1.000000000000000000 ) ) ;
#8839 = CARTESIAN_POINT ( 'NONE',  ( 19.80184082204314677, -279.0307227091901723, -222.9548719994163548 ) ) ;
#8840 = CARTESIAN_POINT ( 'NONE',  ( -68.38257587989305364, -281.4597367734060072, -338.6500801736776793 ) ) ;
#8841 = CARTESIAN_POINT ( 'NONE',  ( 169.7306087885279169, 250.0000000000000568, -24.89999999999998792 ) ) ;
#8842 = CARTESIAN_POINT ( 'NONE',  ( -113.0268343713029111, -277.1597560483435814, -260.2404540504937245 ) ) ;
#8843 = CARTESIAN_POINT ( 'NONE',  ( -106.8689884798507563, -274.2955077142498794, -246.2503093870082012 ) ) ;
#8844 = CARTESIAN_POINT ( 'NONE',  ( -97.32998023095191797, -284.1147755196226967, -222.5814281366277498 ) ) ;
#8845 = CARTESIAN_POINT ( 'NONE',  ( -110.5035570052937004, -273.3907877843992082, -267.6414315660219359 ) ) ;
#8846 = CARTESIAN_POINT ( 'NONE',  ( -95.59038497043366078, -274.6493756253075276, -220.8869774345099017 ) ) ;
#8847 = CARTESIAN_POINT ( 'NONE',  ( -19.01573596297292568, -276.4763902001100178, -341.0452500356694259 ) ) ;
#8848 = CARTESIAN_POINT ( 'NONE',  ( 4.965005543248443232, -296.4805289413608875, -332.2896518079440966 ) ) ;
#8849 = CARTESIAN_POINT ( 'NONE',  ( -102.3001188250270843, -290.1757706292937087, -311.8041704862518486 ) ) ;
#8850 = CARTESIAN_POINT ( 'NONE',  ( -71.82736713252313621, -277.6798704602044836, -203.1154033255956506 ) ) ;
#8851 = CARTESIAN_POINT ( 'NONE',  ( -107.7322323306574674, -289.9856949406647573, -301.7040101081535681 ) ) ;
#8852 = CARTESIAN_POINT ( 'NONE',  ( -34.58110174421783967, -288.0755005284748904, -343.5941064689160953 ) ) ;
#8853 = CARTESIAN_POINT ( 'NONE',  ( 0.7080000526884929757, -290.5589297708508525, -205.6703330189166365 ) ) ;
#8854 = ORIENTED_EDGE ( 'NONE', *, *, #7938, .F. ) ;
#8855 = CARTESIAN_POINT ( 'NONE',  ( 197.5215339232793497, 69.56983351252434034, 11.61569241699052668 ) ) ;
#8856 = CARTESIAN_POINT ( 'NONE',  ( -108.7694091725905423, -290.2623174363489511, -254.9965215831203693 ) ) ;
#8857 = CARTESIAN_POINT ( 'NONE',  ( 175.2296996224750103, 161.0000000000000853, 9.550761578869391144 ) ) ;
#8858 = CARTESIAN_POINT ( 'NONE',  ( -26.66572345227279683, -287.1259050288720687, -194.2890767046102098 ) ) ;
#8859 = CARTESIAN_POINT ( 'NONE',  ( -6.998514795304313196, -294.9805209788416391, -207.2794874003663779 ) ) ;
#8860 = CARTESIAN_POINT ( 'NONE',  ( -33.45876391898881508, -294.0631770539525291, -347.0406373393321360 ) ) ;
#8861 = CARTESIAN_POINT ( 'NONE',  ( 36.71866745073334215, -283.1090817045886752, -289.5538308758492576 ) ) ;
#8862 = CARTESIAN_POINT ( 'NONE',  ( -44.02226279016083765, -285.7986538926571143, -197.6674450321480094 ) ) ;
#8863 = CARTESIAN_POINT ( 'NONE',  ( 35.10900311050138356, -276.7047319330010851, -257.9520013652513626 ) ) ;
#8864 = CARTESIAN_POINT ( 'NONE',  ( 36.34153764730793057, -291.4171529309782045, -258.3383596302508636 ) ) ;
#8865 = CARTESIAN_POINT ( 'NONE',  ( 20.17619755686089889, -273.7068011220162589, -224.7469019056188131 ) ) ;
#8866 = ORIENTED_EDGE ( 'NONE', *, *, #27281, .F. ) ;
#8867 = CARTESIAN_POINT ( 'NONE',  ( 121.1498776811041438, 150.0802918209077177, -263.8330885344481658 ) ) ;
#8868 = CARTESIAN_POINT ( 'NONE',  ( 34.43024595411311140, -293.5715544377029005, -298.1915338441905305 ) ) ;
#8869 = CARTESIAN_POINT ( 'NONE',  ( 28.92919003607481798, -289.0192275503286510, -236.3435088388247607 ) ) ;
#8870 = CARTESIAN_POINT ( 'NONE',  ( -104.9874654316503921, -298.1018962433801107, -234.1161284526125996 ) ) ;
#8871 = CARTESIAN_POINT ( 'NONE',  ( 15.09684731903779031, -287.4681782359988347, -219.4288942946917302 ) ) ;
#8872 = CARTESIAN_POINT ( 'NONE',  ( -105.9598608242558839, -278.0562936677613948, -235.8281145685863578 ) ) ;
#8873 = CARTESIAN_POINT ( 'NONE',  ( -34.97187626212824085, -292.7325605633918144, -193.4864427115071805 ) ) ;
#8874 = CARTESIAN_POINT ( 'NONE',  ( 26.11635329509505965, -285.1391090912272830, -228.9681121035368676 ) ) ;
#8875 = CARTESIAN_POINT ( 'NONE',  ( 21.35428108204349584, -294.5569597582612005, -320.1659980786425308 ) ) ;
#8876 = CARTESIAN_POINT ( 'NONE',  ( -77.27026606787596563, -291.8335902719472301, -209.2235917918601729 ) ) ;
#8877 = CARTESIAN_POINT ( 'NONE',  ( 212.3569123273291268, -142.7221692137691775, -10.75739200365177695 ) ) ;
#8878 = DIRECTION ( 'NONE',  ( 1.000000000000000000, 0.000000000000000000, 0.000000000000000000 ) ) ;
#8879 = CARTESIAN_POINT ( 'NONE',  ( 189.5630867785912983, 267.9798697569148658, -137.6296589467733611 ) ) ;
#8880 = CARTESIAN_POINT ( 'NONE',  ( 38.28551502962600495, -288.9440476537624249, -260.2007990974250333 ) ) ;
#8881 = CARTESIAN_POINT ( 'NONE',  ( 25.18497378105905682, -291.6952119285918457, -320.2651865833026363 ) ) ;
#8882 = VERTEX_POINT ( 'NONE', #7018 ) ;
#8883 = EDGE_CURVE ( 'NONE', #4350, #82047, #24343, .T. ) ;
#8884 = CARTESIAN_POINT ( 'NONE',  ( -89.12232278051294543, -282.7215225026916414, -322.3264413919608842 ) ) ;
#8885 = CARTESIAN_POINT ( 'NONE',  ( -114.3565631923106025, -278.2392709018845380, -268.7304571307972765 ) ) ;
#8886 = CARTESIAN_POINT ( 'NONE',  ( -3.541737745414301308, -282.4994331406393826, -203.5816871522339113 ) ) ;
#8887 = CARTESIAN_POINT ( 'NONE',  ( -10.80946628091583506, -93.01466741719902132, -358.5508527417753726 ) ) ;
#8888 = EDGE_CURVE ( 'NONE', #15166, #65093, #21683, .T. ) ;
#8889 = CARTESIAN_POINT ( 'NONE',  ( -64.32202481136863526, -284.2816168551030955, -198.8581214070207182 ) ) ;
#8890 = CARTESIAN_POINT ( 'NONE',  ( 35.89309306655286491, -285.7594006460940932, -284.8670212524891667 ) ) ;
#8891 = CARTESIAN_POINT ( 'NONE',  ( -29.98280919162694147, -276.0047682608227433, -194.9545386671636891 ) ) ;
#8892 = CARTESIAN_POINT ( 'NONE',  ( -92.79520295629198756, -297.7212822135711008, -222.7719506575992057 ) ) ;
#8893 = CARTESIAN_POINT ( 'NONE',  ( 31.03828969269414628, -292.5963944860451988, -297.4339066869242743 ) ) ;
#8894 = CARTESIAN_POINT ( 'NONE',  ( -114.1095749408321041, -279.2595770265206170, -265.8882907956013923 ) ) ;
#8895 = CARTESIAN_POINT ( 'NONE',  ( 35.35400940667743441, -275.6399870532713408, -277.0194822890528599 ) ) ;
#8896 = CARTESIAN_POINT ( 'NONE',  ( -109.8142680483750411, -273.9493332498915379, -245.2768717625827151 ) ) ;
#8897 = CARTESIAN_POINT ( 'NONE',  ( -98.56499441528772820, -276.8547046792191964, -316.5692621096710013 ) ) ;
#8898 = DIRECTION ( 'NONE',  ( 0.7071067811864494290, 0.000000000000000000, 0.7071067811866457165 ) ) ;
#8899 = CARTESIAN_POINT ( 'NONE',  ( -21.34504598263349351, -274.8469608215774542, -343.6878356007484854 ) ) ;
#8900 = CARTESIAN_POINT ( 'NONE',  ( -110.2563722018130363, -298.2687163366159666, -247.3370227819160334 ) ) ;
#8901 = CARTESIAN_POINT ( 'NONE',  ( 210.1640492649794396, 37.84931640281016030, 12.09245862095555601 ) ) ;
#8902 = AXIS2_PLACEMENT_3D ( 'NONE', #60794, #17703, #46556 ) ;
#8903 = DIRECTION ( 'NONE',  ( 0.000000000000000000, 1.000000000000000000, 0.000000000000000000 ) ) ;
#8904 = CARTESIAN_POINT ( 'NONE',  ( -59.02650409185191194, -284.4189734439064523, -340.4430138669884514 ) ) ;
#8905 = CARTESIAN_POINT ( 'NONE',  ( -63.54131630630689642, -285.1491385968288910, -341.6882104878432642 ) ) ;
#8906 = CARTESIAN_POINT ( 'NONE',  ( -79.36110500714751481, -284.8169325023645797, -210.4804006476250606 ) ) ;
#8907 = CARTESIAN_POINT ( 'NONE',  ( -107.0262733061681928, -276.6304648514791893, -294.8164459674502496 ) ) ;
#8908 = CARTESIAN_POINT ( 'NONE',  ( -109.6226419287274467, -286.1924071183014462, -287.3378962287779359 ) ) ;
#8909 = CARTESIAN_POINT ( 'NONE',  ( -91.79622016618665725, -277.7373736914510687, -220.7081925858389013 ) ) ;
#8910 = CARTESIAN_POINT ( 'NONE',  ( 30.56955190731863325, -277.0017030970631140, -298.1058157186008657 ) ) ;
#8911 = CYLINDRICAL_SURFACE ( 'NONE', #66977, 1.000000000000000888 ) ;
#8912 = CARTESIAN_POINT ( 'NONE',  ( -85.35532082060400683, -273.8599807757759095, -215.2239030790885010 ) ) ;
#8913 = CARTESIAN_POINT ( 'NONE',  ( 20.93693692956661678, -281.6774159029168345, -220.2635816944431610 ) ) ;
#8914 = CARTESIAN_POINT ( 'NONE',  ( -27.37385590155814086, -283.4212073084198664, -346.7044687932805118 ) ) ;
#8915 = ORIENTED_EDGE ( 'NONE', *, *, #22733, .T. ) ;
#8916 = EDGE_LOOP ( 'NONE', ( #62121, #48444, #85753, #28821 ) ) ;
#8917 = LINE ( 'NONE', #55761, #51880 ) ;
#8918 = CARTESIAN_POINT ( 'NONE',  ( 31.57840887707521205, -289.0022579166670198, -238.7654938221631937 ) ) ;
#8919 = CARTESIAN_POINT ( 'NONE',  ( -102.9174208145260394, -295.3091681613669834, -302.9167584809586629 ) ) ;
#8920 = CARTESIAN_POINT ( 'NONE',  ( -34.95525496102173690, -291.4299447735451736, -193.4869571376665078 ) ) ;
#8921 = CARTESIAN_POINT ( 'NONE',  ( 34.96067494489496141, -286.2190965345413360, -284.6766792354404743 ) ) ;
#8922 = CARTESIAN_POINT ( 'NONE',  ( -8.000108060882192618, -287.2349262631291822, -337.9022211624149463 ) ) ;
#8923 = CARTESIAN_POINT ( 'NONE',  ( -77.27791800869859173, -286.7089660836688836, -208.7197317341725125 ) ) ;
#8924 = CARTESIAN_POINT ( 'NONE',  ( -96.37098770878827736, -275.9170559299510614, -316.6271299238869119 ) ) ;
#8925 = CARTESIAN_POINT ( 'NONE',  ( -51.55625700102394404, -287.6309210686104620, -345.2235704297799543 ) ) ;
#8926 = CARTESIAN_POINT ( 'NONE',  ( -31.07697561381440110, -288.1314472800266344, -195.6102673928900231 ) ) ;
#8927 = CARTESIAN_POINT ( 'NONE',  ( -12.84584470881603302, -286.7344887958782351, -341.4788733514471915 ) ) ;
#8928 = CARTESIAN_POINT ( 'NONE',  ( -38.87803493658780241, -284.0131123915988383, -343.5928279372172938 ) ) ;
#8929 = CARTESIAN_POINT ( 'NONE',  ( -66.33245954898512764, -293.6736317099993130, -201.0100956657519760 ) ) ;
#8930 = DIRECTION ( 'NONE',  ( -1.000000000000000000, 0.000000000000000000, 0.000000000000000000 ) ) ;
#8931 = DIRECTION ( 'NONE',  ( 0.4467993836324665735, -0.8946341770721976117, 0.000000000000000000 ) ) ;
#8932 = CARTESIAN_POINT ( 'NONE',  ( -79.83577301879198274, -299.4029969769662785, -207.8196567918878941 ) ) ;
#8933 = CARTESIAN_POINT ( 'NONE',  ( 2.801108927935374027, -279.8028150310561273, -209.1353286392399866 ) ) ;
#8934 = CARTESIAN_POINT ( 'NONE',  ( 37.56211254831914914, -279.6007446379072690, -274.1584186785586894 ) ) ;
#8935 = CARTESIAN_POINT ( 'NONE',  ( 13.28174368073900702, -293.5626728369923057, -328.2367227466242525 ) ) ;
#8936 = CARTESIAN_POINT ( 'NONE',  ( 96.24762458268381238, -298.1514505501566532, -196.5983225616837728 ) ) ;
#8937 = CARTESIAN_POINT ( 'NONE',  ( -26.84210556344882903, -274.9974281247644967, -344.0569300070972076 ) ) ;
#8938 = CARTESIAN_POINT ( 'NONE',  ( 1.846868788303968278, -295.8314366739548404, -332.5945397804495656 ) ) ;
#8939 = CARTESIAN_POINT ( 'NONE',  ( 189.4188515237862589, 293.9636489450775798, -40.00000000000000711 ) ) ;
#8940 = CARTESIAN_POINT ( 'NONE',  ( -35.51950419750271237, -272.6492990649188073, -193.9590454354158737 ) ) ;
#8941 = CARTESIAN_POINT ( 'NONE',  ( -113.1085082524981260, -294.8734690861882086, -263.9335632844120596 ) ) ;
#8942 = CARTESIAN_POINT ( 'NONE',  ( -15.39997310808768027, -296.1879093892999890, -340.6567011795976327 ) ) ;
#8943 = CARTESIAN_POINT ( 'NONE',  ( 156.8934089303672295, 250.0000000000000568, 16.24901362097164537 ) ) ;
#8944 = CARTESIAN_POINT ( 'NONE',  ( -86.59114713265333307, -296.5606627246945095, -324.4637398811782987 ) ) ;
#8945 = DIRECTION ( 'NONE',  ( -0.000000000000000000, -1.000000000000000000, -0.000000000000000000 ) ) ;
#8947 = CARTESIAN_POINT ( 'NONE',  ( -108.1749450250722191, -296.7857258490046206, -252.6562906329563134 ) ) ;
#8946 = CARTESIAN_POINT ( 'NONE',  ( -51.83176867698495727, -283.8878783882207699, -196.3589601016375923 ) ) ;
#8948 = CARTESIAN_POINT ( 'NONE',  ( -113.4874264431697100, -284.6995975975067381, -258.5715010272343193 ) ) ;
#8949 = CARTESIAN_POINT ( 'NONE',  ( 28.02831123012526149, -282.9700742869529790, -232.4655270653493915 ) ) ;
#8950 = CARTESIAN_POINT ( 'NONE',  ( -104.0200194314797670, -284.7202859603532943, -231.7876577858365863 ) ) ;
#8951 = CARTESIAN_POINT ( 'NONE',  ( -106.8245585493610719, -288.1875797782519157, -298.2880949520864533 ) ) ;
#8952 = CARTESIAN_POINT ( 'NONE',  ( 35.77081079830085031, -279.2666405000204009, -287.0812184334320705 ) ) ;
#8953 = CARTESIAN_POINT ( 'NONE',  ( 16.34609039726634450, -285.5196583220530897, -220.1542502294403505 ) ) ;
#8954 = EDGE_CURVE ( 'NONE', #65891, #13595, #89658, .T. ) ;
#8955 = CARTESIAN_POINT ( 'NONE',  ( -112.8314841097673167, -289.3017874062621786, -283.9551682165991338 ) ) ;
#8956 = DIRECTION ( 'NONE',  ( 0.000000000000000000, 0.000000000000000000, -1.000000000000000000 ) ) ;
#8957 = CARTESIAN_POINT ( 'NONE',  ( -111.1750721578119396, -298.1735020312980851, -268.7353858335342238 ) ) ;
#8958 = CARTESIAN_POINT ( 'NONE',  ( -111.2528298213950961, -279.7323183535153248, -289.7967852478623172 ) ) ;
#8960 = CARTESIAN_POINT ( 'NONE',  ( 13.35283445964067717, -280.4516989608321182, -217.7344739335650843 ) ) ;
#8959 = CARTESIAN_POINT ( 'NONE',  ( -6.494570443607216248, -292.6691636014465416, -339.1132917389062982 ) ) ;
#8961 = CARTESIAN_POINT ( 'NONE',  ( -53.28717320853930062, -295.4177453959280228, -345.7465435217305298 ) ) ;
#8962 = CARTESIAN_POINT ( 'NONE',  ( -65.32097911435121773, -283.7691591568415674, -200.1583840204513365 ) ) ;
#8963 = CARTESIAN_POINT ( 'NONE',  ( -106.6737622213088770, -280.9255136201136338, -241.7592681813426623 ) ) ;
#8965 = CARTESIAN_POINT ( 'NONE',  ( -82.51433374258961351, -294.7450277702720882, -328.0698767542548353 ) ) ;
#8964 = AXIS2_PLACEMENT_3D ( 'NONE', #59774, #74900, #31800 ) ;
#8966 = CARTESIAN_POINT ( 'NONE',  ( -93.69472774365132750, -271.2420196176707350, -220.6181314724049685 ) ) ;
#8967 = ORIENTED_EDGE ( 'NONE', *, *, #45431, .T. ) ;
#8968 = CARTESIAN_POINT ( 'NONE',  ( 208.6208076322478746, 32.98517505407394168, 9.000000000000001776 ) ) ;
#8969 = CARTESIAN_POINT ( 'NONE',  ( 31.86880984511438442, -283.8982011302159094, -298.3209482664706229 ) ) ;
#8970 = CARTESIAN_POINT ( 'NONE',  ( -97.23741703219596388, -295.4769168562332879, -312.1999939029255415 ) ) ;
#8971 = PLANE ( 'NONE',  #54959 ) ;
#8972 = CARTESIAN_POINT ( 'NONE',  ( -37.37352853689063181, -280.5523547857346784, -345.3611179825600175 ) ) ;
#8973 = CARTESIAN_POINT ( 'NONE',  ( -49.68320502573006081, -273.0958948290449939, -194.4665000897131790 ) ) ;
#8974 = ADVANCED_FACE ( 'NONE', ( #75020 ), #50560, .F. ) ;
#8975 = CARTESIAN_POINT ( 'NONE',  ( -93.43847437855436056, -291.0484244716171816, -223.6280952983300949 ) ) ;
#8976 = CARTESIAN_POINT ( 'NONE',  ( -98.58045777634879414, -280.6373498300529832, -229.2762995188936941 ) ) ;
#8977 = CARTESIAN_POINT ( 'NONE',  ( -8.678730652493355180, -276.0335845328903588, -202.3001930762216318 ) ) ;
#8978 = CARTESIAN_POINT ( 'NONE',  ( 37.36529517251588572, -283.3419686120200254, -285.3712902237767821 ) ) ;
#8979 = CARTESIAN_POINT ( 'NONE',  ( -30.20860283698491600, -278.9391794219854432, -197.2608520877612364 ) ) ;
#8980 = CARTESIAN_POINT ( 'NONE',  ( -81.99013534660765856, -279.6609526058850861, -330.6231946009731359 ) ) ;
#8981 = ORIENTED_EDGE ( 'NONE', *, *, #74020, .T. ) ;
#8982 = CARTESIAN_POINT ( 'NONE',  ( -31.25794847127400544, -273.9602837596399354, -193.5885507151284344 ) ) ;
#8983 = CARTESIAN_POINT ( 'NONE',  ( 7.525080303610641508, -294.5898577112423595, -210.9617391248979175 ) ) ;
#8984 = FACE_OUTER_BOUND ( 'NONE', #61925, .T. ) ;
#8985 = LINE ( 'NONE', #89443, #85958 ) ;
#8986 = CARTESIAN_POINT ( 'NONE',  ( -33.57666512363037015, -290.2386593933031804, -194.6899213923076388 ) ) ;
#8987 = CARTESIAN_POINT ( 'NONE',  ( -57.90667237330372785, -297.4457873953132889, -200.2956528570652495 ) ) ;
#8988 = CARTESIAN_POINT ( 'NONE',  ( 194.7510731661265595, -164.3527196417747689, 21.50000000000000000 ) ) ;
#8989 = CARTESIAN_POINT ( 'NONE',  ( -35.00124913942655525, -293.6011288634526295, -194.0773181972479335 ) ) ;
#8990 = CARTESIAN_POINT ( 'NONE',  ( 31.98288692825981272, -284.4805209788416960, -303.7098442033569654 ) ) ;
#8991 = EDGE_CURVE ( 'NONE', #2063, #10842, #91378, .T. ) ;
#8992 = CARTESIAN_POINT ( 'NONE',  ( 14.38895274998998630, -288.7812082887159022, -216.2159241868751849 ) ) ;
#8993 = CARTESIAN_POINT ( 'NONE',  ( -5.519584758828873561, -274.6324594877216327, -338.1054399271781676 ) ) ;
#8994 = CARTESIAN_POINT ( 'NONE',  ( 19.42202864065373902, -278.1437641275746842, -318.5191214375342952 ) ) ;
#8995 = CARTESIAN_POINT ( 'NONE',  ( 28.77655579912167383, -291.1759152057372830, -236.1603807368060473 ) ) ;
#8996 = CARTESIAN_POINT ( 'NONE',  ( -22.82641289902340986, -282.0962551499732172, -195.9463751759451213 ) ) ;
#8997 = VERTEX_POINT ( 'NONE', #57220 ) ;
#8998 = CARTESIAN_POINT ( 'NONE',  ( -3.615388837699111235, -282.2609237244788005, -335.1410392491600874 ) ) ;
#8999 = CARTESIAN_POINT ( 'NONE',  ( -113.9030652395410641, -279.6877662628817802, -265.9057974263764095 ) ) ;
#9000 = CARTESIAN_POINT ( 'NONE',  ( 22.20486611472177430, -280.9968393556202955, -318.5711761363790515 ) ) ;
#9001 = CARTESIAN_POINT ( 'NONE',  ( -35.70447383852102519, -277.9733637830140083, -347.1214468863662432 ) ) ;
#9002 = CARTESIAN_POINT ( 'NONE',  ( 22.11308348202614482, -277.7193073687471383, -318.2131265242443305 ) ) ;
#9003 = CARTESIAN_POINT ( 'NONE',  ( -67.74223827176244583, -288.1233781216987495, -207.3071070584150277 ) ) ;
#9004 = ORIENTED_EDGE ( 'NONE', *, *, #61815, .F. ) ;
#9005 = CARTESIAN_POINT ( 'NONE',  ( -111.7230492094858505, -298.6807984470408996, -260.3544738186429868 ) ) ;
#9006 = CARTESIAN_POINT ( 'NONE',  ( -109.4806578211212695, -291.4604550107221144, -283.4070697366714739 ) ) ;
#9007 = CARTESIAN_POINT ( 'NONE',  ( -99.02185173252895822, -276.0002894747262303, -312.4016424949765565 ) ) ;
#9008 = CARTESIAN_POINT ( 'NONE',  ( -82.23567256706812145, -291.4155524855503359, -331.6677672964936505 ) ) ;
#9009 = CARTESIAN_POINT ( 'NONE',  ( -90.82811693935741459, -290.6164386047281596, -220.5119404252024538 ) ) ;
#9010 = CARTESIAN_POINT ( 'NONE',  ( 25.79761164024652587, -287.6423138074338794, -314.4179579310767281 ) ) ;
#9011 = DIRECTION ( 'NONE',  ( 0.000000000000000000, 1.000000000000000000, 0.000000000000000000 ) ) ;
#9012 = CARTESIAN_POINT ( 'NONE',  ( -108.1653458178780483, -282.6799777510105969, -291.1536097612043932 ) ) ;
#9013 = CARTESIAN_POINT ( 'NONE',  ( -108.1873992785075842, -292.7020722548153344, -248.1427604890856742 ) ) ;
#9014 = CARTESIAN_POINT ( 'NONE',  ( -111.0127717019655620, -282.9890455435875651, -273.6499541224108043 ) ) ;
#9015 = CARTESIAN_POINT ( 'NONE',  ( 35.92208456830006469, -282.9514093775057404, -276.7776406674568648 ) ) ;
#9016 = CARTESIAN_POINT ( 'NONE',  ( -113.1258495113986697, -291.3399737695850718, -282.5915274344486647 ) ) ;
#9017 = CARTESIAN_POINT ( 'NONE',  ( -72.16455490927796745, -280.0706252229320512, -206.1321741436102855 ) ) ;
#9018 = CARTESIAN_POINT ( 'NONE',  ( -66.84824534930707784, -290.4689132258185396, -199.6690214780654173 ) ) ;
#9019 = CARTESIAN_POINT ( 'NONE',  ( -18.23209208044610108, -287.0950523456058932, -195.8817975221083145 ) ) ;
#9020 = CARTESIAN_POINT ( 'NONE',  ( 16.64724545834705438, -288.8016692722566177, -325.2505412504290803 ) ) ;
#9021 = CARTESIAN_POINT ( 'NONE',  ( -54.75839660499872252, -285.9888039149282122, -199.4169394873675571 ) ) ;
#9022 = EDGE_LOOP ( 'NONE', ( #77636, #3269, #47700, #15442 ) ) ;
#9023 = CARTESIAN_POINT ( 'NONE',  ( 207.5220701109484764, 35.61982174545049418, 14.46441793359389472 ) ) ;
#9024 = CARTESIAN_POINT ( 'NONE',  ( 5.773560466611446174, -294.4901583558522020, -208.0603974234272755 ) ) ;
#9025 = CARTESIAN_POINT ( 'NONE',  ( -53.20346460585856363, -293.9361297981620851, -345.2598379404914226 ) ) ;
#9026 = CARTESIAN_POINT ( 'NONE',  ( 7.715752982756542977, -275.4786830379741787, -328.1598987853102471 ) ) ;
#9027 = CARTESIAN_POINT ( 'NONE',  ( -57.35518212490794099, -297.1491651875278990, -196.0578615553173734 ) ) ;
#9028 = AXIS2_PLACEMENT_3D ( 'NONE', #32266, #18061, #54037 ) ;
#9029 = CARTESIAN_POINT ( 'NONE',  ( 19.01924043422573263, -291.3638773980719634, -222.8832059282251237 ) ) ;
#9030 = CARTESIAN_POINT ( 'NONE',  ( -108.9556781276153430, -294.5480056551334087, -289.1038563849991192 ) ) ;
#9031 = CARTESIAN_POINT ( 'NONE',  ( -107.3851193177741266, -292.0468377927651886, -248.3858999071535436 ) ) ;
#9032 = CARTESIAN_POINT ( 'NONE',  ( 33.41866307921315382, -294.8844540275463828, -289.5712681157908150 ) ) ;
#9033 = CYLINDRICAL_SURFACE ( 'NONE', #53545, 7.500000000000007105 ) ;
#9034 = CARTESIAN_POINT ( 'NONE',  ( -76.15785261883388557, -293.5689970977561529, -334.7904234825163599 ) ) ;
#9035 = CARTESIAN_POINT ( 'NONE',  ( -96.95722480694192313, -299.1754566296349935, -224.8321829763796700 ) ) ;
#9036 = CARTESIAN_POINT ( 'NONE',  ( -75.98274653586904037, -290.5234782358363645, -332.5726762372370899 ) ) ;
#9037 = CARTESIAN_POINT ( 'NONE',  ( 20.48499476488876425, -278.1963951982112349, -318.6775765033436301 ) ) ;
#9038 = CARTESIAN_POINT ( 'NONE',  ( -97.29991040655650636, -277.8770260836623720, -222.8394250903219529 ) ) ;
#9039 = CARTESIAN_POINT ( 'NONE',  ( -35.51787812975899072, -273.4230329873620349, -193.4715689568409402 ) ) ;
#9040 = CARTESIAN_POINT ( 'NONE',  ( 22.50089894521741485, -279.0230394027645957, -226.0657631041955256 ) ) ;
#9041 = CARTESIAN_POINT ( 'NONE',  ( -106.6825880866542207, -277.3615779648814623, -238.6385575724773105 ) ) ;
#9042 = CARTESIAN_POINT ( 'NONE',  ( -109.5269028076874491, -295.4187228101516212, -256.4905491578002739 ) ) ;
#9043 = CARTESIAN_POINT ( 'NONE',  ( 159.4851178187871312, 3.000000000000000000, 10.00000000000000000 ) ) ;
#9044 = CARTESIAN_POINT ( 'NONE',  ( 2.979259126803790458, -275.2603832868280165, -209.3242943793279665 ) ) ;
#9045 = CARTESIAN_POINT ( 'NONE',  ( 194.7559826945684165, 25.47273943569134858, 13.95515289467987152 ) ) ;
#9046 = CARTESIAN_POINT ( 'NONE',  ( -102.3915876516510366, -288.0652167971555286, -308.5027731949417102 ) ) ;
#9047 = CARTESIAN_POINT ( 'NONE',  ( -62.76365278926252245, -289.3739762372574660, -343.0998545186443494 ) ) ;
#9048 = CARTESIAN_POINT ( 'NONE',  ( -64.26771943868617143, -275.7018206849599551, -200.1687961219183478 ) ) ;
#9049 = CARTESIAN_POINT ( 'NONE',  ( -111.8704363618436304, -270.6597741443814584, -261.9665886293834092 ) ) ;
#9050 = CARTESIAN_POINT ( 'NONE',  ( -94.28637210267525859, -283.0468769499836412, -321.9700062112144678 ) ) ;
#9051 = DIRECTION ( 'NONE',  ( 0.000000000000000000, 0.000000000000000000, -1.000000000000000000 ) ) ;
#9052 = CARTESIAN_POINT ( 'NONE',  ( -53.04522905397051602, -281.2531631837518944, -343.7511565776249540 ) ) ;
#9053 = LINE ( 'NONE', #45036, #84600 ) ;
#9054 = CARTESIAN_POINT ( 'NONE',  ( -86.18187002024816934, -290.1519657750760643, -215.5043268487193018 ) ) ;
#9055 = CARTESIAN_POINT ( 'NONE',  ( -65.54084169259586190, -283.8191963130745421, -201.6356442246963923 ) ) ;
#9056 = CYLINDRICAL_SURFACE ( 'NONE', #63911, 1.897123461337413275 ) ;
#9057 = LINE ( 'NONE', #73023, #89652 ) ;
#9058 = CARTESIAN_POINT ( 'NONE',  ( -3.919549599986841937, -290.4927471186967978, -203.2054626566140030 ) ) ;
#9059 = CARTESIAN_POINT ( 'NONE',  ( -109.8252022439424849, -279.9703319762656406, -284.3051988763929216 ) ) ;
#9060 = CARTESIAN_POINT ( 'NONE',  ( -52.82228976583626689, -284.4512265979993231, -345.4377237466878228 ) ) ;
#9062 = CARTESIAN_POINT ( 'NONE',  ( -68.77493573860628828, -285.6270494822316550, -204.4614294105641363 ) ) ;
#9061 = CARTESIAN_POINT ( 'NONE',  ( -75.68058511348679929, -271.6249904509796806, -205.1896579433549448 ) ) ;
#9063 = CARTESIAN_POINT ( 'NONE',  ( 16.97825691406048065, -277.6840354190537710, -320.0258360862624727 ) ) ;
#9064 = CARTESIAN_POINT ( 'NONE',  ( 11.86384937008692120, -277.1506600438700048, -324.5724204139773974 ) ) ;
#9065 = CARTESIAN_POINT ( 'NONE',  ( -84.81619400750905413, -285.7069368887969745, -328.4229219205618620 ) ) ;
#9066 = ORIENTED_EDGE ( 'NONE', *, *, #72401, .T. ) ;
#9067 = LINE ( 'NONE', #37945, #46744 ) ;
#9068 = CARTESIAN_POINT ( 'NONE',  ( -47.63367391941932283, -295.0128835428789102, -346.6701952930047810 ) ) ;
#9069 = CARTESIAN_POINT ( 'NONE',  ( 34.60811349049909325, -289.2751835694746205, -250.4847218052497340 ) ) ;
#9070 = CARTESIAN_POINT ( 'NONE',  ( 154.5625123364532101, 276.0000000000000568, 13.15740740740740655 ) ) ;
#9071 = CARTESIAN_POINT ( 'NONE',  ( 13.79469577742117181, -291.9094976428775681, -334.5364918783848793 ) ) ;
#9072 = CARTESIAN_POINT ( 'NONE',  ( -113.7722961570585625, -277.3854857085858043, -277.2894164562379729 ) ) ;
#9073 = CARTESIAN_POINT ( 'NONE',  ( -61.41630709679873945, -290.1445867640960046, -198.0085671765353084 ) ) ;
#9074 = CARTESIAN_POINT ( 'NONE',  ( -105.2438747793397624, -286.4545477554837021, -241.5941884883910689 ) ) ;
#9075 = CARTESIAN_POINT ( 'NONE',  ( -65.21828083107389773, -281.4429071139934990, -201.7982252296305603 ) ) ;
#9076 = CARTESIAN_POINT ( 'NONE',  ( 29.60648202368650317, -288.4954783408682033, -233.4200445227367879 ) ) ;
#9077 = CARTESIAN_POINT ( 'NONE',  ( 35.38898843834155628, -283.3165065688847903, -251.9992449447169918 ) ) ;
#9078 = CARTESIAN_POINT ( 'NONE',  ( -38.54283052506055185, -277.2335025225759750, -347.3517491677973794 ) ) ;
#9079 = CARTESIAN_POINT ( 'NONE',  ( -87.18016726726369825, -295.3736879954219035, -214.7915760252834048 ) ) ;
#9080 = CARTESIAN_POINT ( 'NONE',  ( -53.75840807855522030, -279.6805314468577990, -195.0769560434037260 ) ) ;
#9081 = CARTESIAN_POINT ( 'NONE',  ( -75.97856087260620939, -299.4523638578721147, -206.6734643332680719 ) ) ;
#9082 = CARTESIAN_POINT ( 'NONE',  ( 156.4851178187871312, 15.09609934344202387, 9.999999999995333511 ) ) ;
#9083 = EDGE_CURVE ( 'NONE', #36747, #82861, #28330, .T. ) ;
#9084 = CARTESIAN_POINT ( 'NONE',  ( -95.95921662488163406, -280.4090924074130839, -317.1477375740089997 ) ) ;
#9085 = TOROIDAL_SURFACE ( 'NONE', #49933, 24.50000000000000355, 0.5000000000000000000 ) ;
#9086 = CARTESIAN_POINT ( 'NONE',  ( -34.12338131277177666, -272.3319715076768261, -194.4426324905445256 ) ) ;
#9087 = DIRECTION ( 'NONE',  ( 0.000000000000000000, 1.000000000000000000, 0.000000000000000000 ) ) ;
#9088 = CARTESIAN_POINT ( 'NONE',  ( -110.2302281622285847, -277.9844574312039640, -276.0774600598558663 ) ) ;
#9089 = CARTESIAN_POINT ( 'NONE',  ( -10.50119546144568083, -275.5996092216494162, -198.5579425985381192 ) ) ;
#9090 = AXIS2_PLACEMENT_3D ( 'NONE', #25554, #91818, #55862 ) ;
#9091 = CARTESIAN_POINT ( 'NONE',  ( 29.08898020384873462, -280.1091290761240771, -231.8931452900570207 ) ) ;
#9092 = CARTESIAN_POINT ( 'NONE',  ( 6.462152538122775347, -290.2083388516452374, -330.0840053592891650 ) ) ;
#9093 = CARTESIAN_POINT ( 'NONE',  ( -46.06995541350183743, -299.4634762869117139, -194.5552784217425994 ) ) ;
#9094 = CARTESIAN_POINT ( 'NONE',  ( -36.91511479489226133, -299.2624507052767626, -193.7581024177941345 ) ) ;
#9095 = CARTESIAN_POINT ( 'NONE',  ( -64.76662492848308261, -293.6933763771612576, -200.7203664096375917 ) ) ;
#9096 = CARTESIAN_POINT ( 'NONE',  ( -0.3677987265727220012, -280.5591494301300486, -335.4223125805726227 ) ) ;
#9097 = CARTESIAN_POINT ( 'NONE',  ( 35.98134780013140954, -283.3061134356186699, -257.5141400509570531 ) ) ;
#9098 = CARTESIAN_POINT ( 'NONE',  ( -103.4762885368125040, -271.0342565457213482, -235.6361918315443802 ) ) ;
#9099 = CARTESIAN_POINT ( 'NONE',  ( -91.35048713360309591, -286.8993379835645783, -216.6071289141591478 ) ) ;
#9100 = CARTESIAN_POINT ( 'NONE',  ( -90.82766209874905883, -288.7534240805092054, -320.5698635611984173 ) ) ;
#9101 = CARTESIAN_POINT ( 'NONE',  ( -106.5399784064848205, -263.2081406146079985, -317.6450301294818246 ) ) ;
#9102 = ORIENTED_EDGE ( 'NONE', *, *, #63994, .F. ) ;
#9103 = CARTESIAN_POINT ( 'NONE',  ( -17.89195695092106675, -287.3808470759522038, -344.2550540104290917 ) ) ;
#9104 = CARTESIAN_POINT ( 'NONE',  ( -37.27225823610147870, -288.7179772498128045, -343.3822290717908459 ) ) ;
#9105 = ORIENTED_EDGE ( 'NONE', *, *, #470, .T. ) ;
#9106 = CARTESIAN_POINT ( 'NONE',  ( -114.0452827560740303, -285.6005324968264745, -272.8529630916000315 ) ) ;
#9107 = CARTESIAN_POINT ( 'NONE',  ( 24.00445485794711686, -276.4346995311299224, -310.0616403739940097 ) ) ;
#9108 = EDGE_CURVE ( 'NONE', #19715, #38465, #78975, .T. ) ;
#9109 = CARTESIAN_POINT ( 'NONE',  ( 37.12510951001195281, -292.2421902434831509, -252.0257212505495090 ) ) ;
#9110 = CARTESIAN_POINT ( 'NONE',  ( 37.09522644561252491, -282.4454282303729542, -289.6602565434245093 ) ) ;
#9111 = CARTESIAN_POINT ( 'NONE',  ( 28.67695266115447694, -282.5701066125907346, -232.0956605147805476 ) ) ;
#9112 = CARTESIAN_POINT ( 'NONE',  ( 21.59656273432573315, -282.5523519239649772, -319.8790486983861570 ) ) ;
#9113 = CARTESIAN_POINT ( 'NONE',  ( 13.33510197507002459, -280.7849264556178923, -217.7467716656487937 ) ) ;
#9114 = CARTESIAN_POINT ( 'NONE',  ( -67.74223827176246004, -292.9809262143061233, -333.4151289067050357 ) ) ;
#9115 = CARTESIAN_POINT ( 'NONE',  ( 25.64300257841772535, -23.00939279306157559, -345.2368619827582279 ) ) ;
#9116 = ORIENTED_EDGE ( 'NONE', *, *, #65647, .F. ) ;
#9117 = CARTESIAN_POINT ( 'NONE',  ( 36.92881274143096704, -277.6755328978853754, -279.9362686722686817 ) ) ;
#9118 = CARTESIAN_POINT ( 'NONE',  ( -96.09881083034818516, -239.5351746575481116, -341.4074303404881903 ) ) ;
#9119 = CARTESIAN_POINT ( 'NONE',  ( 9.018223279003795056, -297.9961767976545275, -197.2644819129092468 ) ) ;
#9120 = CARTESIAN_POINT ( 'NONE',  ( 26.45720724600711904, -293.6268434591170262, -313.3637495427612976 ) ) ;
#9121 = CARTESIAN_POINT ( 'NONE',  ( 85.38584713910209700, 81.22694468296866432, -299.0555890527453471 ) ) ;
#9123 = CARTESIAN_POINT ( 'NONE',  ( -45.47058429120745160, -287.5567332815635950, -343.7120665572656435 ) ) ;
#9122 = CARTESIAN_POINT ( 'NONE',  ( -23.47448262698475219, -296.7972917440171159, -193.9536260485545256 ) ) ;
#9124 = CARTESIAN_POINT ( 'NONE',  ( -109.4940434518397012, -298.1853584393807637, -287.8761787819575488 ) ) ;
#9125 = CARTESIAN_POINT ( 'NONE',  ( -67.76704287674850491, -286.9594315245317375, -203.4616262207693183 ) ) ;
#9126 = ORIENTED_EDGE ( 'NONE', *, *, #65006, .F. ) ;
#9127 = CARTESIAN_POINT ( 'NONE',  ( -93.50911006021783578, -296.7777182059328993, -322.7067802158568952 ) ) ;
#9128 = CARTESIAN_POINT ( 'NONE',  ( -80.65758281933071316, -284.1496973153713839, -329.2604653410962783 ) ) ;
#9129 = CARTESIAN_POINT ( 'NONE',  ( -51.71100489476024364, -296.6673148526487580, -195.0639097959698347 ) ) ;
#9130 = CARTESIAN_POINT ( 'NONE',  ( -11.21778715862602915, -293.1867848522107920, -198.0438698485044995 ) ) ;
#9131 = CARTESIAN_POINT ( 'NONE',  ( 17.44137971370090057, -293.3012842422797348, -216.2644325114591766 ) ) ;
#9132 = CARTESIAN_POINT ( 'NONE',  ( -83.83066911307926716, -291.5594250562043044, -214.0781208413714580 ) ) ;
#9133 = VERTEX_POINT ( 'NONE', #16318 ) ;
#9134 = DIRECTION ( 'NONE',  ( 0.000000000000000000, 0.000000000000000000, 1.000000000000000000 ) ) ;
#9135 = CARTESIAN_POINT ( 'NONE',  ( -104.1753700635891846, -298.8825151260207917, -234.5627023305806631 ) ) ;
#9136 = CARTESIAN_POINT ( 'NONE',  ( 27.30544482081423041, -274.8895997679970264, -311.5541567216604903 ) ) ;
#9137 = ORIENTED_EDGE ( 'NONE', *, *, #28588, .F. ) ;
#9138 = ORIENTED_EDGE ( 'NONE', *, *, #6687, .T. ) ;
#9139 = CARTESIAN_POINT ( 'NONE',  ( -84.83332288771921981, -277.1944949473821680, -330.9604025014336912 ) ) ;
#9140 = CARTESIAN_POINT ( 'NONE',  ( -34.42629273200908102, -296.5691725639474612, -196.6685504366246562 ) ) ;
#9141 = CARTESIAN_POINT ( 'NONE',  ( -75.15503193404150295, -281.4033739698395493, -206.4191824871593610 ) ) ;
#9142 = CARTESIAN_POINT ( 'NONE',  ( -37.84145811329845088, -275.1980249520919983, -344.6073027684507792 ) ) ;
#9143 = CARTESIAN_POINT ( 'NONE',  ( -47.34195471741013250, -299.1274695561657495, -197.5970055555608553 ) ) ;
#9144 = CARTESIAN_POINT ( 'NONE',  ( -110.4244668606738031, -273.5651163645595716, -264.9078314618561194 ) ) ;
#9145 = CARTESIAN_POINT ( 'NONE',  ( -113.3283667958448717, -274.3120101190713740, -270.3834786793233889 ) ) ;
#9146 = CARTESIAN_POINT ( 'NONE',  ( -54.92483659935874130, -271.8472745662669467, -197.0860191318285786 ) ) ;
#9147 = CARTESIAN_POINT ( 'NONE',  ( -35.63993590234115061, -295.6816902625537864, -343.4557541938581835 ) ) ;
#9148 = CARTESIAN_POINT ( 'NONE',  ( -62.98921826990011397, -290.2862291908141970, -201.3859069991136437 ) ) ;
#9149 = LINE ( 'NONE', #24784, #83506 ) ;
#9150 = CARTESIAN_POINT ( 'NONE',  ( -56.90232548531886891, -277.7900761719059233, -344.8265334085669451 ) ) ;
#9151 = CARTESIAN_POINT ( 'NONE',  ( 31.11758006296859946, -275.3808760783071534, -245.0169478399705838 ) ) ;
#9152 = CARTESIAN_POINT ( 'NONE',  ( -63.02004936067496033, -284.4094411572768877, -198.2922574883576488 ) ) ;
#9153 = CARTESIAN_POINT ( 'NONE',  ( -112.5049693374609490, -298.5614778661650348, -269.6460059547466699 ) ) ;
#9154 = DIRECTION ( 'NONE',  ( -1.000000000000000000, 0.000000000000000000, 0.000000000000000000 ) ) ;
#9155 = CARTESIAN_POINT ( 'NONE',  ( -5.719616189304495002, -285.6760467203123426, -204.3727202851144966 ) ) ;
#9156 = CARTESIAN_POINT ( 'NONE',  ( -112.5073296679233579, -282.5570572200399511, -269.9654422040516693 ) ) ;
#9157 = CARTESIAN_POINT ( 'NONE',  ( -98.49860391413844241, -276.2200049760867842, -312.0481319462705301 ) ) ;
#9158 = CARTESIAN_POINT ( 'NONE',  ( -94.92537007064133547, -276.4847930727288485, -316.2015080090582728 ) ) ;
#9160 = CARTESIAN_POINT ( 'NONE',  ( -87.95950376613905064, -281.3449301281473254, -214.9489759980830286 ) ) ;
#9159 = TOROIDAL_SURFACE ( 'NONE', #62106, 1.500000000000000000, 0.5000000000000000000 ) ;
#9161 = CARTESIAN_POINT ( 'NONE',  ( 9.728031657626821982, -275.9216909358538032, -213.9778722357959850 ) ) ;
#9162 = CARTESIAN_POINT ( 'NONE',  ( 153.9133111279456045, 20.47222690886500729, 13.06183683676587037 ) ) ;
#9163 = CARTESIAN_POINT ( 'NONE',  ( -108.4129980346834827, -271.3054697768196775, -242.7330557397093287 ) ) ;
#9164 = AXIS2_PLACEMENT_3D ( 'NONE', #51355, #93513, #79342 ) ;
#9165 = CARTESIAN_POINT ( 'NONE',  ( -47.88737891490783483, -281.9186281276775503, -195.8853239550579133 ) ) ;
#9166 = DIRECTION ( 'NONE',  ( -0.000000000000000000, -1.000000000000000000, -0.000000000000000000 ) ) ;
#9167 = CARTESIAN_POINT ( 'NONE',  ( -82.43644798484535841, -287.3623993679281625, -209.6676621444179887 ) ) ;
#9168 = SURFACE_STYLE_FILL_AREA ( #8711 ) ;
#9169 = CARTESIAN_POINT ( 'NONE',  ( -56.38500114910112160, -289.8067327222232734, -197.7660584288144321 ) ) ;
#9170 = DIRECTION ( 'NONE',  ( 0.000000000000000000, 0.000000000000000000, 1.000000000000000000 ) ) ;
#9171 = CARTESIAN_POINT ( 'NONE',  ( -35.11733266678204757, -296.8755288573426583, -196.9645103397436969 ) ) ;
#9172 = CARTESIAN_POINT ( 'NONE',  ( -90.68775549754472820, -289.4253738842709254, -218.7368615088576007 ) ) ;
#9173 = CARTESIAN_POINT ( 'NONE',  ( 65.71450562203199297, 45.78484130816451625, -315.1169351998001389 ) ) ;
#9174 = CARTESIAN_POINT ( 'NONE',  ( -83.63170945779074827, -298.0521521680024080, -525.1711561948568487 ) ) ;
#9175 = CARTESIAN_POINT ( 'NONE',  ( 37.04810059467506989, -285.8168868228125916, -253.3070234639806415 ) ) ;
#9176 = CARTESIAN_POINT ( 'NONE',  ( -23.90001074543902249, -284.4777052374152504, -342.9266841951295532 ) ) ;
#9177 = CARTESIAN_POINT ( 'NONE',  ( -77.96159486801235516, -283.7541092000960248, -206.1427548461797983 ) ) ;
#9178 = CARTESIAN_POINT ( 'NONE',  ( -108.1084758968160457, -290.7892470358717674, -252.3920358492311493 ) ) ;
#9179 = CARTESIAN_POINT ( 'NONE',  ( 0.6890442174752087201, -281.9948814677866267, -207.3018416625570239 ) ) ;
#9180 = CARTESIAN_POINT ( 'NONE',  ( 21.14513809291120694, -282.9710290070006522, -314.3351112133436231 ) ) ;
#9181 = CARTESIAN_POINT ( 'NONE',  ( -12.73644950063787817, -290.7139001104780505, -341.6407181709393512 ) ) ;
#9182 = CARTESIAN_POINT ( 'NONE',  ( -36.54275480140048415, -298.2285753783489781, -193.3610960453318341 ) ) ;
#9183 = B_SPLINE_CURVE_WITH_KNOTS ( 'NONE', 3,
 ( #10455, #40722, #9994, #32250, #67773, #40257 ),
 .UNSPECIFIED., .F., .F.,
 ( 4, 2, 4 ),
 ( 0.000000000000000000, 0.001358919387270749205, 0.002717838774541498411 ),
 .UNSPECIFIED. ) ;
#9184 = ORIENTED_EDGE ( 'NONE', *, *, #25508, .T. ) ;
#9185 = CARTESIAN_POINT ( 'NONE',  ( -26.37811156009245650, -286.9935048667940691, -345.1214946649760691 ) ) ;
#9186 = CARTESIAN_POINT ( 'NONE',  ( 34.18425571773870786, -275.9155106654981751, -299.0186854183480136 ) ) ;
#9187 = CARTESIAN_POINT ( 'NONE',  ( -19.70750661701979212, -294.2597570172372912, -197.7757371491893821 ) ) ;
#9188 = CARTESIAN_POINT ( 'NONE',  ( 210.8848006936870263, 293.9636489450776367, -54.00000000000000000 ) ) ;
#9189 = CARTESIAN_POINT ( 'NONE',  ( -106.6379572354042296, -280.6233781216988064, -303.7686719486574702 ) ) ;
#9190 = CARTESIAN_POINT ( 'NONE',  ( -96.50212868765615326, -275.9170559266127043, -316.7299881841029219 ) ) ;
#9191 = CARTESIAN_POINT ( 'NONE',  ( 156.1760182705795899, 20.00000000000000355, -14.66829968254867111 ) ) ;
#9192 = CARTESIAN_POINT ( 'NONE',  ( -86.92607734711852174, -295.7757042214179819, -212.4311402268074005 ) ) ;
#9193 = CARTESIAN_POINT ( 'NONE',  ( -90.26468574689654645, -272.6271513255361469, -219.9141414218865123 ) ) ;
#9194 = CARTESIAN_POINT ( 'NONE',  ( -109.9633529955325457, -292.2397244722101846, -257.5472157442295043 ) ) ;
#9195 = CARTESIAN_POINT ( 'NONE',  ( -96.95986742359423260, -292.0867545243746690, -227.7420105527843930 ) ) ;
#9196 = CARTESIAN_POINT ( 'NONE',  ( -108.7327328792310084, -286.0572837542106868, -289.9356755233485501 ) ) ;
#9197 = CARTESIAN_POINT ( 'NONE',  ( 17.05726805101543420, -294.2340589614796045, -216.6269770537394379 ) ) ;
#9198 = CARTESIAN_POINT ( 'NONE',  ( 37.57556621645260009, -294.6712314311852765, -254.7824184169341777 ) ) ;
#9199 = CARTESIAN_POINT ( 'NONE',  ( 29.48920500658742228, -293.7806032168152228, -299.7316835774735182 ) ) ;
#9200 = CARTESIAN_POINT ( 'NONE',  ( 25.18780854749623188, -288.9919255907174147, -228.8538412119010275 ) ) ;
#9201 = CARTESIAN_POINT ( 'NONE',  ( 17.82775891794059220, -282.4559784356180785, -324.1525821193869206 ) ) ;
#9202 = CARTESIAN_POINT ( 'NONE',  ( -79.79536173366994944, -295.5633072455308934, -207.7922159327702332 ) ) ;
#9203 = CARTESIAN_POINT ( 'NONE',  ( -57.75389097702219487, -285.6290778144822866, -196.0606156211788402 ) ) ;
#9204 = CARTESIAN_POINT ( 'NONE',  ( 23.60964851202093584, -276.9435381818844348, -227.2486325963364493 ) ) ;
#9205 = EDGE_CURVE ( 'NONE', #90412, #75708, #23881, .T. ) ;
#9206 = CARTESIAN_POINT ( 'NONE',  ( -107.7314009193064095, -283.6228332469245856, -249.3902518422579533 ) ) ;
#9207 = CARTESIAN_POINT ( 'NONE',  ( 22.52985302956614433, -286.1695701984517655, -315.5318803675999106 ) ) ;
#9208 = CARTESIAN_POINT ( 'NONE',  ( -112.9763733789620659, -276.7481522989206155, -265.9224604803757757 ) ) ;
#9209 = CARTESIAN_POINT ( 'NONE',  ( 201.0592549708491958, 40.73798607845790798, 10.50000000000000000 ) ) ;
#9210 = CARTESIAN_POINT ( 'NONE',  ( -103.5385673699460085, -284.4783959399725859, -239.3225538553712397 ) ) ;
#9211 = CARTESIAN_POINT ( 'NONE',  ( -112.3320105730065990, -279.9545684241080608, -254.6625159821743694 ) ) ;
#9212 = CARTESIAN_POINT ( 'NONE',  ( 33.64642815502740092, -286.2369473492973384, -241.0073738777431060 ) ) ;
#9213 = CARTESIAN_POINT ( 'NONE',  ( -8.819951329815337360, -296.4339930625933448, -338.6719415027869218 ) ) ;
#9214 = CARTESIAN_POINT ( 'NONE',  ( -20.28514319310341563, -278.4368442357993558, -344.6817803636983513 ) ) ;
#9215 = CARTESIAN_POINT ( 'NONE',  ( 19.52196237491152075, -277.5667152321353797, -321.5649270622869835 ) ) ;
#9216 = CARTESIAN_POINT ( 'NONE',  ( -70.45469727677706828, -277.3347523296615122, -335.4190108500763472 ) ) ;
#9217 = CARTESIAN_POINT ( 'NONE',  ( -93.23065889118245764, -299.2464325808889498, -220.5971479192537004 ) ) ;
#9218 = CARTESIAN_POINT ( 'NONE',  ( -16.64088514526811124, -284.3199027410548752, -198.3937629426661431 ) ) ;
#9219 = CARTESIAN_POINT ( 'NONE',  ( -59.77214241290157304, -290.9381350083733082, -343.1849854490653797 ) ) ;
#9220 = CARTESIAN_POINT ( 'NONE',  ( -20.79170200569873472, -293.7551444382265231, -341.8299909895254132 ) ) ;
#9221 = VERTEX_POINT ( 'NONE', #2117 ) ;
#9222 = CARTESIAN_POINT ( 'NONE',  ( 34.85822803511160828, -293.3672232948167107, -281.6104102700148246 ) ) ;
#9223 = CARTESIAN_POINT ( 'NONE',  ( -84.08885930499720018, -292.5065349058130550, -209.4978330762367591 ) ) ;
#9224 = CARTESIAN_POINT ( 'NONE',  ( -37.01618781890024223, -280.7077496143334656, -197.2599093036648128 ) ) ;
#9225 = EDGE_CURVE ( 'NONE', #74598, #10872, #52749, .T. ) ;
#9226 = CARTESIAN_POINT ( 'NONE',  ( 19.11967835457857845, -297.6638056878800853, -193.6802856397917481 ) ) ;
#9227 = CARTESIAN_POINT ( 'NONE',  ( 39.60060493744474286, -288.2183452828665509, -271.5414338850840181 ) ) ;
#9228 = CARTESIAN_POINT ( 'NONE',  ( 19.61146230834608417, -288.5896331962988484, -322.1695704097429598 ) ) ;
#9229 = CARTESIAN_POINT ( 'NONE',  ( -35.93731551994839890, -286.4035304601642906, -197.3534800894326509 ) ) ;
#9230 = FACE_OUTER_BOUND ( 'NONE', #55636, .T. ) ;
#9231 = CARTESIAN_POINT ( 'NONE',  ( -104.8366539456450539, -254.2583971032736940, -325.3939605836368969 ) ) ;
#9232 = CARTESIAN_POINT ( 'NONE',  ( -102.1682833893122790, -254.0870747469653566, -324.0649701474447966 ) ) ;
#9233 = CONICAL_SURFACE ( 'NONE', #21421, 8.550761578869359170, 0.7853981633974639331 ) ;
#9234 = CARTESIAN_POINT ( 'NONE',  ( -36.47449613086610753, -276.2382106544087037, -343.5299502666913440 ) ) ;
#9235 = CARTESIAN_POINT ( 'NONE',  ( -99.44423846440159309, -276.9356955854393050, -309.4110797231923016 ) ) ;
#9236 = CARTESIAN_POINT ( 'NONE',  ( -14.82618927689352972, -297.8346270237912563, -193.4244760388092175 ) ) ;
#9237 = CARTESIAN_POINT ( 'NONE',  ( 46.66400796352151303, 10.61984656453235587, -329.2320478923130054 ) ) ;
#9238 = CARTESIAN_POINT ( 'NONE',  ( -96.68258349367351911, -276.5846228379504055, -318.6719875330187506 ) ) ;
#9239 = CARTESIAN_POINT ( 'NONE',  ( -81.26741293479715011, -297.3999401733335617, -332.4294497083434976 ) ) ;
#9240 = ORIENTED_EDGE ( 'NONE', *, *, #15737, .T. ) ;
#9241 = CARTESIAN_POINT ( 'NONE',  ( -110.0347439241129734, -291.1410984331432132, -263.0324192407556438 ) ) ;
#9242 = CARTESIAN_POINT ( 'NONE',  ( -107.6294690725139276, -297.7533807336070026, -239.1845865574373988 ) ) ;
#9243 = CARTESIAN_POINT ( 'NONE',  ( -95.95538381259881078, -273.8756416572669536, -220.5638496629271685 ) ) ;
#9244 = CARTESIAN_POINT ( 'NONE',  ( -104.9611038077306375, -296.3503672220018075, -297.8677762764351655 ) ) ;
#9245 = ORIENTED_EDGE ( 'NONE', *, *, #50089, .F. ) ;
#9246 = DIRECTION ( 'NONE',  ( 0.000000000000000000, 0.000000000000000000, 1.000000000000000000 ) ) ;
#9247 = CARTESIAN_POINT ( 'NONE',  ( -17.70806079349900841, -278.7209958060949475, -343.3257285949125048 ) ) ;
#9248 = CARTESIAN_POINT ( 'NONE',  ( -2.925997099835125681, -282.1172802842498299, -339.1877222854670890 ) ) ;
#9249 = CARTESIAN_POINT ( 'NONE',  ( -97.89644304253572216, -279.0593592761925379, -311.6812000781450251 ) ) ;
#9250 = CARTESIAN_POINT ( 'NONE',  ( -97.98103580883828556, -279.6940580695944050, -316.1737855163179347 ) ) ;
#9251 = CARTESIAN_POINT ( 'NONE',  ( -40.78817235996842783, -272.4880299243721424, -196.6982445760002065 ) ) ;
#9252 = CARTESIAN_POINT ( 'NONE',  ( 73.43068321062708037, -181.2434395487258598, 0.000000000000000000 ) ) ;
#9253 = DIRECTION ( 'NONE',  ( 0.000000000000000000, -0.000000000000000000, 1.000000000000000000 ) ) ;
#9254 = CARTESIAN_POINT ( 'NONE',  ( -57.11524933343630295, -279.9565163721202339, -200.0901655462288602 ) ) ;
#9255 = CARTESIAN_POINT ( 'NONE',  ( 10.43367144330280105, -277.2147819990506150, -330.6094025640717291 ) ) ;
#9256 = CARTESIAN_POINT ( 'NONE',  ( 33.32532904734250678, -277.8796050551589474, -295.6374761423203950 ) ) ;
#9257 = CARTESIAN_POINT ( 'NONE',  ( -1.758340108244709432, -275.1647528702646923, -337.9808694157658238 ) ) ;
#9258 = ORIENTED_EDGE ( 'NONE', *, *, #17906, .F. ) ;
#9259 = CARTESIAN_POINT ( 'NONE',  ( 208.4306832106270804, -124.2391364535881024, 0.000000000000000000 ) ) ;
#9260 = CARTESIAN_POINT ( 'NONE',  ( 37.77016376036974776, -283.4547181006087726, -264.3101094794230335 ) ) ;
#9261 = CARTESIAN_POINT ( 'NONE',  ( -55.04154764649329223, -291.0158151446058810, -199.3729702094652225 ) ) ;
#9262 = CARTESIAN_POINT ( 'NONE',  ( 24.62605641101286125, -286.2951263686590551, -224.8275047242626385 ) ) ;
#9263 = CARTESIAN_POINT ( 'NONE',  ( -66.98573991443798548, -281.6859368285051346, -338.1923178402363988 ) ) ;
#9265 = CARTESIAN_POINT ( 'NONE',  ( 17.04289510117902040, -284.9147758917934539, -219.5128798779178112 ) ) ;
#9264 = CARTESIAN_POINT ( 'NONE',  ( -83.17578265238967106, -282.2683916607443280, -327.9991844447695257 ) ) ;
#9266 = CARTESIAN_POINT ( 'NONE',  ( 15.53484523709902021, -282.0254844878625704, -219.3846845375686883 ) ) ;
#9267 = CARTESIAN_POINT ( 'NONE',  ( 202.9738562182569694, 295.9636489450776367, -54.00000000004089173 ) ) ;
#9268 = CARTESIAN_POINT ( 'NONE',  ( 26.04498570800102186, -280.5145684407276576, -312.6525884457160487 ) ) ;
#9269 = CARTESIAN_POINT ( 'NONE',  ( 24.09146401314860597, -296.1366013369365078, -313.4064074905962229 ) ) ;
#9270 = CARTESIAN_POINT ( 'NONE',  ( -103.8227961372751196, -287.0174945330898595, -235.1740781949551433 ) ) ;
#9271 = CYLINDRICAL_SURFACE ( 'NONE', #68592, 7.500000000000013323 ) ;
#9272 = CARTESIAN_POINT ( 'NONE',  ( -103.3638481591172678, -292.9577530237928613, -233.6134627514234694 ) ) ;
#9273 = CARTESIAN_POINT ( 'NONE',  ( 34.79040958219606239, -273.2854874014033726, -249.6336676311344149 ) ) ;
#9274 = CARTESIAN_POINT ( 'NONE',  ( -5.702344222117779360, -287.8437307093554978, -340.3833285940913811 ) ) ;
#9275 = CARTESIAN_POINT ( 'NONE',  ( 19.97991237435656942, -291.3013309531997947, -223.8580820775575546 ) ) ;
#9276 = CARTESIAN_POINT ( 'NONE',  ( -48.18343439339133027, -269.7948820652890731, -438.7219023889692835 ) ) ;
#9277 = CARTESIAN_POINT ( 'NONE',  ( -89.44719669208357971, -276.4896035446204792, -322.2625502989038750 ) ) ;
#9278 = CARTESIAN_POINT ( 'NONE',  ( -105.8939361676800104, -295.0673922253043315, -241.8750439835143879 ) ) ;
#9279 = CARTESIAN_POINT ( 'NONE',  ( -53.50077043607949179, -290.5790032532176497, -342.0558034434805563 ) ) ;
#9280 = DIRECTION ( 'NONE',  ( 0.000000000000000000, 1.000000000000000000, 0.000000000000000000 ) ) ;
#9281 = CARTESIAN_POINT ( 'NONE',  ( 201.2104617360081704, 15.00000000000000000, 10.00000000000000000 ) ) ;
#9282 = CARTESIAN_POINT ( 'NONE',  ( 28.96254726950153113, -292.5281954743124970, -308.2362442120626724 ) ) ;
#9283 = CARTESIAN_POINT ( 'NONE',  ( 22.62989943797673575, -288.5565931269269981, -227.2651356116299155 ) ) ;
#9284 = CARTESIAN_POINT ( 'NONE',  ( -94.87875627210028995, -289.4714041571656367, -220.7079701932398450 ) ) ;
#9285 = EDGE_CURVE ( 'NONE', #6260, #33595, #40858, .T. ) ;
#9286 = CARTESIAN_POINT ( 'NONE',  ( 32.39321816517778529, -288.6676917040457511, -246.8575844714772813 ) ) ;
#9287 = DIRECTION ( 'NONE',  ( 0.000000000000000000, 0.000000000000000000, 1.000000000000000000 ) ) ;
#9288 = CARTESIAN_POINT ( 'NONE',  ( 19.64568605195591644, -289.0022081802937919, -316.2418279152250307 ) ) ;
#9289 = CARTESIAN_POINT ( 'NONE',  ( 26.72119379197537015, -296.0633791598679636, -310.1373111701892071 ) ) ;
#9290 = DIRECTION ( 'NONE',  ( 0.000000000000000000, 0.000000000000000000, 1.000000000000000000 ) ) ;
#9291 = CARTESIAN_POINT ( 'NONE',  ( 31.33825936494917386, -289.1968139352492244, -304.4082472752643866 ) ) ;
#9292 = CARTESIAN_POINT ( 'NONE',  ( -33.96323542717557586, -278.1145699907761468, -195.0816866541901220 ) ) ;
#9293 = CARTESIAN_POINT ( 'NONE',  ( -103.5854320905429802, -278.3732943287595276, -309.6767640793804048 ) ) ;
#9294 = VECTOR ( 'NONE', #62190, 1000.000000000000000 ) ;
#9295 = CARTESIAN_POINT ( 'NONE',  ( -79.89555834670423451, -279.1606471997329777, -206.1495867284706094 ) ) ;
#9296 = CARTESIAN_POINT ( 'NONE',  ( -107.3572157436031489, -298.8712320091726156, -244.3338223848977862 ) ) ;
#9297 = CARTESIAN_POINT ( 'NONE',  ( -111.5886471288081765, -282.6881124382738335, -259.7596317679280560 ) ) ;
#9298 = CARTESIAN_POINT ( 'NONE',  ( 193.9343195356973126, 214.9970011440366875, 17.23862273017082458 ) ) ;
#9299 = CARTESIAN_POINT ( 'NONE',  ( -8.750080944692463447, -278.5698607786820276, -201.8528353145363781 ) ) ;
#9300 = CARTESIAN_POINT ( 'NONE',  ( -109.1992937345548569, -282.2747094013134870, -291.8880122362516545 ) ) ;
#9301 = DIRECTION ( 'NONE',  ( 0.000000000000000000, 0.000000000000000000, 1.000000000000000000 ) ) ;
#9302 = CARTESIAN_POINT ( 'NONE',  ( -6.869518930715255323, -275.1393295584406928, -340.3334737087832877 ) ) ;
#9303 = CIRCLE ( 'NONE', #30486, 4.999999999999986677 ) ;
#9304 = CARTESIAN_POINT ( 'NONE',  ( -63.80001349355167406, -296.9234865064245810, -339.1950108594052722 ) ) ;
#9305 = CARTESIAN_POINT ( 'NONE',  ( -37.32816513526459801, -281.9722845857710922, -347.0650187101471715 ) ) ;
#9306 = CARTESIAN_POINT ( 'NONE',  ( -101.6682902808948796, -297.0171056054360292, -305.3682350702949293 ) ) ;
#9307 = CARTESIAN_POINT ( 'NONE',  ( 52.84749097760590075, -300.4742676677981308, -193.8345526933532597 ) ) ;
#9308 = CARTESIAN_POINT ( 'NONE',  ( 17.30419981504129368, -274.5262934496395815, -221.8515619462640984 ) ) ;
#9309 = CARTESIAN_POINT ( 'NONE',  ( 36.44639545423920879, -295.3789794707898295, -256.8615969540347805 ) ) ;
#9310 = CARTESIAN_POINT ( 'NONE',  ( 34.04312958210429230, -288.0868973087494851, -299.3684577602278978 ) ) ;
#9311 = CARTESIAN_POINT ( 'NONE',  ( -99.05842242463586445, -277.2198575950725967, -226.7679948077680763 ) ) ;
#9312 = CARTESIAN_POINT ( 'NONE',  ( -114.0066250333133411, -290.4821002456295673, -262.6348487506654692 ) ) ;
#9313 = CARTESIAN_POINT ( 'NONE',  ( -45.40020517645733378, -288.2155034653073358, -343.1517007822778851 ) ) ;
#9314 = CARTESIAN_POINT ( 'NONE',  ( 33.58645800185961861, -291.8692495818679049, -294.8962646433143391 ) ) ;
#9315 = ORIENTED_EDGE ( 'NONE', *, *, #25921, .F. ) ;
#9316 = LINE ( 'NONE', #67112, #28797 ) ;
#9317 = CARTESIAN_POINT ( 'NONE',  ( -95.82134458623738738, -289.4453256542315103, -314.1783413290849580 ) ) ;
#9318 = CARTESIAN_POINT ( 'NONE',  ( 204.6539576904058606, 300.2961574867697436, -4.888549259831427740 ) ) ;
#9319 = CARTESIAN_POINT ( 'NONE',  ( -69.70459707143959349, -286.5776924869188065, -200.7374348708920877 ) ) ;
#9320 = CARTESIAN_POINT ( 'NONE',  ( -37.37352853689063181, -294.5519495502701375, -200.3611179825600459 ) ) ;
#9321 = CARTESIAN_POINT ( 'NONE',  ( 34.22778269782197214, -292.9636815480681662, -298.1213294457143661 ) ) ;
#9322 = CARTESIAN_POINT ( 'NONE',  ( 22.15043002687142959, -283.5166811540997855, -318.4856890816274699 ) ) ;
#9323 = CARTESIAN_POINT ( 'NONE',  ( -106.9864936730093348, -284.0955080349102104, -292.2381090140426636 ) ) ;
#9324 = CARTESIAN_POINT ( 'NONE',  ( -105.6099249115084575, -273.1795651454737595, -234.6305738050200773 ) ) ;
#9325 = CARTESIAN_POINT ( 'NONE',  ( 33.98376699622755126, -276.6350916942104163, -252.6432959120383259 ) ) ;
#9326 = CARTESIAN_POINT ( 'NONE',  ( 3.153523199933804921, -290.6186907111285223, -207.5943450251776596 ) ) ;
#9327 = CARTESIAN_POINT ( 'NONE',  ( -8.802341622391294251, -273.2288335437097544, -202.6856419010590002 ) ) ;
#9328 = VERTEX_POINT ( 'NONE', #3506 ) ;
#9329 = ORIENTED_EDGE ( 'NONE', *, *, #40401, .T. ) ;
#9330 = CARTESIAN_POINT ( 'NONE',  ( 180.5468918863934960, 256.3577768311903355, -167.2605672291198857 ) ) ;
#9331 = CARTESIAN_POINT ( 'NONE',  ( -44.18054286001340358, -287.8851514045184103, -196.2359236978707315 ) ) ;
#9332 = CARTESIAN_POINT ( 'NONE',  ( -99.74891817102903246, -297.0379659272837785, -315.0244331584569295 ) ) ;
#9333 = CARTESIAN_POINT ( 'NONE',  ( -95.85250664052482250, -285.8178224404293815, -226.5389981144259082 ) ) ;
#9334 = CARTESIAN_POINT ( 'NONE',  ( -84.73057161874488941, -276.7456623870044155, -330.8200186737783497 ) ) ;
#9335 = CARTESIAN_POINT ( 'NONE',  ( 15.36225741254725286, -293.4246494547327302, -214.2915341415307751 ) ) ;
#9336 = CARTESIAN_POINT ( 'NONE',  ( 34.76481083387752591, -285.9890037049091802, -293.6195907857422185 ) ) ;
#9337 = CARTESIAN_POINT ( 'NONE',  ( 4.219455850647682027, -294.8419587714506633, -335.2190530474730963 ) ) ;
#9338 = CARTESIAN_POINT ( 'NONE',  ( -99.73187561860062544, -291.4078247623962739, -232.4196698157836352 ) ) ;
#9339 = DIRECTION ( 'NONE',  ( 0.000000000000000000, 0.000000000000000000, 1.000000000000000000 ) ) ;
#9340 = CARTESIAN_POINT ( 'NONE',  ( -113.5000000000000568, -298.0521521680024080, -397.9547385950631337 ) ) ;
#9341 = CARTESIAN_POINT ( 'NONE',  ( 168.1374001854913161, 229.6528827648448328, -190.0556063143384335 ) ) ;
#9342 = CARTESIAN_POINT ( 'NONE',  ( -111.8439212269905028, -285.8640842813732093, -286.8573844371703103 ) ) ;
#9343 = CARTESIAN_POINT ( 'NONE',  ( -37.30987171927208834, -295.5523547857347353, -195.3611179825600175 ) ) ;
#9344 = ORIENTED_EDGE ( 'NONE', *, *, #48992, .T. ) ;
#9345 = CARTESIAN_POINT ( 'NONE',  ( -109.2854881134171734, -283.2874891543556828, -284.4436406515244471 ) ) ;
#9346 = CARTESIAN_POINT ( 'NONE',  ( -104.9590386008110983, -277.7426348631080941, -307.1529625857808696 ) ) ;
#9347 = CARTESIAN_POINT ( 'NONE',  ( 35.73611740963192318, -283.7596727182389031, -286.4751185696181892 ) ) ;
#9348 = CARTESIAN_POINT ( 'NONE',  ( 169.7292685188034227, 230.4183104143901062, -191.5860846049169197 ) ) ;
#9349 = CARTESIAN_POINT ( 'NONE',  ( -85.74325200706886108, -282.2820553938334456, -329.4872210758128404 ) ) ;
#9350 = CARTESIAN_POINT ( 'NONE',  ( 34.25459885592858456, -285.2985038511157541, -249.2016013927953964 ) ) ;
#9351 = CARTESIAN_POINT ( 'NONE',  ( 21.77938134748067966, -276.7672742108748025, -222.9590885080746432 ) ) ;
#9352 = CARTESIAN_POINT ( 'NONE',  ( -110.1122087153026143, -297.1375724696620750, -263.2999384606431477 ) ) ;
#9353 = EDGE_CURVE ( 'NONE', #42812, #91222, #48447, .T. ) ;
#9354 = CARTESIAN_POINT ( 'NONE',  ( 36.11476244439325711, -292.2065457862624953, -268.0391397338300408 ) ) ;
#9355 = CARTESIAN_POINT ( 'NONE',  ( -89.13732877151714717, -278.4097586906273705, -327.1988311645158092 ) ) ;
#9356 = CARTESIAN_POINT ( 'NONE',  ( -48.60784014164740796, -277.1994615326570965, -342.5379122864406440 ) ) ;
#9357 = CARTESIAN_POINT ( 'NONE',  ( -46.11491558741615648, -298.8846996149286497, -194.0993916506022856 ) ) ;
#9358 = CARTESIAN_POINT ( 'NONE',  ( -86.90594116065956598, -276.6432078885947590, -328.9530741798733970 ) ) ;
#9359 = CARTESIAN_POINT ( 'NONE',  ( 202.9737692553709962, 295.9636489462768054, -68.65455572929471373 ) ) ;
#9360 = CARTESIAN_POINT ( 'NONE',  ( -69.88068506323564577, -275.4804950842052449, -337.9488520313279878 ) ) ;
#9361 = EDGE_CURVE ( 'NONE', #49098, #200, #83490, .T. ) ;
#9362 = CARTESIAN_POINT ( 'NONE',  ( 20.93015744612140239, -295.6487743138541191, -319.7878001415969038 ) ) ;
#9363 = DIRECTION ( 'NONE',  ( 0.7806247497998687335, 0.000000000000000000, 0.6249999999999139577 ) ) ;
#9364 = CIRCLE ( 'NONE', #22964, 20.00000000000000000 ) ;
#9365 = CARTESIAN_POINT ( 'NONE',  ( 211.1232656141943949, 0.000000000000000000, -7.000000000000000000 ) ) ;
#9366 = CARTESIAN_POINT ( 'NONE',  ( -97.77942276236090891, -285.0556220006229751, -311.9406250675800720 ) ) ;
#9367 = CARTESIAN_POINT ( 'NONE',  ( -71.26595434794067785, -285.2540185525364222, -338.3546396788050288 ) ) ;
#9368 = CARTESIAN_POINT ( 'NONE',  ( 15.10840051377569715, -286.1655619060246067, -219.4407918758481344 ) ) ;
#9369 = CARTESIAN_POINT ( 'NONE',  ( -98.64692345768735038, -277.5176028380968205, -229.1837950430018225 ) ) ;
#9370 = CARTESIAN_POINT ( 'NONE',  ( -109.8768178802355919, -286.6182510395533996, -254.5054146310430383 ) ) ;
#9371 = CARTESIAN_POINT ( 'NONE',  ( -35.62744554201038483, -278.5538885771593414, -196.6752029966957593 ) ) ;
#9372 = CARTESIAN_POINT ( 'NONE',  ( -64.43464373333104334, -278.4938122583737368, -338.5340249355006677 ) ) ;
#9373 = FACE_OUTER_BOUND ( 'NONE', #57966, .T. ) ;
#9374 = CARTESIAN_POINT ( 'NONE',  ( -48.89134119960048963, -274.3935443852893741, -198.1670271450167604 ) ) ;
#9375 = AXIS2_PLACEMENT_3D ( 'NONE', #65024, #22357, #14810 ) ;
#9376 = CARTESIAN_POINT ( 'NONE',  ( 29.14174062027015921, -281.8529327494938457, -231.8369576884314256 ) ) ;
#9377 = PRODUCT_DEFINITION ( 'UNKNOWN', '', #37123, #92065 ) ;
#9378 = CARTESIAN_POINT ( 'NONE',  ( 36.53887046323130505, -281.7744392365738690, -248.8386078375712316 ) ) ;
#9379 = ORIENTED_EDGE ( 'NONE', *, *, #41133, .F. ) ;
#9380 = ORIENTED_EDGE ( 'NONE', *, *, #53233, .F. ) ;
#9381 = CARTESIAN_POINT ( 'NONE',  ( 120.8395553409046528, -299.5541904835127980, -197.5480973984245168 ) ) ;
#9382 = CARTESIAN_POINT ( 'NONE',  ( 33.91892579954672016, -289.7445942240782415, -296.2476975210049659 ) ) ;
#9383 = CARTESIAN_POINT ( 'NONE',  ( -107.6116207925811352, -296.0180866902563821, -249.9959522083234162 ) ) ;
#9384 = CARTESIAN_POINT ( 'NONE',  ( 17.42284735118061434, -292.1577082024437004, -216.3031949670192375 ) ) ;
#9385 = CARTESIAN_POINT ( 'NONE',  ( 32.50384318475535395, -285.7227723736917255, -246.8598875580085235 ) ) ;
#9386 = CARTESIAN_POINT ( 'NONE',  ( 32.87037456973008176, -286.4186139456267597, -292.5678098937314644 ) ) ;
#9387 = CARTESIAN_POINT ( 'NONE',  ( 18.06591383834199860, -288.0746774278188695, -222.2245744819838649 ) ) ;
#9388 = CARTESIAN_POINT ( 'NONE',  ( -110.5382276462480746, -276.3420841287217513, -286.7094822062604749 ) ) ;
#9389 = CARTESIAN_POINT ( 'NONE',  ( 0.3061181238226263757, -286.9596750936422040, -336.6708858315362818 ) ) ;
#9390 = CARTESIAN_POINT ( 'NONE',  ( -63.86438439859188065, -287.7064970884492823, -200.1935717889540456 ) ) ;
#9391 = CARTESIAN_POINT ( 'NONE',  ( -51.36876014307293303, -287.2309533524947938, -344.2073772716512963 ) ) ;
#9392 = CARTESIAN_POINT ( 'NONE',  ( 21.20520556334179929, -283.1094260327879510, -314.3780755328174905 ) ) ;
#9393 = CARTESIAN_POINT ( 'NONE',  ( -71.36575023778237892, -293.6041527637054287, -203.3215524616446714 ) ) ;
#9394 = CARTESIAN_POINT ( 'NONE',  ( 204.5044540939250055, -147.7221692137691775, 10.75739200365177695 ) ) ;
#9395 = LINE ( 'NONE', #66263, #77580 ) ;
#9396 = CARTESIAN_POINT ( 'NONE',  ( -112.7942526783575516, -298.4097371523959623, -275.2706406738089413 ) ) ;
#9397 = CARTESIAN_POINT ( 'NONE',  ( 33.61469190428632459, -280.5139669131145297, -252.4834640556606473 ) ) ;
#9398 = CARTESIAN_POINT ( 'NONE',  ( 6.747804008366109940, -280.4522460350520987, -331.0333214281962455 ) ) ;
#9399 = CARTESIAN_POINT ( 'NONE',  ( 6.513436402753930210, -293.6702768332052642, -333.5202053665329913 ) ) ;
#9400 = CARTESIAN_POINT ( 'NONE',  ( -77.08980148549616729, -271.7512966860838333, -207.9266527333860495 ) ) ;
#9401 = CARTESIAN_POINT ( 'NONE',  ( 6.220049248655174168, -274.5359313369930305, -330.7877276881820308 ) ) ;
#9402 = CARTESIAN_POINT ( 'NONE',  ( -4.098710172409132824, -295.9195122302720051, -335.9202126317778152 ) ) ;
#9403 = DIRECTION ( 'NONE',  ( 0.000000000000000000, 0.000000000000000000, 1.000000000000000000 ) ) ;
#9404 = CARTESIAN_POINT ( 'NONE',  ( -93.69831990971792379, -271.8343379430217510, -218.7420208060979974 ) ) ;
#9405 = CARTESIAN_POINT ( 'NONE',  ( -97.48631844581680639, -294.1639130578289496, -316.8003137591177847 ) ) ;
#9406 = CARTESIAN_POINT ( 'NONE',  ( -12.07480611750736799, -293.8126527156005068, -201.1912628995287946 ) ) ;
#9407 = LINE ( 'NONE', #9886, #56602 ) ;
#9408 = CARTESIAN_POINT ( 'NONE',  ( -0.01734373234466295849, -293.3655432072883968, -207.4366064895172599 ) ) ;
#9409 = FACE_OUTER_BOUND ( 'NONE', #43730, .T. ) ;
#9411 = CARTESIAN_POINT ( 'NONE',  ( 14.31627945125103629, -294.3013321230193924, -322.0117731805708559 ) ) ;
#9410 = CARTESIAN_POINT ( 'NONE',  ( -112.2710970162148101, -282.4700302973818680, -278.3606356837190106 ) ) ;
#9412 = CARTESIAN_POINT ( 'NONE',  ( 38.42557020330212225, -281.7246931477653220, -284.1573547824448269 ) ) ;
#9413 = CARTESIAN_POINT ( 'NONE',  ( -17.39608807173466332, -282.2277362880728333, -197.4811704312260758 ) ) ;
#9414 = CARTESIAN_POINT ( 'NONE',  ( -107.9050482121129448, -284.6127052516715707, -239.4616675676830653 ) ) ;
#9415 = CARTESIAN_POINT ( 'NONE',  ( -107.7662954873343182, -288.2232244660248170, -295.6673384357686700 ) ) ;
#9416 = CARTESIAN_POINT ( 'NONE',  ( -20.19161114001082069, -271.7666405000204577, -195.3683826091709363 ) ) ;
#9417 = CARTESIAN_POINT ( 'NONE',  ( -24.66797078881636907, -281.3732731368497184, -345.6615672673524955 ) ) ;
#9418 = CARTESIAN_POINT ( 'NONE',  ( -14.39624385009643426, -285.0406471295142978, -200.4883300999165954 ) ) ;
#9419 = CARTESIAN_POINT ( 'NONE',  ( -112.6188907879411687, -289.6573926183591539, -255.6354476039742849 ) ) ;
#9420 = CARTESIAN_POINT ( 'NONE',  ( 206.9189553108847406, 30.70889394204682787, 14.50000000000000000 ) ) ;
#9421 = CARTESIAN_POINT ( 'NONE',  ( 16.75931787345694346, -295.8658678766325920, -320.5559410893037011 ) ) ;
#9422 = CARTESIAN_POINT ( 'NONE',  ( -103.0894641370723974, -279.4651095680663389, -309.3985989646350276 ) ) ;
#9424 = CARTESIAN_POINT ( 'NONE',  ( 11.32306847253002857, -280.4158516843758662, -215.9200692808280451 ) ) ;
#9423 = CARTESIAN_POINT ( 'NONE',  ( 5.654382319007485336, -292.4934067197319791, -332.3096068555218494 ) ) ;
#9425 = CARTESIAN_POINT ( 'NONE',  ( 34.45225792870877513, -294.0714351290135937, -298.1932503304552142 ) ) ;
#9426 = CARTESIAN_POINT ( 'NONE',  ( -43.52360509942221967, -284.0546177066939890, -195.0021606904724081 ) ) ;
#9427 = CARTESIAN_POINT ( 'NONE',  ( -35.72831347859996498, -279.0321009685991953, -345.3565492688085783 ) ) ;
#9428 = CARTESIAN_POINT ( 'NONE',  ( -15.53415644707979126, -293.8217661629800546, -340.3275428985779740 ) ) ;
#9429 = CIRCLE ( 'NONE', #62386, 1.000000000000000000 ) ;
#9430 = CARTESIAN_POINT ( 'NONE',  ( -112.3496288967640879, -270.6240362761600977, -264.7374179722997951 ) ) ;
#9431 = VERTEX_POINT ( 'NONE', #47514 ) ;
#9432 = CARTESIAN_POINT ( 'NONE',  ( 203.5977283565847813, 62.01285785379747040, -6.999999999999999112 ) ) ;
#9434 = CARTESIAN_POINT ( 'NONE',  ( 3.585205170984413936, -282.5850915640243102, -207.8744732089052718 ) ) ;
#9433 = AXIS2_PLACEMENT_3D ( 'NONE', #66174, #52406, #37719 ) ;
#9435 = CARTESIAN_POINT ( 'NONE',  ( -58.43198869703611109, -294.8399360726095892, -340.3124451293195420 ) ) ;
#9436 = DIRECTION ( 'NONE',  ( -1.000000000000000000, 0.000000000000000000, 0.000000000000000000 ) ) ;
#9437 = CARTESIAN_POINT ( 'NONE',  ( -20.25526795762938548, -280.3380690714491266, -345.3683826091709648 ) ) ;
#9438 = CARTESIAN_POINT ( 'NONE',  ( -94.01923303865451942, -272.4566771834714132, -218.4589795183534022 ) ) ;
#9439 = CARTESIAN_POINT ( 'NONE',  ( 38.06792231139792904, -288.7038455710182348, -257.3734082591798824 ) ) ;
#9440 = CARTESIAN_POINT ( 'NONE',  ( -109.2763902914211513, -290.5531949438906736, -257.6467586588815379 ) ) ;
#9441 = VECTOR ( 'NONE', #91403, 1000.000000000000000 ) ;
#9442 = CARTESIAN_POINT ( 'NONE',  ( -43.83125591036727542, -281.4889182350472083, -196.9033676322069084 ) ) ;
#9443 = CARTESIAN_POINT ( 'NONE',  ( -68.64019928937229054, -275.2339793804651435, -203.5128137329799074 ) ) ;
#9444 = CARTESIAN_POINT ( 'NONE',  ( 5.165534353092529507, -279.4364851505123966, -210.5257979733775358 ) ) ;
#9445 = ORIENTED_EDGE ( 'NONE', *, *, #54191, .F. ) ;
#9446 = CARTESIAN_POINT ( 'NONE',  ( 9.512021383094186433, -274.5099932745846445, -209.2568727532990067 ) ) ;
#9447 = CARTESIAN_POINT ( 'NONE',  ( -69.66456076751934745, -293.5435032731721208, -203.2907444164762580 ) ) ;
#9448 = LINE ( 'NONE', #9925, #5245 ) ;
#9449 = CARTESIAN_POINT ( 'NONE',  ( 160.5350683151633291, 250.0000000000000568, 24.72542485937378842 ) ) ;
#9450 = B_SPLINE_CURVE_WITH_KNOTS ( 'NONE', 3,
 ( #30884, #59299, #60235, #88619, #23766, #44605, #75359, #53098, #9544, #52631, #81511, #80589, #38430, #2919, #31347, #45056 ),
 .UNSPECIFIED., .F., .F.,
 ( 4, 2, 2, 2, 2, 2, 2, 4 ),
 ( 0.000000000000000000, 0.0005475143912465603533, 0.001095028782493120707, 0.001642543173739681060, 0.002190057564986241413, 0.002737571956232801550, 0.003285086347479362120, 0.004380115129972482826 ),
 .UNSPECIFIED. ) ;
#9451 = CARTESIAN_POINT ( 'NONE',  ( 35.52287402197072197, -291.4267013884627318, -249.5518240744340801 ) ) ;
#9452 = CARTESIAN_POINT ( 'NONE',  ( -110.2497162214860822, -272.1317480020769040, -264.9026157334960772 ) ) ;
#9453 = DIRECTION ( 'NONE',  ( 0.000000000000000000, 0.000000000000000000, 1.000000000000000000 ) ) ;
#9454 = CARTESIAN_POINT ( 'NONE',  ( -113.3184584092758769, -292.1686304840458774, -262.7257586349020357 ) ) ;
#9455 = CARTESIAN_POINT ( 'NONE',  ( -37.37352853689063181, -294.5519495502701375, -190.3611179825600175 ) ) ;
#9456 = CARTESIAN_POINT ( 'NONE',  ( -33.16108494954359287, -288.1049510632423107, -195.5935759879883449 ) ) ;
#9457 = CARTESIAN_POINT ( 'NONE',  ( 36.92228243610966842, -273.6758569549191407, -279.9867987363098791 ) ) ;
#9458 = CARTESIAN_POINT ( 'NONE',  ( 21.81121262166312746, -276.8487912599250649, -225.1489165455837735 ) ) ;
#9459 = CARTESIAN_POINT ( 'NONE',  ( 30.05242332892795432, -291.2118248548381416, -238.6269397304359359 ) ) ;
#9460 = CARTESIAN_POINT ( 'NONE',  ( -33.99394332330222568, -281.9542575672364251, -194.6703126847654346 ) ) ;
#9461 = CIRCLE ( 'NONE', #59449, 2.999999999999999556 ) ;
#9462 = ORIENTED_EDGE ( 'NONE', *, *, #83602, .F. ) ;
#9463 = CARTESIAN_POINT ( 'NONE',  ( 1.147934986711255156, -281.8723990899705427, -332.5687598379224710 ) ) ;
#9464 = CARTESIAN_POINT ( 'NONE',  ( -113.7698113889289999, -279.5444806902247024, -277.3167785949152631 ) ) ;
#9465 = CARTESIAN_POINT ( 'NONE',  ( 23.08020642156183300, -280.9796477978960638, -317.4694837491276758 ) ) ;
#9466 = CARTESIAN_POINT ( 'NONE',  ( -93.15465407850270196, -278.7708410684625733, -323.1415971877929678 ) ) ;
#9467 = DIRECTION ( 'NONE',  ( 1.000000000000000000, 0.000000000000000000, 0.000000000000000000 ) ) ;
#9468 = CARTESIAN_POINT ( 'NONE',  ( 3.150145769630703807, -278.0392902086244362, -335.1003557875072829 ) ) ;
#9469 = CARTESIAN_POINT ( 'NONE',  ( 27.36219212280431989, -290.4805209788416391, -301.4846348637938149 ) ) ;
#9470 = ORIENTED_EDGE ( 'NONE', *, *, #74672, .F. ) ;
#9471 = CARTESIAN_POINT ( 'NONE',  ( -108.6151890816451555, -298.8558147292780518, -246.8491257729131121 ) ) ;
#9472 = CARTESIAN_POINT ( 'NONE',  ( -110.6145881170797338, -291.5848479143420491, -273.9376898259026802 ) ) ;
#9473 = CARTESIAN_POINT ( 'NONE',  ( -5.599580795686239121, -274.6527245038339515, -337.9346838064539043 ) ) ;
#9474 = CARTESIAN_POINT ( 'NONE',  ( 0.2379153472877099940, -290.3194023438956037, -336.4641059641636502 ) ) ;
#9475 = CARTESIAN_POINT ( 'NONE',  ( -101.2087008305070981, -290.3876129906558390, -234.6917518073010172 ) ) ;
#9476 = CARTESIAN_POINT ( 'NONE',  ( 38.49726714829844809, -286.8966162944844882, -257.3229458393884670 ) ) ;
#9477 = DIRECTION ( 'NONE',  ( -0.000000000000000000, -1.000000000000000000, -0.000000000000000000 ) ) ;
#9478 = CARTESIAN_POINT ( 'NONE',  ( -110.6700310492390003, -282.8375507055343405, -279.1334383318287564 ) ) ;
#9479 = CARTESIAN_POINT ( 'NONE',  ( -96.74268996601836079, -291.7977083417767972, -314.9063381743656578 ) ) ;
#9480 = CARTESIAN_POINT ( 'NONE',  ( -103.6448513711170278, -282.5993002788165995, -302.6435727770219160 ) ) ;
#9481 = CARTESIAN_POINT ( 'NONE',  ( 22.50541189448504653, -282.2754232012916304, -227.7047390776429552 ) ) ;
#9482 = CARTESIAN_POINT ( 'NONE',  ( 38.74047069050961767, -288.3652710480009205, -260.1472305566273349 ) ) ;
#9483 = CARTESIAN_POINT ( 'NONE',  ( -83.48145137529853343, -279.8922531219755001, -213.6466087886844036 ) ) ;
#9484 = CARTESIAN_POINT ( 'NONE',  ( -2.224125328174093141, -291.3013735828918698, -202.2673093764281873 ) ) ;
#9485 = CARTESIAN_POINT ( 'NONE',  ( -32.32718939472812991, -286.9166714291579297, -193.6732539625215850 ) ) ;
#9486 = CARTESIAN_POINT ( 'NONE',  ( 0.6943330428560532397, -289.0518129433099261, -337.3002235550299588 ) ) ;
#9487 = CARTESIAN_POINT ( 'NONE',  ( -80.62442908483677684, -283.8240825678217902, -329.2084055579150004 ) ) ;
#9488 = EDGE_LOOP ( 'NONE', ( #43064, #86296, #46913, #72753 ) ) ;
#9489 = CARTESIAN_POINT ( 'NONE',  ( 208.4306832106270804, -125.2391364535880882, 7.500000000000012434 ) ) ;
#9490 = CARTESIAN_POINT ( 'NONE',  ( 35.50983018896830856, -295.1469322956708652, -249.5062068842898668 ) ) ;
#9491 = AXIS2_PLACEMENT_3D ( 'NONE', #53186, #17220, #27472 ) ;
#9492 = CARTESIAN_POINT ( 'NONE',  ( -8.589013747690593448, -293.3685946375959475, -341.3156187562711352 ) ) ;
#9493 = CARTESIAN_POINT ( 'NONE',  ( -74.14184375902216573, -276.6129697035595996, -333.6790291688340631 ) ) ;
#9494 = CARTESIAN_POINT ( 'NONE',  ( -105.1597938471894622, -296.3710902508544223, -233.9987829939236121 ) ) ;
#9495 = CARTESIAN_POINT ( 'NONE',  ( 34.11364144979955881, -292.2676591057815472, -288.3844893160392644 ) ) ;
#9496 = CARTESIAN_POINT ( 'NONE',  ( -96.07977523306759338, -295.4171107106524801, -225.3092351886646725 ) ) ;
#9497 = CARTESIAN_POINT ( 'NONE',  ( -70.41329951488975780, -292.8111405176712765, -204.8370779666246335 ) ) ;
#9498 = CARTESIAN_POINT ( 'NONE',  ( 26.49700095824392321, -294.1393480828650127, -234.2179915113005393 ) ) ;
#9499 = DIRECTION ( 'NONE',  ( -1.000000000000000000, 0.000000000000000000, 0.000000000000000000 ) ) ;
#9500 = AXIS2_PLACEMENT_3D ( 'NONE', #35832, #92640, #73570 ) ;
#9501 = CARTESIAN_POINT ( 'NONE',  ( -68.78479238207643220, -293.4643346603442637, -338.6493661170446217 ) ) ;
#9502 = CARTESIAN_POINT ( 'NONE',  ( -28.90822910419799285, -300.1578788866440846, -195.3582340379268487 ) ) ;
#9503 = CARTESIAN_POINT ( 'NONE',  ( 34.75543000370136326, -288.6625238938570988, -283.2223883440931331 ) ) ;
#9504 = COLOUR_RGB ( '',0.7921568627450980005, 0.8196078431372548767, 0.9333333333333333481 ) ;
#9505 = VECTOR ( 'NONE', #81174, 1000.000000000000000 ) ;
#9506 = CARTESIAN_POINT ( 'NONE',  ( 18.67184088299908140, -278.2313260657311957, -320.7876779903811553 ) ) ;
#9507 = CARTESIAN_POINT ( 'NONE',  ( -91.06157840015363547, -276.5893136465502380, -325.0447860595913880 ) ) ;
#9508 = CARTESIAN_POINT ( 'NONE',  ( -99.47977570931168145, -272.5038024858304198, -224.9719255903343935 ) ) ;
#9509 = CARTESIAN_POINT ( 'NONE',  ( 34.71128871121850068, -279.8746842424320107, -289.1115847744714529 ) ) ;
#9510 = CARTESIAN_POINT ( 'NONE',  ( -45.58355504442788941, -275.5546819062440704, -346.1665942128354914 ) ) ;
#9511 = AXIS2_PLACEMENT_3D ( 'NONE', #18831, #24049, #74242 ) ;
#9512 = CARTESIAN_POINT ( 'NONE',  ( -73.55992231105126677, -294.2284233043565678, -334.3101903791263680 ) ) ;
#9513 = DIRECTION ( 'NONE',  ( 0.000000000000000000, -1.000000000000000000, 0.000000000000000000 ) ) ;
#9514 = CARTESIAN_POINT ( 'NONE',  ( -64.61450876430727419, -274.3378719868794064, -202.5236804764352030 ) ) ;
#9515 = CARTESIAN_POINT ( 'NONE',  ( 196.2226125757317163, 24.40159866106579400, 11.63920816608860243 ) ) ;
#9517 = CARTESIAN_POINT ( 'NONE',  ( 27.86223874192444683, -274.9399759604181668, -237.5366399163407891 ) ) ;
#9516 = CARTESIAN_POINT ( 'NONE',  ( -96.16348885126021173, -289.2169844236783547, -223.2611818973692266 ) ) ;
#9518 = CARTESIAN_POINT ( 'NONE',  ( -103.7984261479585228, -290.0447901394413748, -309.3574989870229501 ) ) ;
#9519 = CARTESIAN_POINT ( 'NONE',  ( -112.0435739941657403, -274.6592404272614090, -262.0149532151006611 ) ) ;
#9520 = CARTESIAN_POINT ( 'NONE',  ( -101.7572472965752013, -294.0403003499689021, -308.5508139450483895 ) ) ;
#9521 = EDGE_CURVE ( 'NONE', #30328, #76803, #33724, .T. ) ;
#9522 = CARTESIAN_POINT ( 'NONE',  ( -93.32091865446615486, -283.0292447186187133, -323.0158156954145170 ) ) ;
#9523 = ADVANCED_FACE ( 'NONE', ( #69776 ), #47343, .T. ) ;
#9524 = CARTESIAN_POINT ( 'NONE',  ( 152.4536156746142410, 250.5000000000000568, 12.00000000000000000 ) ) ;
#9525 = CARTESIAN_POINT ( 'NONE',  ( 35.94179950145240809, -279.7576011828080027, -286.3742222304793472 ) ) ;
#9526 = CIRCLE ( 'NONE', #18677, 4.000000000000003553 ) ;
#9527 = FACE_BOUND ( 'NONE', #57454, .T. ) ;
#9528 = CARTESIAN_POINT ( 'NONE',  ( -75.17117814374545048, -290.3311724257180231, -207.4045619966211973 ) ) ;
#9529 = CARTESIAN_POINT ( 'NONE',  ( -43.05116421143137018, -281.2644270251465173, -344.4273711321836231 ) ) ;
#9530 = CARTESIAN_POINT ( 'NONE',  ( 198.4456942626906368, 41.56718807020170203, 10.77776320379719444 ) ) ;
#9531 = LINE ( 'NONE', #58823, #50347 ) ;
#9532 = CARTESIAN_POINT ( 'NONE',  ( -95.83515293023801007, -289.1979716293355978, -223.3990880863079553 ) ) ;
#9533 = CARTESIAN_POINT ( 'NONE',  ( -27.21386722455003593, -275.7031927505482258, -197.3156636692561676 ) ) ;
#9534 = CARTESIAN_POINT ( 'NONE',  ( -69.00822795820450040, -284.6644545443642755, -340.1267266683782395 ) ) ;
#9536 = CARTESIAN_POINT ( 'NONE',  ( -100.9913200069670296, -285.0424895279036832, -234.5122320193257792 ) ) ;
#9535 = CARTESIAN_POINT ( 'NONE',  ( -34.13928655502773069, -272.1719845320087074, -194.8690074849444898 ) ) ;
#9537 = CARTESIAN_POINT ( 'NONE',  ( 20.49675419209061644, -277.6142700564980714, -315.8796384092860876 ) ) ;
#9538 = CARTESIAN_POINT ( 'NONE',  ( -68.09601417438385340, -278.2694544743675920, -336.7584312091295260 ) ) ;
#9539 = CARTESIAN_POINT ( 'NONE',  ( -107.1758150725308241, -286.9099069766326693, -242.8665648304010460 ) ) ;
#9540 = ORIENTED_EDGE ( 'NONE', *, *, #63681, .T. ) ;
#9541 = DIRECTION ( 'NONE',  ( -0.000000000000000000, 1.000000000000000000, -0.000000000000000000 ) ) ;
#9542 = CARTESIAN_POINT ( 'NONE',  ( -93.69091745377926372, -295.6699649583649148, -322.8568726151731312 ) ) ;
#9543 = CARTESIAN_POINT ( 'NONE',  ( -10.17431246740073902, -288.3884020661536738, -200.8218995084926632 ) ) ;
#9544 = CARTESIAN_POINT ( 'NONE',  ( 195.9349804655796277, 25.71257817237890109, 14.38313153394006605 ) ) ;
#9545 = CARTESIAN_POINT ( 'NONE',  ( -72.08107566293803359, -286.9809262143061233, -342.4248175857292154 ) ) ;
#9546 = CARTESIAN_POINT ( 'NONE',  ( -112.7641495822103792, -277.2971579571951111, -284.3238613800242547 ) ) ;
#9547 = CARTESIAN_POINT ( 'NONE',  ( -2.404286826974449287, -290.9063848176224951, -202.6278273392493361 ) ) ;
#9548 = CARTESIAN_POINT ( 'NONE',  ( -84.10261485729554920, -286.9162846033334517, -213.3375839668977392 ) ) ;
#9549 = CARTESIAN_POINT ( 'NONE',  ( -38.39042639563859893, -281.7989750584970920, -196.3426382076160905 ) ) ;
#9550 = CARTESIAN_POINT ( 'NONE',  ( -7.589438515866753221, -287.8597349408465789, -199.9244425422143934 ) ) ;
#9551 = CARTESIAN_POINT ( 'NONE',  ( -23.67677284669430904, -284.8776729323631116, -344.1057476738113792 ) ) ;
#9552 = CARTESIAN_POINT ( 'NONE',  ( 18.90466005522554127, -276.4360532191820994, -322.9476844291065731 ) ) ;
#9553 = CARTESIAN_POINT ( 'NONE',  ( -97.40924347634015135, -295.1799316593315439, -226.0254753265287206 ) ) ;
#9554 = CARTESIAN_POINT ( 'NONE',  ( -104.7925647195064727, -278.8665227833717495, -233.2211008802947561 ) ) ;
#9556 = CARTESIAN_POINT ( 'NONE',  ( -34.43343589471964350, -300.0089847519888622, -195.9201493502285985 ) ) ;
#9555 = AXIS2_PLACEMENT_3D ( 'NONE', #82064, #56365, #74989 ) ;
#9557 = DIRECTION ( 'NONE',  ( -0.000000000000000000, -0.000000000000000000, -1.000000000000000000 ) ) ;
#9558 = DIRECTION ( 'NONE',  ( -1.000000000000000000, 0.000000000000000000, 0.000000000000000000 ) ) ;
#9559 = CARTESIAN_POINT ( 'NONE',  ( -113.3283667958448859, -270.7922942169334988, -270.3387572857972145 ) ) ;
#9560 = CARTESIAN_POINT ( 'NONE',  ( 197.2116943569230045, 215.0000000000000568, -12.92446933126075592 ) ) ;
#9561 = CARTESIAN_POINT ( 'NONE',  ( -108.5476548306190523, -277.8434185245061485, -286.7781366562203402 ) ) ;
#9562 = CIRCLE ( 'NONE', #86690, 20.15985230015483154 ) ;
#9563 = CARTESIAN_POINT ( 'NONE',  ( -55.25572410665161982, -275.0317299028056937, -195.8822856719018546 ) ) ;
#9564 = CARTESIAN_POINT ( 'NONE',  ( -1.753895159114033486, -281.6510032957936005, -338.3782360564489409 ) ) ;
#9565 = CARTESIAN_POINT ( 'NONE',  ( -72.82525072372939690, -291.2891930513913508, -335.3141136941061404 ) ) ;
#9566 = CARTESIAN_POINT ( 'NONE',  ( -48.88439730649810855, -299.4279394921284165, -194.8793321862684138 ) ) ;
#9567 = CARTESIAN_POINT ( 'NONE',  ( -95.27111034232653708, -297.0765878341701978, -320.4828912119334632 ) ) ;
#9568 = CARTESIAN_POINT ( 'NONE',  ( 22.44349852126331868, -294.9357139585002869, -225.3526915261700196 ) ) ;
#9569 = CARTESIAN_POINT ( 'NONE',  ( 8.907515791671118066, -280.4163668843435175, -329.2578714169447380 ) ) ;
#9570 = CIRCLE ( 'NONE', #62537, 1.897123461337413275 ) ;
#9571 = CARTESIAN_POINT ( 'NONE',  ( -24.65454250923442103, -282.1354596386078128, -197.0102473204980242 ) ) ;
#9572 = CARTESIAN_POINT ( 'NONE',  ( -78.28397095592997346, -295.5769831587709291, -208.1297061412503240 ) ) ;
#9573 = CARTESIAN_POINT ( 'NONE',  ( -109.9173159969080587, -285.8567699480836382, -293.6252306047210823 ) ) ;
#9574 = CARTESIAN_POINT ( 'NONE',  ( 12.35529499789633867, -287.2611780074056469, -324.3228928726314280 ) ) ;
#9575 = CARTESIAN_POINT ( 'NONE',  ( -102.7707769666400281, -256.8657757996624582, -326.5951631694345565 ) ) ;
#9576 = EDGE_LOOP ( 'NONE', ( #65271, #50235, #69335, #68879 ) ) ;
#9577 = CARTESIAN_POINT ( 'NONE',  ( -40.33399641314547779, -287.6637787920037681, -346.7262601866163436 ) ) ;
#9578 = CARTESIAN_POINT ( 'NONE',  ( 28.83090566339503269, -286.8020831496699543, -239.4859867367827917 ) ) ;
#9579 = ORIENTED_EDGE ( 'NONE', *, *, #74557, .T. ) ;
#9580 = CARTESIAN_POINT ( 'NONE',  ( -76.58784257588565936, -284.6436472105988855, -336.3107154012035949 ) ) ;
#9581 = AXIS2_PLACEMENT_3D ( 'NONE', #23741, #25139, #16177 ) ;
#9582 = CARTESIAN_POINT ( 'NONE',  ( 33.85342694397820651, -275.6707604746904963, -254.0774322510782497 ) ) ;
#9583 = CARTESIAN_POINT ( 'NONE',  ( -27.87356325090788900, -291.0898816066291488, -194.2034736890373097 ) ) ;
#9584 = CARTESIAN_POINT ( 'NONE',  ( 36.49951349824269897, -281.9334795679911849, -248.8479575381061863 ) ) ;
#9585 = CARTESIAN_POINT ( 'NONE',  ( 21.42425918968850596, -282.4119547273760418, -221.6859725747800098 ) ) ;
#9586 = CARTESIAN_POINT ( 'NONE',  ( 17.20513261849135489, -281.1375432829694887, -215.9689100848758017 ) ) ;
#9587 = CARTESIAN_POINT ( 'NONE',  ( -9.247346698079034866, -280.4299762035796562, -202.9837678910780880 ) ) ;
#9588 = CARTESIAN_POINT ( 'NONE',  ( -37.37352853689063181, -292.5523547857346784, -340.3611179825599606 ) ) ;
#9589 = CARTESIAN_POINT ( 'NONE',  ( 122.1772289462398788, 149.4124950158447973, -263.6923987309557447 ) ) ;
#9590 = ORIENTED_EDGE ( 'NONE', *, *, #40721, .F. ) ;
#9591 = CARTESIAN_POINT ( 'NONE',  ( 33.79687352975842884, -277.2497541240991268, -246.9710812992753972 ) ) ;
#9592 = CARTESIAN_POINT ( 'NONE',  ( -31.94682571628636225, -123.9324301101092090, -363.8327245793788620 ) ) ;
#9593 = CIRCLE ( 'NONE', #50435, 0.4999999999999977796 ) ;
#9594 = CARTESIAN_POINT ( 'NONE',  ( -65.96931166538414004, -281.4486690165381333, -339.3120012551716513 ) ) ;
#9595 = CARTESIAN_POINT ( 'NONE',  ( -106.8010399994768846, -296.2046685995755411, -247.4127002469209913 ) ) ;
#9596 = CARTESIAN_POINT ( 'NONE',  ( 13.24273499658139563, -292.2452640551445597, -212.3892124921750337 ) ) ;
#9597 = CARTESIAN_POINT ( 'NONE',  ( 180.2407988376923242, 251.0076156727935484, -164.4202208545905535 ) ) ;
#9599 = CARTESIAN_POINT ( 'NONE',  ( -105.8633389802770637, -288.5875474646359180, -297.9068605740301905 ) ) ;
#9598 = CARTESIAN_POINT ( 'NONE',  ( -15.00602699531519946, -296.9013540461178877, -193.9556305505829812 ) ) ;
#9600 = CARTESIAN_POINT ( 'NONE',  ( -2.544137217372268278, -296.4471605080928498, -335.9354658466741625 ) ) ;
#9601 = CARTESIAN_POINT ( 'NONE',  ( 4.995878742864167776, -287.9526293940747337, -210.2257885732047384 ) ) ;
#9602 = EDGE_LOOP ( 'NONE', ( #32888, #36068, #7692, #53755 ) ) ;
#9603 = CARTESIAN_POINT ( 'NONE',  ( 39.37218390606714991, -294.5284385272452141, -273.1540033555661466 ) ) ;
#9604 = CARTESIAN_POINT ( 'NONE',  ( -108.4268429839573002, -285.2676277954465149, -253.4285056921538057 ) ) ;
#9605 = CARTESIAN_POINT ( 'NONE',  ( -82.72293255170497162, -296.2424162609503924, -208.5817507381792097 ) ) ;
#9606 = AXIS2_PLACEMENT_3D ( 'NONE', #967, #1417, #66755 ) ;
#9607 = CARTESIAN_POINT ( 'NONE',  ( 15.32003981088454303, -293.5760444376549572, -214.3336259263829504 ) ) ;
#9608 = CARTESIAN_POINT ( 'NONE',  ( 39.16423400484711692, -293.9364249304986174, -261.7265915748383804 ) ) ;
#9609 = CARTESIAN_POINT ( 'NONE',  ( -82.54460461646614533, -289.8564400820790183, -327.6821213783204598 ) ) ;
#9610 = VERTEX_POINT ( 'NONE', #25736 ) ;
#9611 = CARTESIAN_POINT ( 'NONE',  ( 139.6539576904058606, 131.4142135623731633, -11.08578643762690241 ) ) ;
#9612 = CARTESIAN_POINT ( 'NONE',  ( -23.66215476692705266, -300.0820794693608491, -194.5920294635623691 ) ) ;
#9613 = CARTESIAN_POINT ( 'NONE',  ( -63.40748561418260465, -272.5148295702056203, -198.3292948402741160 ) ) ;
#9614 = CARTESIAN_POINT ( 'NONE',  ( 21.99556429462856499, -281.2097165398878360, -313.3069080113020277 ) ) ;
#9615 = ORIENTED_EDGE ( 'NONE', *, *, #53799, .F. ) ;
#9616 = VERTEX_POINT ( 'NONE', #11064 ) ;
#9617 = CARTESIAN_POINT ( 'NONE',  ( -95.16868428462585427, -277.3724968870231464, -321.1111604131556305 ) ) ;
#9618 = CARTESIAN_POINT ( 'NONE',  ( -87.86631430535015852, -271.7319292938724971, -216.4980116749645163 ) ) ;
#9619 = CARTESIAN_POINT ( 'NONE',  ( -109.8177735249234956, -280.6216546491324948, -254.2378388582386890 ) ) ;
#9620 = CARTESIAN_POINT ( 'NONE',  ( -62.22582171728111433, -275.5186783481403836, -340.3560777830685424 ) ) ;
#9621 = CARTESIAN_POINT ( 'NONE',  ( -90.34317137244825346, -298.4866376724843917, -219.5146078483751637 ) ) ;
#9622 = CARTESIAN_POINT ( 'NONE',  ( -94.80476720963775961, -274.1320257151780879, -224.9584267569736937 ) ) ;
#9623 = CARTESIAN_POINT ( 'NONE',  ( -113.3291995039209610, -274.3478717295945444, -267.5537497277130683 ) ) ;
#9624 = CARTESIAN_POINT ( 'NONE',  ( -0.8200461576269352237, -272.5547160917676024, -204.4330481359575913 ) ) ;
#9625 = CARTESIAN_POINT ( 'NONE',  ( 29.58670639534934566, -294.5985647998004993, -299.7631768915263706 ) ) ;
#9626 = CARTESIAN_POINT ( 'NONE',  ( -2.141750492084252500, -291.1024768445341238, -205.7222101552331139 ) ) ;
#9627 = FACE_OUTER_BOUND ( 'NONE', #58900, .T. ) ;
#9628 = CARTESIAN_POINT ( 'NONE',  ( 12.66937557499071865, -276.8685166163006102, -328.8283670206632223 ) ) ;
#9629 = CARTESIAN_POINT ( 'NONE',  ( 27.86033449979522914, -275.2732823938303000, -237.5328575219699303 ) ) ;
#9630 = CARTESIAN_POINT ( 'NONE',  ( -94.04498570814091352, -282.5346182343785131, -321.7423648691323592 ) ) ;
#9631 = CARTESIAN_POINT ( 'NONE',  ( 36.28021853227310345, -295.7465373113632268, -285.5216431374584545 ) ) ;
#9632 = CARTESIAN_POINT ( 'NONE',  ( 152.4536156746142410, 250.5000000000000568, 14.50000000000000000 ) ) ;
#9633 = CARTESIAN_POINT ( 'NONE',  ( -94.24118806243090773, -284.3985009912003648, -224.3515934724798626 ) ) ;
#9634 = CARTESIAN_POINT ( 'NONE',  ( -44.27607357025885904, -281.1393677264312032, -345.2593338798153582 ) ) ;
#9635 = ADVANCED_FACE ( 'NONE', ( #54160 ), #77348, .T. ) ;
#9636 = CARTESIAN_POINT ( 'NONE',  ( 28.39572249904824019, -273.6815862500943695, -237.2859583943369444 ) ) ;
#9637 = CARTESIAN_POINT ( 'NONE',  ( 28.84179041037316082, -284.0215787747085869, -305.7508026366863305 ) ) ;
#9638 = CARTESIAN_POINT ( 'NONE',  ( 31.64018965405740502, -277.0912415470053816, -295.5813785493502905 ) ) ;
#9639 = CARTESIAN_POINT ( 'NONE',  ( 202.9738562182569694, 293.9636489450776367, 3.999999999999991562 ) ) ;
#9640 = CARTESIAN_POINT ( 'NONE',  ( 195.1071592636706384, 20.05007635861079152, 15.17306086504857809 ) ) ;
#9641 = CARTESIAN_POINT ( 'NONE',  ( -85.28888665664459268, -271.8020784740338627, -211.1369023491587598 ) ) ;
#9642 = CIRCLE ( 'NONE', #62592, 6.500000000000033751 ) ;
#9643 = CARTESIAN_POINT ( 'NONE',  ( -110.6202909622703459, -280.7667899159553144, -253.6196557692183546 ) ) ;
#9644 = EDGE_CURVE ( 'NONE', #16441, #2619, #86634, .T. ) ;
#9645 = DIRECTION ( 'NONE',  ( 0.000000000000000000, 0.000000000000000000, 1.000000000000000000 ) ) ;
#9646 = CARTESIAN_POINT ( 'NONE',  ( 20.96312752533805934, -288.8142182511105602, -222.3001018252047913 ) ) ;
#9647 = TOROIDAL_SURFACE ( 'NONE', #47489, 4.499999999999993783, 0.5000000000000000000 ) ;
#9648 = FACE_OUTER_BOUND ( 'NONE', #1331, .T. ) ;
#9649 = CARTESIAN_POINT ( 'NONE',  ( -76.62360297572647028, -289.5267465033693952, -206.4115730585729409 ) ) ;
#9650 = DIRECTION ( 'NONE',  ( 0.9764705882352960886, -0.000000000000000000, 0.2156506209390900708 ) ) ;
#9651 = CARTESIAN_POINT ( 'NONE',  ( -108.9827760595227204, -295.1376887373888280, -286.3200260151753582 ) ) ;
#9652 = CARTESIAN_POINT ( 'NONE',  ( 10.90028209779220880, -286.5165004939282767, -326.8522606881854813 ) ) ;
#9653 = CARTESIAN_POINT ( 'NONE',  ( 134.9260051231060800, 178.6636279401649858, -236.0341445084446548 ) ) ;
#9654 = DIRECTION ( 'NONE',  ( -0.9531768234071978929, 0.3024135303179465439, 0.000000000000000000 ) ) ;
#9655 = CARTESIAN_POINT ( 'NONE',  ( 35.28189445654910372, -286.3292427795454955, -293.7816487635085423 ) ) ;
#9656 = CARTESIAN_POINT ( 'NONE',  ( -31.73373715014760066, -281.2221778240656249, -346.1536594611444571 ) ) ;
#9657 = CARTESIAN_POINT ( 'NONE',  ( -109.7001197232018086, -290.6844909527291634, -260.3291148907240427 ) ) ;
#9658 = AXIS2_PLACEMENT_3D ( 'NONE', #77093, #12223, #62916 ) ;
#9659 = VECTOR ( 'NONE', #77029, 1000.000000000000000 ) ;
#9660 = CARTESIAN_POINT ( 'NONE',  ( 22.30006093257002320, -283.5758584552910975, -313.4899532973534519 ) ) ;
#9661 = CARTESIAN_POINT ( 'NONE',  ( 31.51002955751323853, -282.6855108344136056, -295.2504299291638290 ) ) ;
#9662 = CARTESIAN_POINT ( 'NONE',  ( -84.12339619002325719, -291.6710849824654588, -329.5028801870471398 ) ) ;
#9663 = CARTESIAN_POINT ( 'NONE',  ( -104.2132673289376328, -273.3820114902280807, -232.1235974607446053 ) ) ;
#9664 = VECTOR ( 'NONE', #74863, 1000.000000000000000 ) ;
#9665 = CARTESIAN_POINT ( 'NONE',  ( -68.78087493636886052, -287.5420300542889436, -339.0840255363177675 ) ) ;
#9666 = CARTESIAN_POINT ( 'NONE',  ( 9.510340858009232790, -274.6766464873756490, -209.2555842279344347 ) ) ;
#9667 = CARTESIAN_POINT ( 'NONE',  ( -1.675214451139585670, -294.5070912195915298, -204.7741367537638837 ) ) ;
#9668 = CARTESIAN_POINT ( 'NONE',  ( 208.4306832106270804, -125.2391364535880882, 0.000000000000000000 ) ) ;
#9669 = CARTESIAN_POINT ( 'NONE',  ( -85.33152481854864391, -287.9090924074130839, -210.2361428286349110 ) ) ;
#9670 = CARTESIAN_POINT ( 'NONE',  ( -37.15765503423568106, -275.0496619208087736, -345.5403109653299794 ) ) ;
#9671 = CARTESIAN_POINT ( 'NONE',  ( 154.7659666677360235, 19.56018909072649237, -12.94946946942526189 ) ) ;
#9672 = CARTESIAN_POINT ( 'NONE',  ( -84.70309758908993558, -295.8115657042626481, -210.6674127538477137 ) ) ;
#9673 = CARTESIAN_POINT ( 'NONE',  ( -110.7708891840191967, -292.2487011182695369, -262.9723015143296720 ) ) ;
#9674 = CARTESIAN_POINT ( 'NONE',  ( -40.77143143020767013, -273.3565983371993298, -197.2899150103065153 ) ) ;
#9675 = CARTESIAN_POINT ( 'NONE',  ( -106.6784313101480421, -291.7429396202433054, -295.3235990421428028 ) ) ;
#9676 = VECTOR ( 'NONE', #78988, 1000.000000000000000 ) ;
#9677 = CARTESIAN_POINT ( 'NONE',  ( -47.03744230239777124, -292.8672274803445816, -197.7704778735459001 ) ) ;
#9678 = CARTESIAN_POINT ( 'NONE',  ( -95.90467839396086447, -285.6835378491161350, -315.6405171358399571 ) ) ;
#9679 = CARTESIAN_POINT ( 'NONE',  ( -83.92163728383285104, -292.8520801888985261, -209.7228447386410721 ) ) ;
#9680 = CARTESIAN_POINT ( 'NONE',  ( -96.21021476626545166, -292.5287890275836844, -221.4757845979581532 ) ) ;
#9681 = CARTESIAN_POINT ( 'NONE',  ( 35.20667710874763401, -293.4982800520415935, -278.9126461052029526 ) ) ;
#9682 = CARTESIAN_POINT ( 'NONE',  ( 35.01810479133706622, -289.8081786559753255, -290.2786723915117477 ) ) ;
#9683 = CARTESIAN_POINT ( 'NONE',  ( 19.78493743910090430, -282.4205870152138687, -322.0680666349201147 ) ) ;
#9684 = CARTESIAN_POINT ( 'NONE',  ( -29.22743638579740377, -296.2328265389438684, -194.8037401712774113 ) ) ;
#9685 = CARTESIAN_POINT ( 'NONE',  ( -97.57907372424848802, -285.0276190402675525, -222.3980193881760101 ) ) ;
#9686 = CARTESIAN_POINT ( 'NONE',  ( 30.57229365799015497, -277.1221266620555070, -239.2597902487837018 ) ) ;
#9687 = CARTESIAN_POINT ( 'NONE',  ( -110.4927588826779896, -283.2682903735683908, -276.3655419500586845 ) ) ;
#9688 = CARTESIAN_POINT ( 'NONE',  ( 18.80684608830102533, -284.8598328251433713, -220.5617770117214036 ) ) ;
#9689 = CARTESIAN_POINT ( 'NONE',  ( -112.8502645824861332, -276.6048669289613713, -277.1956951455856597 ) ) ;
#9690 = DIRECTION ( 'NONE',  ( 0.000000000000000000, 0.000000000000000000, 1.000000000000000000 ) ) ;
#9691 = CARTESIAN_POINT ( 'NONE',  ( -13.51521690613310867, -282.2420721763609777, -339.4820312254543069 ) ) ;
#9692 = CARTESIAN_POINT ( 'NONE',  ( -90.79215903166142709, -280.5197032940744180, -215.4140538910143050 ) ) ;
#9693 = CARTESIAN_POINT ( 'NONE',  ( 25.65173673949179545, -287.1934814764543944, -314.3231674453072060 ) ) ;
#9694 = CARTESIAN_POINT ( 'NONE',  ( 10.96967698473418196, -296.1328630804842419, -326.4323659849628712 ) ) ;
#9695 = CARTESIAN_POINT ( 'NONE',  ( -1.822379850096921050, -278.1896645024045256, -337.7763855712681789 ) ) ;
#9696 = CARTESIAN_POINT ( 'NONE',  ( -82.24323739268915290, -278.9659198923695271, -332.3058532132864116 ) ) ;
#9697 = CARTESIAN_POINT ( 'NONE',  ( -66.80460821013873840, -277.2826198268955977, -337.1513646647946416 ) ) ;
#9698 = CARTESIAN_POINT ( 'NONE',  ( 54.45717190063074042, -301.2040501375654458, -195.4963978399819666 ) ) ;
#9699 = CARTESIAN_POINT ( 'NONE',  ( 1.132567318379380295, -284.5664680352114715, -206.1153447585900551 ) ) ;
#9700 = CARTESIAN_POINT ( 'NONE',  ( -113.5690871964362998, -292.1771159278787877, -268.3958913118173655 ) ) ;
#9701 = CARTESIAN_POINT ( 'NONE',  ( -23.47377997482075074, -293.7911545718362163, -342.3984021109696414 ) ) ;
#9702 = VERTEX_POINT ( 'NONE', #18183 ) ;
#9703 = CARTESIAN_POINT ( 'NONE',  ( -44.29799553449681326, -291.6286053763753330, -197.6212392608824473 ) ) ;
#9704 = ORIENTED_EDGE ( 'NONE', *, *, #61720, .F. ) ;
#9705 = CARTESIAN_POINT ( 'NONE',  ( -40.31296186643939450, -290.1683176475759751, -347.0074567454298062 ) ) ;
#9706 = CARTESIAN_POINT ( 'NONE',  ( -62.35160674059837049, -280.3695924750994095, -201.6170928565556437 ) ) ;
#9707 = CARTESIAN_POINT ( 'NONE',  ( -100.4883037576032052, -296.0496371898498182, -226.8179472181121525 ) ) ;
#9708 = CARTESIAN_POINT ( 'NONE',  ( 39.53796266087696409, -288.1824963986957187, -268.6787875364595379 ) ) ;
#9709 = CARTESIAN_POINT ( 'NONE',  ( 18.63235654641265526, -288.6072984260324006, -323.2066406965383294 ) ) ;
#9710 = CARTESIAN_POINT ( 'NONE',  ( -82.80457111999362496, -284.0266621948856027, -327.5680566504572653 ) ) ;
#9711 = CARTESIAN_POINT ( 'NONE',  ( -110.4262895430625235, -266.6388475384601406, -306.9518243255819812 ) ) ;
#9712 = AXIS2_PLACEMENT_3D ( 'NONE', #80216, #9154, #87304 ) ;
#9713 = CARTESIAN_POINT ( 'NONE',  ( -72.24340455811125139, -195.2487258463710589, -358.8499853455330708 ) ) ;
#9714 = CARTESIAN_POINT ( 'NONE',  ( -102.6165336565486541, -253.8500844666206717, -324.0719648433210409 ) ) ;
#9715 = CARTESIAN_POINT ( 'NONE',  ( -97.02333222867909512, -277.1594937821095073, -312.6995964369357353 ) ) ;
#9716 = CARTESIAN_POINT ( 'NONE',  ( -45.95801919408835801, -276.0841584091795085, -343.2129552043403464 ) ) ;
#9717 = CARTESIAN_POINT ( 'NONE',  ( -35.82335762372186139, -297.5783404797697926, -193.4227788670093275 ) ) ;
#9718 = CARTESIAN_POINT ( 'NONE',  ( 122.9258408653956991, 147.2208392559248296, -261.0359777952371019 ) ) ;
#9719 = CARTESIAN_POINT ( 'NONE',  ( -59.53803955172939766, -276.0185769589936058, -343.5773783888014918 ) ) ;
#9720 = AXIS2_PLACEMENT_3D ( 'NONE', #11752, #47248, #40605 ) ;
#9721 = EDGE_LOOP ( 'NONE', ( #25196, #9470, #34189, #26568 ) ) ;
#9722 = CARTESIAN_POINT ( 'NONE',  ( -109.2383596609985972, -290.8732257106869383, -283.3556856857578623 ) ) ;
#9723 = CARTESIAN_POINT ( 'NONE',  ( -30.51270251543930456, -298.9384395258788913, -193.5216892424431876 ) ) ;
#9724 = CARTESIAN_POINT ( 'NONE',  ( 35.24365826826731762, -286.3889136012417680, -281.9568113050851821 ) ) ;
#9725 = CARTESIAN_POINT ( 'NONE',  ( -23.37999692633991700, -298.7149106595792887, -193.4215241743794991 ) ) ;
#9726 = CARTESIAN_POINT ( 'NONE',  ( -88.50033490900717936, -295.9604296249843856, -322.5070443184440592 ) ) ;
#9727 = ORIENTED_EDGE ( 'NONE', *, *, #47895, .F. ) ;
#9728 = CARTESIAN_POINT ( 'NONE',  ( 199.0029451100810434, 66.39899626990381876, -8.059931973035714847 ) ) ;
#9729 = CIRCLE ( 'NONE', #42998, 5.654241149514405151 ) ;
#9730 = CIRCLE ( 'NONE', #62695, 0.5000000000000003331 ) ;
#9731 = CARTESIAN_POINT ( 'NONE',  ( -51.02735006416685337, -279.1458987424568363, -344.6713943997652336 ) ) ;
#9732 = CARTESIAN_POINT ( 'NONE',  ( 36.41788400524419700, -281.3367010969636794, -292.4315722113687457 ) ) ;
#9733 = CIRCLE ( 'NONE', #46017, 24.50000000000001066 ) ;
#9734 = CARTESIAN_POINT ( 'NONE',  ( -106.5514983162812968, -279.3098327798778655, -294.6858358276443823 ) ) ;
#9735 = CARTESIAN_POINT ( 'NONE',  ( -107.5845723957051376, -280.6855329966974182, -241.3798670223202123 ) ) ;
#9736 = CARTESIAN_POINT ( 'NONE',  ( -33.75803411021154687, -296.6726007387902655, -196.7727745394008139 ) ) ;
#9737 = CARTESIAN_POINT ( 'NONE',  ( 197.9812641850257080, 65.99374301882849636, -9.931412343739248527 ) ) ;
#9738 = CARTESIAN_POINT ( 'NONE',  ( 19.67468459943277992, -281.0747940208947284, -224.7745862308991889 ) ) ;
#9739 = CARTESIAN_POINT ( 'NONE',  ( -3.905633187153184416, -275.2848279538511633, -201.1643582922885116 ) ) ;
#9740 = AXIS2_PLACEMENT_3D ( 'NONE', #55474, #70624, #54991 ) ;
#9741 = CARTESIAN_POINT ( 'NONE',  ( -13.71725678742743781, -276.3589537357258337, -199.1790533596775958 ) ) ;
#9742 = CARTESIAN_POINT ( 'NONE',  ( 32.47398523807097348, -274.5263043586089111, -301.4155277852229347 ) ) ;
#9743 = ORIENTED_EDGE ( 'NONE', *, *, #57401, .T. ) ;
#9744 = DIRECTION ( 'NONE',  ( -1.000000000000000000, 0.000000000000000000, 0.000000000000000000 ) ) ;
#9745 = CARTESIAN_POINT ( 'NONE',  ( -83.92400360699230077, -290.5900684568355246, -213.9457767266160602 ) ) ;
#9746 = CARTESIAN_POINT ( 'NONE',  ( -113.3853541599517030, -284.0482895119258728, -258.5789019710456387 ) ) ;
#9747 = EDGE_CURVE ( 'NONE', #15079, #15987, #41264, .T. ) ;
#9748 = CARTESIAN_POINT ( 'NONE',  ( 34.44383347964154041, -279.5568131191429870, -252.2870437996168107 ) ) ;
#9750 = CARTESIAN_POINT ( 'NONE',  ( -69.37283355358874815, -283.7072063281451051, -203.1509231710868733 ) ) ;
#9749 = CARTESIAN_POINT ( 'NONE',  ( 5.279068719812944011, -279.2163240380427851, -210.3707439335192078 ) ) ;
#9751 = CARTESIAN_POINT ( 'NONE',  ( 31.77609534240992417, -289.9341811840557739, -299.6089987112021049 ) ) ;
#9752 = CARTESIAN_POINT ( 'NONE',  ( 7.372140313387451016, -281.8820973033118662, -212.0919861584098669 ) ) ;
#9753 = DIRECTION ( 'NONE',  ( 0.000000000000000000, 0.000000000000000000, 1.000000000000000000 ) ) ;
#9754 = CARTESIAN_POINT ( 'NONE',  ( -71.39965445627603913, -281.8942926984311157, -338.5263302623653203 ) ) ;
#9755 = CARTESIAN_POINT ( 'NONE',  ( -6.593732790961580825, -296.6485725985107820, -338.7684506057563567 ) ) ;
#9756 = CARTESIAN_POINT ( 'NONE',  ( -53.52254542783733626, -278.0873266681529685, -196.0633866177273035 ) ) ;
#9757 = CARTESIAN_POINT ( 'NONE',  ( -111.7800635601057451, -286.4138848816814971, -281.1661910985126269 ) ) ;
#9758 = LINE ( 'NONE', #89272, #23223 ) ;
#9759 = CARTESIAN_POINT ( 'NONE',  ( 3.345148980613364742, -294.5141475197300451, -206.6289105848380814 ) ) ;
#9760 = CARTESIAN_POINT ( 'NONE',  ( -29.52975948234265502, -274.9531837361189446, -345.0054695198509194 ) ) ;
#9761 = CARTESIAN_POINT ( 'NONE',  ( -65.39761142603670407, -288.6067599024544279, -341.9507278319026113 ) ) ;
#9762 = CARTESIAN_POINT ( 'NONE',  ( 31.58273731087751912, -291.6035428158867262, -243.9819152356743643 ) ) ;
#9763 = CARTESIAN_POINT ( 'NONE',  ( -43.43092116352006826, -259.9338699230254406, -439.2716167192226067 ) ) ;
#9764 = CARTESIAN_POINT ( 'NONE',  ( 33.71473966042284331, -274.4831356230225197, -289.1287988120994328 ) ) ;
#9765 = CARTESIAN_POINT ( 'NONE',  ( -105.0731592380539610, -294.2877703324295453, -300.8729624262172138 ) ) ;
#9766 = CARTESIAN_POINT ( 'NONE',  ( -56.17592060565986856, -290.6149353201861913, -341.4528586170248445 ) ) ;
#9767 = FACE_OUTER_BOUND ( 'NONE', #36839, .T. ) ;
#9768 = CARTESIAN_POINT ( 'NONE',  ( 27.47376236305100861, -291.4993518334920850, -229.9913528745648250 ) ) ;
#9769 = CARTESIAN_POINT ( 'NONE',  ( -16.97039141062375123, -287.9196120952910292, -199.3749794889406814 ) ) ;
#9770 = CARTESIAN_POINT ( 'NONE',  ( -88.82164420867685806, -288.0033196463141394, -326.2519881607545926 ) ) ;
#9771 = EDGE_CURVE ( 'NONE', #80899, #38465, #26144, .T. ) ;
#9772 = CARTESIAN_POINT ( 'NONE',  ( 22.45988901229327439, -288.3817652812061851, -227.3899815451443942 ) ) ;
#9773 = CARTESIAN_POINT ( 'NONE',  ( -39.80257052418233599, -229.5268262511776527, 22.50000000000000000 ) ) ;
#9774 = CARTESIAN_POINT ( 'NONE',  ( 19.63451674066463681, -287.7073056923214835, -224.4466923867013861 ) ) ;
#9775 = CARTESIAN_POINT ( 'NONE',  ( 3.360558448169713941, -296.4883044739045772, -333.8396993327915538 ) ) ;
#9776 = CARTESIAN_POINT ( 'NONE',  ( 7.300011400535150408, -287.8504146969630142, -208.0452830692688053 ) ) ;
#9777 = CARTESIAN_POINT ( 'NONE',  ( -99.29902237962620859, -276.0494080346783221, -313.6116025848223785 ) ) ;
#9778 = CARTESIAN_POINT ( 'NONE',  ( -113.7447166088730768, -278.7625871955591492, -280.1810138114370261 ) ) ;
#9779 = CARTESIAN_POINT ( 'NONE',  ( 10.81308941622893727, -280.3637467699149397, -210.2356486785652976 ) ) ;
#9780 = CARTESIAN_POINT ( 'NONE',  ( -53.00427921903821726, -299.8304358388951982, -197.3249770768330507 ) ) ;
#9781 = CARTESIAN_POINT ( 'NONE',  ( -40.02052801174312435, -284.0183229268633340, -195.4089696973081232 ) ) ;
#9782 = DIRECTION ( 'NONE',  ( -0.000000000000000000, -0.000000000000000000, 1.000000000000000000 ) ) ;
#9783 = CARTESIAN_POINT ( 'NONE',  ( -79.74127196714272259, -277.6117016336031043, -209.4255636160433482 ) ) ;
#9784 = CARTESIAN_POINT ( 'NONE',  ( -60.63534809389868485, -281.3540195771609547, -341.7063627447745944 ) ) ;
#9785 = DIRECTION ( 'NONE',  ( 0.000000000000000000, 0.000000000000000000, 1.000000000000000000 ) ) ;
#9786 = CARTESIAN_POINT ( 'NONE',  ( -34.33794152799971044, -275.4949121717301068, -346.6086437673907312 ) ) ;
#9787 = CARTESIAN_POINT ( 'NONE',  ( -96.14599511751498540, -297.4539419530267423, -314.7976917115472588 ) ) ;
#9788 = CARTESIAN_POINT ( 'NONE',  ( 23.15058279763064419, -281.1050318346463541, -317.5222990162498036 ) ) ;
#9789 = CARTESIAN_POINT ( 'NONE',  ( -109.2790518340333108, -297.6747840242583152, -256.5674410555818667 ) ) ;
#9790 = CARTESIAN_POINT ( 'NONE',  ( -111.8218348645858811, -297.6464213469399738, -287.9108098609399917 ) ) ;
#9791 = CARTESIAN_POINT ( 'NONE',  ( 22.30055460734150330, -274.6307383756973763, -228.2100405927494933 ) ) ;
#9792 = CARTESIAN_POINT ( 'NONE',  ( -11.59696698761547573, -294.3874482099959096, -199.8628208135307318 ) ) ;
#9793 = CARTESIAN_POINT ( 'NONE',  ( 14.24530587071075161, -286.9197968553933720, -213.1250789842667075 ) ) ;
#9794 = CARTESIAN_POINT ( 'NONE',  ( -39.52076249630715665, -278.1048740695651986, -194.8197344119153342 ) ) ;
#9795 = CIRCLE ( 'NONE', #29490, 4.999999999999990230 ) ;
#9796 = CARTESIAN_POINT ( 'NONE',  ( -112.9245502226013969, -290.5702363738715235, -255.5875854675222456 ) ) ;
#9797 = CARTESIAN_POINT ( 'NONE',  ( -105.3359527187882207, -289.2463177848592295, -297.7037137619369105 ) ) ;
#9798 = CARTESIAN_POINT ( 'NONE',  ( 18.89634741421465947, -290.8620007685027531, -220.7203140196610605 ) ) ;
#9799 = VERTEX_POINT ( 'NONE', #55108 ) ;
#9800 = CARTESIAN_POINT ( 'NONE',  ( 185.2614386149834900, 255.8498544563436212, -168.8850006258623466 ) ) ;
#9801 = CARTESIAN_POINT ( 'NONE',  ( -34.58195314628625994, -288.5243327706897389, -343.4201401007718459 ) ) ;
#9802 = DIRECTION ( 'NONE',  ( -1.000000000000000000, 0.000000000000000000, 0.000000000000000000 ) ) ;
#9803 = CARTESIAN_POINT ( 'NONE',  ( -112.2927515526778564, -285.2853080173690046, -286.9490685634335705 ) ) ;
#9804 = CARTESIAN_POINT ( 'NONE',  ( 23.79513032152149776, -291.9901604993756337, -223.9163402126301037 ) ) ;
#9805 = CARTESIAN_POINT ( 'NONE',  ( 26.32087894317058385, -283.4294005228077253, -312.7919357759415107 ) ) ;
#9806 = CARTESIAN_POINT ( 'NONE',  ( -104.1141557471359818, -283.9884278403224016, -299.8643241657096041 ) ) ;
#9807 = CARTESIAN_POINT ( 'NONE',  ( -97.34634728117254099, -297.1988415976783244, -222.1071821841918847 ) ) ;
#9808 = CARTESIAN_POINT ( 'NONE',  ( 17.81636526077367932, -277.5563473228442604, -318.9479098553642871 ) ) ;
#9809 = CARTESIAN_POINT ( 'NONE',  ( -63.35073507984012764, -289.7316987517211260, -200.3941478945161521 ) ) ;
#9810 = AXIS2_PLACEMENT_3D ( 'NONE', #43476, #35459, #57245 ) ;
#9811 = CARTESIAN_POINT ( 'NONE',  ( -48.92304016706964376, -272.6963947151297702, -197.8320633928682355 ) ) ;
#9812 = VERTEX_POINT ( 'NONE', #84430 ) ;
#9813 = CARTESIAN_POINT ( 'NONE',  ( 196.1089143772224759, 40.84001755061112959, 13.20492811982817294 ) ) ;
#9814 = CARTESIAN_POINT ( 'NONE',  ( -84.58018157659009262, -287.3162523268560449, -212.7629163056879236 ) ) ;
#9815 = CARTESIAN_POINT ( 'NONE',  ( -94.41231436011754852, -296.9337271715625093, -321.6099434708485205 ) ) ;
#9816 = CARTESIAN_POINT ( 'NONE',  ( -110.4923597237573745, -285.1962291497000592, -270.9183435146323973 ) ) ;
#9817 = CARTESIAN_POINT ( 'NONE',  ( 8.092125093130805524, -275.5069109236012537, -332.3025060009279628 ) ) ;
#9818 = CARTESIAN_POINT ( 'NONE',  ( 8.783148742161767331, -293.3170895263070861, -208.7657199287959031 ) ) ;
#9819 = CARTESIAN_POINT ( 'NONE',  ( 25.34885385511638844, -285.1214030380116355, -227.7914877013124055 ) ) ;
#9820 = CARTESIAN_POINT ( 'NONE',  ( 39.41966412220719462, -293.8130945796434617, -264.5786228559652500 ) ) ;
#9821 = CARTESIAN_POINT ( 'NONE',  ( -108.7321347707435137, -291.0878121699835219, -255.0153261033129581 ) ) ;
#9822 = CARTESIAN_POINT ( 'NONE',  ( 209.3190042249899250, 30.23012903947020646, 14.26380412667039010 ) ) ;
#9823 = CARTESIAN_POINT ( 'NONE',  ( 221.8344101925596306, -43.55766379199612004, 22.50000000000000000 ) ) ;
#9824 = CARTESIAN_POINT ( 'NONE',  ( 6.292094988509354891, -59.58581467011203614, -351.0172641016240505 ) ) ;
#9825 = CARTESIAN_POINT ( 'NONE',  ( -113.6342575831652368, -286.1126340743217042, -267.1629504333221803 ) ) ;
#9826 = CARTESIAN_POINT ( 'NONE',  ( -2.659677404128736544, -274.1237833571632905, -342.4524372437778652 ) ) ;
#9827 = ORIENTED_EDGE ( 'NONE', *, *, #69553, .F. ) ;
#9828 = CARTESIAN_POINT ( 'NONE',  ( -109.0252103026800938, -283.2700229538513099, -285.7733293863130939 ) ) ;
#9829 = CARTESIAN_POINT ( 'NONE',  ( -112.1556390077946332, -277.9914063238471158, -288.5441879536006127 ) ) ;
#9830 = CARTESIAN_POINT ( 'NONE',  ( 36.12945993587742777, -283.3685413907255679, -256.0804567259272062 ) ) ;
#9831 = CARTESIAN_POINT ( 'NONE',  ( -97.34057529231125727, -248.7244481610983087, -333.3648534768652780 ) ) ;
#9832 = CARTESIAN_POINT ( 'NONE',  ( -83.54149235775581417, -282.2461979953035893, -331.2896159282820463 ) ) ;
#9833 = CARTESIAN_POINT ( 'NONE',  ( 34.98849370620082055, -285.3335742626629212, -251.8652202634366688 ) ) ;
#9834 = CARTESIAN_POINT ( 'NONE',  ( 25.11272978387250276, -276.8369696826169388, -227.4458297074222060 ) ) ;
#9835 = CARTESIAN_POINT ( 'NONE',  ( -20.82817513350164162, -295.3269101086378328, -341.5841320997348021 ) ) ;
#9836 = CARTESIAN_POINT ( 'NONE',  ( 4.800036883009760835, -291.3191363122518283, -210.0881147899867187 ) ) ;
#9837 = CARTESIAN_POINT ( 'NONE',  ( -96.06597149290826110, -278.5335842364756900, -320.0279166731389751 ) ) ;
#9838 = CARTESIAN_POINT ( 'NONE',  ( -27.02151370780244122, -276.9172729085353239, -342.6279412990078868 ) ) ;
#9839 = CARTESIAN_POINT ( 'NONE',  ( 19.63828796805541188, -275.1722565129433633, -321.7108111205922114 ) ) ;
#9840 = DIRECTION ( 'NONE',  ( 0.9167375550253826777, 5.544037366339495023E-15, 0.3994899938747948354 ) ) ;
#9841 = CARTESIAN_POINT ( 'NONE',  ( -37.81293164330911338, -275.0579264444754131, -345.3722021308782359 ) ) ;
#9842 = EDGE_CURVE ( 'NONE', #4469, #69769, #12576, .T. ) ;
#9843 = CARTESIAN_POINT ( 'NONE',  ( 3.924473101418306520, -295.9337739410519248, -334.7329023063056184 ) ) ;
#9844 = CARTESIAN_POINT ( 'NONE',  ( 180.5235960634565799, 214.6007075219689000, -24.43326837773227211 ) ) ;
#9845 = DIRECTION ( 'NONE',  ( 1.000000000000000000, 0.000000000000000000, 1.224646799147353207E-16 ) ) ;
#9846 = CARTESIAN_POINT ( 'NONE',  ( -89.10284742764287103, -284.8805173293629309, -322.3458382200366827 ) ) ;
#9847 = CARTESIAN_POINT ( 'NONE',  ( -33.09270350509498826, -284.7594926595880338, -346.2418599714705465 ) ) ;
#9848 = CARTESIAN_POINT ( 'NONE',  ( -10.70511129342985690, -285.7575212949250840, -202.2712564899942151 ) ) ;
#9849 = CARTESIAN_POINT ( 'NONE',  ( 28.73783559161208245, -274.3941693347215391, -303.3386281445947361 ) ) ;
#9850 = CARTESIAN_POINT ( 'NONE',  ( 35.44641809470454774, -283.6026141821849365, -285.0113242216903018 ) ) ;
#9851 = CARTESIAN_POINT ( 'NONE',  ( -109.9726944037626311, -276.8681261896258547, -282.9036337822892619 ) ) ;
#9852 = CARTESIAN_POINT ( 'NONE',  ( -21.57318746054862402, -277.9250244664475531, -342.0064894934947688 ) ) ;
#9853 = DIRECTION ( 'NONE',  ( 0.000000000000000000, -1.000000000000000000, 0.000000000000000000 ) ) ;
#9854 = CARTESIAN_POINT ( 'NONE',  ( 35.17189338322290126, -282.0319481775883332, -244.7869617890567895 ) ) ;
#9855 = CARTESIAN_POINT ( 'NONE',  ( -38.17553398408971077, -280.5343091141434684, -193.4271747283714262 ) ) ;
#9856 = ORIENTED_EDGE ( 'NONE', *, *, #89600, .T. ) ;
#9857 = ORIENTED_EDGE ( 'NONE', *, *, #56217, .T. ) ;
#9858 = CARTESIAN_POINT ( 'NONE',  ( 195.3470921470671158, 40.91257177144665746, 14.84270801981803700 ) ) ;
#9859 = CARTESIAN_POINT ( 'NONE',  ( 36.80964199851275964, -289.2140874069019105, -254.7457740286168644 ) ) ;
#9860 = CARTESIAN_POINT ( 'NONE',  ( -77.59230153146845055, -296.6941246685178157, -209.2061314547664495 ) ) ;
#9861 = CARTESIAN_POINT ( 'NONE',  ( -84.19766316037826925, -290.7757288606391626, -209.3199886476936342 ) ) ;
#9862 = EDGE_CURVE ( 'NONE', #33982, #56036, #65525, .T. ) ;
#9863 = CARTESIAN_POINT ( 'NONE',  ( 34.37136329923080069, -286.2537841291144787, -287.3300392358489717 ) ) ;
#9864 = CARTESIAN_POINT ( 'NONE',  ( -26.40510210283736114, -287.4851145156978873, -343.1845903235468427 ) ) ;
#9865 = CARTESIAN_POINT ( 'NONE',  ( -9.356116832418225115, -287.6313537156144093, -202.4952158166496190 ) ) ;
#9866 = CARTESIAN_POINT ( 'NONE',  ( -95.51957283810780552, -275.8997473858997864, -317.7134222536338370 ) ) ;
#9867 = CARTESIAN_POINT ( 'NONE',  ( 35.61350560996478976, -286.2315701808482231, -292.4059039905488362 ) ) ;
#9868 = CARTESIAN_POINT ( 'NONE',  ( 36.06071206279163732, -289.3538093307945473, -254.9014189386541318 ) ) ;
#9869 = CARTESIAN_POINT ( 'NONE',  ( -54.11782974035947547, -287.2667779930648067, -343.6851928737355593 ) ) ;
#9870 = CARTESIAN_POINT ( 'NONE',  ( 25.76786062151803591, -283.0033063016231836, -307.6176703856384620 ) ) ;
#9871 = CARTESIAN_POINT ( 'NONE',  ( -111.0647581494525440, -292.3636499960987862, -285.0870527662316363 ) ) ;
#9872 = CARTESIAN_POINT ( 'NONE',  ( 185.0172044724083946, 276.0000000000000568, 22.46007009812148425 ) ) ;
#9873 = CARTESIAN_POINT ( 'NONE',  ( 152.4536156746142410, 249.5000000000000568, 12.50000000000000000 ) ) ;
#9874 = CARTESIAN_POINT ( 'NONE',  ( -94.49818481850003593, -299.1532571841493109, -220.8618432982795525 ) ) ;
#9875 = CARTESIAN_POINT ( 'NONE',  ( -32.94311282739938207, -279.3061489930066159, -197.3319857342073078 ) ) ;
#9876 = CARTESIAN_POINT ( 'NONE',  ( 34.12965940181446456, -279.8473453391552539, -293.2643087542202807 ) ) ;
#9877 = CARTESIAN_POINT ( 'NONE',  ( 36.93784224080613399, -292.9960305013196376, -290.0260208911292921 ) ) ;
#9878 = CARTESIAN_POINT ( 'NONE',  ( -83.80962717219931335, -271.6437861450824016, -212.7529087836911117 ) ) ;
#9879 = CARTESIAN_POINT ( 'NONE',  ( -10.76227492213332226, -274.7826462363113933, -339.8941917943659519 ) ) ;
#9880 = CARTESIAN_POINT ( 'NONE',  ( -99.13895738467218166, -297.3193845195517042, -310.2329832237285814 ) ) ;
#9881 = CARTESIAN_POINT ( 'NONE',  ( 206.1702329640447147, -6.606856988583545110E-17, 7.166221634559009956 ) ) ;
#9882 = CARTESIAN_POINT ( 'NONE',  ( 18.77375479150365933, -297.2225164868111165, -194.0686380784358391 ) ) ;
#9883 = CARTESIAN_POINT ( 'NONE',  ( -74.13560225244695800, -293.7736376000908081, -336.9045079275734338 ) ) ;
#9884 = EDGE_CURVE ( 'NONE', #43035, #26246, #4435, .T. ) ;
#9885 = CARTESIAN_POINT ( 'NONE',  ( 23.06128707832070646, -294.3959680663696759, -228.3049597045583141 ) ) ;
#9886 = CARTESIAN_POINT ( 'NONE',  ( -83.63170945779074827, -373.0521521680024648, -517.1711561948568487 ) ) ;
#9887 = CARTESIAN_POINT ( 'NONE',  ( 26.37015791516194341, -293.8625538294185162, -234.2938191352998274 ) ) ;
#9888 = LINE ( 'NONE', #74285, #68682 ) ;
#9890 = CARTESIAN_POINT ( 'NONE',  ( -47.79303666712760901, -295.1886229446446350, -342.6603706623741346 ) ) ;
#9889 = CARTESIAN_POINT ( 'NONE',  ( -33.77931186183484868, -284.1168854587702981, -195.0901661182930695 ) ) ;
#9891 = CARTESIAN_POINT ( 'NONE',  ( -50.09350821601505999, -283.2104416505460449, -346.3517522504720318 ) ) ;
#9892 = CARTESIAN_POINT ( 'NONE',  ( 22.58992810886332947, -282.8465046359950179, -224.3235344374665203 ) ) ;
#9893 = CARTESIAN_POINT ( 'NONE',  ( -109.0072414961743306, -284.5768410370488368, -242.1128923590738395 ) ) ;
#9894 = CARTESIAN_POINT ( 'NONE',  ( -112.1705501103153182, -288.5414404816520459, -271.1806506031392701 ) ) ;
#9895 = DIRECTION ( 'NONE',  ( 0.000000000000000000, 1.000000000000000000, 0.000000000000000000 ) ) ;
#9896 = CARTESIAN_POINT ( 'NONE',  ( 25.34956039056106647, -280.6122332085997755, -313.8871202295876515 ) ) ;
#9897 = CARTESIAN_POINT ( 'NONE',  ( -10.55472642596464183, -285.0938676076682441, -201.9099254332658404 ) ) ;
#9898 = CARTESIAN_POINT ( 'NONE',  ( -4.478041913113405492, -287.5495392352121371, -339.6681960487437664 ) ) ;
#9899 = DIRECTION ( 'NONE',  ( -1.000000000000000000, -4.095251346825557639E-15, 0.000000000000000000 ) ) ;
#9900 = CARTESIAN_POINT ( 'NONE',  ( -12.72236635771002788, -296.3269730412072249, -339.9874377601415176 ) ) ;
#9901 = CARTESIAN_POINT ( 'NONE',  ( -86.70062840136722571, -279.1477484668685634, -328.7595926825929382 ) ) ;
#9903 = CARTESIAN_POINT ( 'NONE',  ( -68.52847119376930607, -279.2973688576392419, -204.3348141531652686 ) ) ;
#9902 = CARTESIAN_POINT ( 'NONE',  ( -14.30927091733863676, -292.7750434281453522, -342.1100831703632821 ) ) ;
#9904 = CARTESIAN_POINT ( 'NONE',  ( -2.057729579103245499, -292.6729075361406558, -201.9062833302965601 ) ) ;
#9905 = CARTESIAN_POINT ( 'NONE',  ( -109.5426468588345159, -282.9191558380418314, -247.9065675782656228 ) ) ;
#9906 = EDGE_CURVE ( 'NONE', #33474, #46837, #71534, .T. ) ;
#9907 = CARTESIAN_POINT ( 'NONE',  ( -48.17914321879006678, -279.1900778574910191, -344.6264829827023277 ) ) ;
#9908 = CARTESIAN_POINT ( 'NONE',  ( -3.044139853223456260, -293.6459454442413630, -335.0688131032514434 ) ) ;
#9909 = CARTESIAN_POINT ( 'NONE',  ( -67.35312805639196654, -295.6585651308055276, -201.5721544375535927 ) ) ;
#9910 = VERTEX_POINT ( 'NONE', #68851 ) ;
#9911 = DIRECTION ( 'NONE',  ( -0.7957555401921962979, -0.6056179655966504871, 0.000000000000000000 ) ) ;
#9912 = CARTESIAN_POINT ( 'NONE',  ( -11.18999682103091686, -282.3743959738797571, -200.3926948210630599 ) ) ;
#9913 = CARTESIAN_POINT ( 'NONE',  ( -110.1611162163360973, -295.9736302621539039, -276.8989164124456579 ) ) ;
#9914 = DIRECTION ( 'NONE',  ( 1.000000000000000000, 0.000000000000000000, 0.000000000000000000 ) ) ;
#9915 = CARTESIAN_POINT ( 'NONE',  ( -69.85430415644619018, -271.1237833571632905, -202.7746430608542312 ) ) ;
#9916 = CARTESIAN_POINT ( 'NONE',  ( -111.6594595240124619, -271.9965132982247269, -250.6376077469666370 ) ) ;
#9917 = CARTESIAN_POINT ( 'NONE',  ( 36.89423065911203281, -288.6343510633527103, -251.8590949951244227 ) ) ;
#9918 = CARTESIAN_POINT ( 'NONE',  ( -74.71772516099515826, -289.3979432552050639, -333.0817278144757552 ) ) ;
#9919 = CARTESIAN_POINT ( 'NONE',  ( -5.274120841319772879, -282.0021661177767669, -204.0106988921551761 ) ) ;
#9920 = CARTESIAN_POINT ( 'NONE',  ( -63.45772478805206163, -299.4673947567290497, -201.0542547850966173 ) ) ;
#9921 = CARTESIAN_POINT ( 'NONE',  ( -79.26919076345298265, -278.2669363119382524, -210.1181430150086555 ) ) ;
#9922 = ORIENTED_EDGE ( 'NONE', *, *, #31774, .F. ) ;
#9923 = CARTESIAN_POINT ( 'NONE',  ( -104.2284779812430600, -272.8821307731292336, -232.1075735540319727 ) ) ;
#9924 = CARTESIAN_POINT ( 'NONE',  ( -100.9546090670384615, -292.9944419588503024, -231.6996124152321670 ) ) ;
#9925 = CARTESIAN_POINT ( 'NONE',  ( 223.4306832106270804, -147.4436952405746979, 21.50000000000000000 ) ) ;
#9926 = CARTESIAN_POINT ( 'NONE',  ( -82.60289083594690851, -290.3410952500420876, -327.7659721634676657 ) ) ;
#9927 = DIRECTION ( 'NONE',  ( 0.000000000000000000, 0.000000000000000000, 1.000000000000000000 ) ) ;
#9928 = CARTESIAN_POINT ( 'NONE',  ( 35.11279740381718995, -291.4090784477664329, -248.2104685958580035 ) ) ;
#9929 = CARTESIAN_POINT ( 'NONE',  ( -69.26294878366692842, -297.2868899521721460, -204.6867594310858749 ) ) ;
#9930 = DIRECTION ( 'NONE',  ( -1.000000000000000000, -0.000000000000000000, 0.000000000000000000 ) ) ;
#9931 = CARTESIAN_POINT ( 'NONE',  ( -111.8838571220086493, -291.8663737897115880, -286.6759758174366652 ) ) ;
#9932 = CARTESIAN_POINT ( 'NONE',  ( 25.18497378105907814, -289.4090924074130839, -220.4570493818173702 ) ) ;
#9933 = CARTESIAN_POINT ( 'NONE',  ( 36.33096146400724535, -289.7212613059061823, -283.4899931212314073 ) ) ;
#9934 = CARTESIAN_POINT ( 'NONE',  ( 26.93764601780200252, -274.0659118134340133, -308.6781387921165560 ) ) ;
#9935 = CARTESIAN_POINT ( 'NONE',  ( 35.52600146347161569, -277.2746245475428850, -255.0801729698249858 ) ) ;
#9936 = CARTESIAN_POINT ( 'NONE',  ( 27.50068826931539689, -291.1400055566363676, -233.6938217431761302 ) ) ;
#9937 = CARTESIAN_POINT ( 'NONE',  ( -90.21344657196837602, -281.1749379213878797, -216.0211708448780143 ) ) ;
#9938 = PRESENTATION_LAYER_ASSIGNMENT (  '', '', ( #31117 ) ) ;
#9939 = ORIENTED_EDGE ( 'NONE', *, *, #13746, .F. ) ;
#9940 = CARTESIAN_POINT ( 'NONE',  ( -40.24670249014474166, -282.4382147928780569, -343.4053075509805240 ) ) ;
#9941 = CARTESIAN_POINT ( 'NONE',  ( -95.90421196187325847, -278.9617731786528907, -319.8982959258485153 ) ) ;
#9942 = CARTESIAN_POINT ( 'NONE',  ( -4.348827258955087594, -281.4218677185662614, -339.5093072718176472 ) ) ;
#9943 = CARTESIAN_POINT ( 'NONE',  ( -89.04476833809601999, -278.6995507975592545, -327.1027512870687133 ) ) ;
#9944 = EDGE_CURVE ( 'NONE', #37492, #55107, #24662, .T. ) ;
#9945 = APPLICATION_PROTOCOL_DEFINITION ( 'draft international standard', 'automotive_design', 1998, #80138 ) ;
#9946 = CARTESIAN_POINT ( 'NONE',  ( -55.19039093520709827, -275.3467254329793263, -196.1712804887263815 ) ) ;
#9947 = CARTESIAN_POINT ( 'NONE',  ( -105.5795714935544112, -280.8376638359844151, -285.9686137636504668 ) ) ;
#9948 = ORIENTED_EDGE ( 'NONE', *, *, #41512, .F. ) ;
#9949 = CARTESIAN_POINT ( 'NONE',  ( -110.7416098782010891, -298.7509451859120304, -254.8897257155112186 ) ) ;
#9950 = CARTESIAN_POINT ( 'NONE',  ( -109.7221141836586611, -291.4779942927941647, -282.0719114613131069 ) ) ;
#9951 = CARTESIAN_POINT ( 'NONE',  ( -99.03427638254679266, -291.7161585215891932, -314.7455486226522225 ) ) ;
#9952 = CARTESIAN_POINT ( 'NONE',  ( -87.99525036370171449, -290.6696676790480751, -217.5833860367995953 ) ) ;
#9953 = CARTESIAN_POINT ( 'NONE',  ( 36.63379597003661559, -286.7923764334385055, -249.0258990881542900 ) ) ;
#9954 = CARTESIAN_POINT ( 'NONE',  ( 183.0442525570908288, 275.0000000000000568, 7.500000000000000000 ) ) ;
#9955 = CARTESIAN_POINT ( 'NONE',  ( -26.64676077994170100, -281.3138494874469870, -343.4339249386031270 ) ) ;
#9956 = CARTESIAN_POINT ( 'NONE',  ( -10.25163302473109717, -290.5553476767098005, -339.5320586341034641 ) ) ;
#9957 = CARTESIAN_POINT ( 'NONE',  ( -109.1048677774284528, -282.8124165396556009, -287.1720772192215350 ) ) ;
#9958 = CARTESIAN_POINT ( 'NONE',  ( -6.578175613760438800, -281.7799452396975539, -203.6027257611767709 ) ) ;
#9959 = CARTESIAN_POINT ( 'NONE',  ( -5.712459371392874630, -289.5875332037014687, -340.3068922860259704 ) ) ;
#9960 = CARTESIAN_POINT ( 'NONE',  ( -64.84509111272539883, -280.1753177911814987, -202.6739557870255624 ) ) ;
#9961 = CARTESIAN_POINT ( 'NONE',  ( 35.08225795746511011, -292.0290671447872342, -245.2449159236358867 ) ) ;
#9962 = CARTESIAN_POINT ( 'NONE',  ( 23.72686322068857123, -287.7316625933499381, -223.7049114343797669 ) ) ;
#9963 = CARTESIAN_POINT ( 'NONE',  ( 20.23652376549609500, -287.3519379484955039, -219.2503823002382717 ) ) ;
#9964 = CARTESIAN_POINT ( 'NONE',  ( -91.66362565694265641, -284.0206987331293931, -319.1459847004953758 ) ) ;
#9965 = ORIENTED_EDGE ( 'NONE', *, *, #36530, .F. ) ;
#9966 = LINE ( 'NONE', #80535, #23168 ) ;
#9967 = CARTESIAN_POINT ( 'NONE',  ( 35.09892406273690568, -295.1293097740040139, -248.1651397951241620 ) ) ;
#9968 = CARTESIAN_POINT ( 'NONE',  ( 38.73762242568383130, -292.1291950292558681, -261.7978606863005666 ) ) ;
#9969 = CARTESIAN_POINT ( 'NONE',  ( -64.43129076525022469, -276.4732150278147174, -338.4558663469026669 ) ) ;
#9970 = CARTESIAN_POINT ( 'NONE',  ( -112.7870606520255166, -296.0878875200045854, -255.4169339165041208 ) ) ;
#9971 = CARTESIAN_POINT ( 'NONE',  ( 34.89996748549255301, -291.8418287558436646, -255.8060771180843460 ) ) ;
#9972 = CARTESIAN_POINT ( 'NONE',  ( -94.38034297048322685, -295.4517127757300159, -223.1760903312505491 ) ) ;
#9973 = CARTESIAN_POINT ( 'NONE',  ( -47.06215973795028873, -293.1310087205572472, -197.6105635572535562 ) ) ;
#9974 = CARTESIAN_POINT ( 'NONE',  ( 14.54473894379112231, -295.3808295260497516, -322.2207643882104549 ) ) ;
#9975 = DIRECTION ( 'NONE',  ( 0.000000000000000000, 0.000000000000000000, 1.000000000000000000 ) ) ;
#9976 = CARTESIAN_POINT ( 'NONE',  ( -58.36360920679964437, -293.3229525051447695, -342.5825932733167178 ) ) ;
#9977 = CARTESIAN_POINT ( 'NONE',  ( -103.6897508074134038, -299.0170822937945445, -235.2808793229553430 ) ) ;
#9978 = CARTESIAN_POINT ( 'NONE',  ( 29.01811925908577550, -288.0764112151803147, -239.3807561661215857 ) ) ;
#9979 = CARTESIAN_POINT ( 'NONE',  ( 30.38823470957666117, -277.9667574367251746, -303.5112904689913762 ) ) ;
#9980 = CARTESIAN_POINT ( 'NONE',  ( -51.25563148528563318, -276.0211720234513564, -345.6898059554854399 ) ) ;
#9981 = CARTESIAN_POINT ( 'NONE',  ( -7.722162016759400061, -273.7787423754169254, -199.3398424528018040 ) ) ;
#9982 = CARTESIAN_POINT ( 'NONE',  ( 12.87034856786478798, -280.4245380306837205, -325.3162302230959426 ) ) ;
#9983 = CARTESIAN_POINT ( 'NONE',  ( 3.059882193921571680, -274.9195427624969170, -335.0309020544182772 ) ) ;
#9984 = CARTESIAN_POINT ( 'NONE',  ( -109.7589535603569573, -295.4011480807924386, -257.8317571024118706 ) ) ;
#9985 = DIRECTION ( 'NONE',  ( -1.000000000000000000, -0.000000000000000000, -0.000000000000000000 ) ) ;
#9986 = CARTESIAN_POINT ( 'NONE',  ( -104.4766043141997187, -273.5932745095020096, -241.3053539905463367 ) ) ;
#9987 = CARTESIAN_POINT ( 'NONE',  ( 197.1034181619488663, 25.84651970789479947, 12.27392387986159505 ) ) ;
#9989 = CARTESIAN_POINT ( 'NONE',  ( 21.48244090413423280, -274.7798036787380624, -227.1324187615000767 ) ) ;
#9988 = CARTESIAN_POINT ( 'NONE',  ( -107.2814458553013424, -288.2085156541588731, -298.4117644639158584 ) ) ;
#9990 = CARTESIAN_POINT ( 'NONE',  ( -17.72432682165848306, -288.8058899575905230, -344.8202253137417301 ) ) ;
#9991 = CARTESIAN_POINT ( 'NONE',  ( -51.51647858738688512, -299.8517702051267406, -196.2979200959672994 ) ) ;
#9992 = CARTESIAN_POINT ( 'NONE',  ( -102.8063700430792125, -295.0353824842449058, -234.1063884039852212 ) ) ;
#9993 = CARTESIAN_POINT ( 'NONE',  ( -96.15333330122081179, -283.0818777094344796, -319.8319661097800122 ) ) ;
#9994 = CARTESIAN_POINT ( 'NONE',  ( 155.8725544043011553, 19.96731923950661525, 14.33077026901213635 ) ) ;
#9995 = CARTESIAN_POINT ( 'NONE',  ( -72.45220931098012329, -281.5166370790795440, -336.6495233384585504 ) ) ;
#9996 = MECHANICAL_DESIGN_GEOMETRIC_PRESENTATION_REPRESENTATION (  '', ( #22120 ), #64479 ) ;
#9997 = CARTESIAN_POINT ( 'NONE',  ( 175.2296996224750103, 250.0000000000000568, -25.00000000000000355 ) ) ;
#9998 = CARTESIAN_POINT ( 'NONE',  ( -84.07009452426848384, -290.1878900372651060, -213.7608736298832355 ) ) ;
#9999 = CARTESIAN_POINT ( 'NONE',  ( -104.1342104250410330, -282.2590610662592212, -302.8771847243558000 ) ) ;
#10000 = CARTESIAN_POINT ( 'NONE',  ( 200.3789899249135544, 40.95381314121857486, 10.02076201298226721 ) ) ;
#10001 = DIRECTION ( 'NONE',  ( 0.01273136352371030157, 0.9999189529070979798, 0.000000000000000000 ) ) ;
#10002 = CARTESIAN_POINT ( 'NONE',  ( -94.96042251753112851, -289.2152406154886535, -222.3297927940171235 ) ) ;
#10003 = CARTESIAN_POINT ( 'NONE',  ( -67.35746438392645530, -275.1713385687233426, -203.0437890354925798 ) ) ;
#10004 = CARTESIAN_POINT ( 'NONE',  ( -8.175779688113395949, -283.8837834530419286, -341.2506814278392540 ) ) ;
#10006 = CARTESIAN_POINT ( 'NONE',  ( -88.89429033568079319, -283.8010199160273146, -322.1169842834329415 ) ) ;
#10005 = CARTESIAN_POINT ( 'NONE',  ( 4.094315903279943214, -272.6851563448075808, -207.1138175289611354 ) ) ;
#10007 = CARTESIAN_POINT ( 'NONE',  ( 19.64935706065706711, -277.6314969295889341, -316.9362636418679244 ) ) ;
#10008 = CARTESIAN_POINT ( 'NONE',  ( -61.83427240088293075, -278.1814975978680877, -339.3549167273005196 ) ) ;
#10009 = EDGE_CURVE ( 'NONE', #6373, #73562, #22462, .T. ) ;
#10010 = CARTESIAN_POINT ( 'NONE',  ( 28.03145067257481315, -284.0431787727699202, -307.2277630360985654 ) ) ;
#10011 = EDGE_LOOP ( 'NONE', ( #48919, #75051, #14745, #33558 ) ) ;
#10012 = PLANE ( 'NONE',  #25591 ) ;
#10013 = CARTESIAN_POINT ( 'NONE',  ( -4.504459831131269354, -294.4646721581770521, -340.0226669062264477 ) ) ;
#10014 = CARTESIAN_POINT ( 'NONE',  ( -30.40294396809127164, -288.1200987561765032, -195.9875741171783829 ) ) ;
#10015 = CARTESIAN_POINT ( 'NONE',  ( 114.7448031289451222, -296.6656502513747569, -195.3611179825600175 ) ) ;
#10016 = CARTESIAN_POINT ( 'NONE',  ( -111.2869819898779866, -287.6237833571632905, -305.9350535429201159 ) ) ;
#10017 = CARTESIAN_POINT ( 'NONE',  ( -84.36650604195679648, -278.3427919080723996, -209.7120769616728637 ) ) ;
#10018 = CARTESIAN_POINT ( 'NONE',  ( -95.95035890381885224, -289.6139582180073830, -221.6432655608323330 ) ) ;
#10019 = CARTESIAN_POINT ( 'NONE',  ( -108.4248537068418017, -285.8173032810881296, -289.8481844162884613 ) ) ;
#10020 = CARTESIAN_POINT ( 'NONE',  ( -41.89686238152864917, -278.8704480035421511, -344.2469189503393636 ) ) ;
#10021 = CARTESIAN_POINT ( 'NONE',  ( 13.83864486679501660, -288.1781864971354707, -213.5523415782789414 ) ) ;
#10022 = CARTESIAN_POINT ( 'NONE',  ( 35.60111004784599942, -283.7770093047340652, -287.8613781295371155 ) ) ;
#10023 = CARTESIAN_POINT ( 'NONE',  ( 10.52771815065294625, -276.5787318250444287, -330.7410510484766064 ) ) ;
#10024 = CARTESIAN_POINT ( 'NONE',  ( -91.21590465307482987, -295.3021833736847270, -218.6207752515046536 ) ) ;
#10025 = CARTESIAN_POINT ( 'NONE',  ( -98.57506698344418794, -279.0080531743761867, -223.6547949431706854 ) ) ;
#10026 = CARTESIAN_POINT ( 'NONE',  ( -67.42323911292918126, -299.5746791046591966, -202.2559387275920244 ) ) ;
#10027 = DIRECTION ( 'NONE',  ( 1.000000000000000000, 0.000000000000000000, -0.000000000000000000 ) ) ;
#10028 = DIRECTION ( 'NONE',  ( 0.1727706028203384314, 0.000000000000000000, 0.9849620900324524975 ) ) ;
#10029 = CARTESIAN_POINT ( 'NONE',  ( -94.62145573745037552, -295.3732980830532711, -220.6911650413244388 ) ) ;
#10030 = CARTESIAN_POINT ( 'NONE',  ( 199.2296996224750103, 68.12454877777268791, -4.237361107270372962 ) ) ;
#10031 = CARTESIAN_POINT ( 'NONE',  ( -99.23055486891736621, -277.5229251376787829, -309.2854930727917235 ) ) ;
#10032 = CARTESIAN_POINT ( 'NONE',  ( 13.68846862446016743, -275.9532887817881601, -213.1594267440934800 ) ) ;
#10033 = CARTESIAN_POINT ( 'NONE',  ( 39.47505563341835710, -280.6056632643965258, -269.9435485344857852 ) ) ;
#10034 = CARTESIAN_POINT ( 'NONE',  ( -34.51718406982833187, -290.7764571392863218, -344.3708089446921576 ) ) ;
#10035 = CARTESIAN_POINT ( 'NONE',  ( -106.5295068657478481, -297.6566176777852206, -302.5442680727112474 ) ) ;
#10036 = CARTESIAN_POINT ( 'NONE',  ( -76.86414466607730844, -296.7737164462395185, -336.0428272258292850 ) ) ;
#10037 = CARTESIAN_POINT ( 'NONE',  ( 34.37900947287858600, -295.2744938955358975, -248.8246693847556514 ) ) ;
#10038 = CARTESIAN_POINT ( 'NONE',  ( 31.72305642217235899, -279.1749930202285555, -241.5498731901628275 ) ) ;
#10039 = CARTESIAN_POINT ( 'NONE',  ( -46.66050028238030478, -281.8532458216003533, -196.4545942326763281 ) ) ;
#10040 = CARTESIAN_POINT ( 'NONE',  ( -107.1478338048257513, -294.9718139683891422, -244.3587901969843585 ) ) ;
#10041 = CARTESIAN_POINT ( 'NONE',  ( -99.12771944298239646, -285.5536982517733122, -315.0466683873710849 ) ) ;
#10042 = CARTESIAN_POINT ( 'NONE',  ( 23.79944016464181189, -285.9125904452710643, -229.8218499948106626 ) ) ;
#10043 = CARTESIAN_POINT ( 'NONE',  ( 39.60848648064015265, -280.8954554044021847, -269.9391182948613164 ) ) ;
#10044 = CARTESIAN_POINT ( 'NONE',  ( 175.7043253900435786, 241.9494694207491534, -179.2918632058347157 ) ) ;
#10045 = VERTEX_POINT ( 'NONE', #56044 ) ;
#10046 = CARTESIAN_POINT ( 'NONE',  ( -29.05922573830736511, -287.5240033711278329, -346.3747949725814692 ) ) ;
#10047 = CARTESIAN_POINT ( 'NONE',  ( 4.741015212186894701, -286.3044395497469168, -210.6240142159401216 ) ) ;
#10048 = ORIENTED_EDGE ( 'NONE', *, *, #44981, .T. ) ;
#10049 = CARTESIAN_POINT ( 'NONE',  ( -55.61515296490964744, -284.3616968247805517, -344.8431522612921185 ) ) ;
#10050 = CARTESIAN_POINT ( 'NONE',  ( 32.08059082321670274, -275.5831436183505048, -247.5570882805398014 ) ) ;
#10051 = CARTESIAN_POINT ( 'NONE',  ( -74.51697224360025018, -290.4898246469914511, -203.2828677576506209 ) ) ;
#10052 = CARTESIAN_POINT ( 'NONE',  ( 39.53837978329480762, -282.1621426936807779, -267.0534761568782187 ) ) ;
#10053 = CARTESIAN_POINT ( 'NONE',  ( -113.5000000000000568, -296.0521521680024080, -400.5374811273811702 ) ) ;
#10054 = CARTESIAN_POINT ( 'NONE',  ( -111.0662224004974377, -280.3215223886096510, -250.6280784346119219 ) ) ;
#10055 = CARTESIAN_POINT ( 'NONE',  ( 23.72793881191635279, -281.2598884821137517, -223.4754897898779973 ) ) ;
#10056 = CARTESIAN_POINT ( 'NONE',  ( 27.33386217378598815, -285.4809262143061801, -301.5434626090942629 ) ) ;
#10057 = CARTESIAN_POINT ( 'NONE',  ( -70.65833882835340773, -196.5096356399514548, -360.5769090472070957 ) ) ;
#10058 = ORIENTED_EDGE ( 'NONE', *, *, #70761, .T. ) ;
#10059 = CARTESIAN_POINT ( 'NONE',  ( 32.82880071992069304, -277.2140611204449101, -244.3586328017393896 ) ) ;
#10060 = CARTESIAN_POINT ( 'NONE',  ( -114.3264652396838841, -272.7034455692090091, -284.0776971561411983 ) ) ;
#10061 = CARTESIAN_POINT ( 'NONE',  ( 35.67938640242756776, -279.3717387606615148, -254.8156812153096666 ) ) ;
#10062 = CARTESIAN_POINT ( 'NONE',  ( -109.1442272649399712, -296.0823763066272818, -256.5726169319009955 ) ) ;
#10063 = CARTESIAN_POINT ( 'NONE',  ( 30.84490722477851321, -293.5199719409974932, -305.9997694829770012 ) ) ;
#10064 = DIRECTION ( 'NONE',  ( 0.000000000000000000, 0.000000000000000000, -1.000000000000000000 ) ) ;
#10065 = ADVANCED_FACE ( 'NONE', ( #12482 ), #34266, .F. ) ;
#10067 = CARTESIAN_POINT ( 'NONE',  ( -89.23794897637390022, -288.1974228851292423, -322.8322507112116568 ) ) ;
#10066 = CARTESIAN_POINT ( 'NONE',  ( -72.98945113080966962, -296.1643055656552406, -202.7169034487176589 ) ) ;
#10068 = CARTESIAN_POINT ( 'NONE',  ( -42.45149074866827021, -296.9777029714415448, -344.4202532785936341 ) ) ;
#10069 = ADVANCED_FACE ( 'NONE', ( #63173 ), #41332, .F. ) ;
#10070 = CARTESIAN_POINT ( 'NONE',  ( 32.30261197297213016, -288.5576111756396926, -246.8895762823406699 ) ) ;
#10071 = VERTEX_POINT ( 'NONE', #37702 ) ;
#10072 = CARTESIAN_POINT ( 'NONE',  ( 22.01966288266718408, -293.8377689909356718, -221.6882426259114709 ) ) ;
#10073 = CARTESIAN_POINT ( 'NONE',  ( -107.4157718441762626, -285.3199821643093514, -249.5067965445178686 ) ) ;
#10074 = CARTESIAN_POINT ( 'NONE',  ( -84.95754812396879174, -296.2065547794595091, -210.3549538234418037 ) ) ;
#10075 = CARTESIAN_POINT ( 'NONE',  ( -47.73169993441930359, -292.7262149981494872, -194.1746124373250950 ) ) ;
#10076 = CARTESIAN_POINT ( 'NONE',  ( -22.21203183361346589, -292.7331521495007678, -194.8706375430522542 ) ) ;
#10077 = CARTESIAN_POINT ( 'NONE',  ( -5.790510541521365795, -288.7920068999575847, -336.1906131971953187 ) ) ;
#10078 = ORIENTED_EDGE ( 'NONE', *, *, #83711, .T. ) ;
#10079 = CARTESIAN_POINT ( 'NONE',  ( 157.4851178187871312, 14.99999999999999467, 7.000000000000000888 ) ) ;
#10080 = CARTESIAN_POINT ( 'NONE',  ( -112.7458507401992733, -274.5437195739473282, -264.7578475319475046 ) ) ;
#10081 = CARTESIAN_POINT ( 'NONE',  ( -97.49169456466592010, -271.9848197135761438, -222.9270912740024357 ) ) ;
#10082 = CARTESIAN_POINT ( 'NONE',  ( -2.326675228930831896, -281.6355269625391884, -334.6977382692795686 ) ) ;
#10083 = ORIENTED_EDGE ( 'NONE', *, *, #3472, .F. ) ;
#10084 = CARTESIAN_POINT ( 'NONE',  ( -51.30760475743491611, -276.7337858303380926, -346.0214141156695291 ) ) ;
#10085 = CARTESIAN_POINT ( 'NONE',  ( -103.9181012651606153, -271.3780272389824404, -238.5173866586522138 ) ) ;
#10086 = CARTESIAN_POINT ( 'NONE',  ( -88.39704607707935224, -281.1883556822812125, -216.3992670618211775 ) ) ;
#10087 = CARTESIAN_POINT ( 'NONE',  ( -39.21223733438745995, -275.2154597038931456, -344.5727516631195044 ) ) ;
#10088 = CARTESIAN_POINT ( 'NONE',  ( -108.9760715191731464, -297.5474499343453090, -286.3500936098838565 ) ) ;
#10089 = CARTESIAN_POINT ( 'NONE',  ( -106.5325994041138244, -273.8115654333241764, -246.3605366288671803 ) ) ;
#10090 = CARTESIAN_POINT ( 'NONE',  ( -43.24829040909175859, -299.5790065920785992, -194.3377250612365970 ) ) ;
#10091 = CARTESIAN_POINT ( 'NONE',  ( -24.41638868785404881, -272.2363182896086187, -196.0696849548029661 ) ) ;
#10092 = CARTESIAN_POINT ( 'NONE',  ( 16.80810937755174805, -293.5001679676471440, -221.1779170736596427 ) ) ;
#10093 = CARTESIAN_POINT ( 'NONE',  ( -7.010937760586750223, -291.0328829448560555, -203.3132263463032245 ) ) ;
#10094 = DIRECTION ( 'NONE',  ( -0.6249999999999938938, -1.734723475976788793E-14, -0.7806247497998048956 ) ) ;
#10095 = CARTESIAN_POINT ( 'NONE',  ( -89.16603447433475083, -278.2507182878662206, -327.2273229961910488 ) ) ;
#10096 = CARTESIAN_POINT ( 'NONE',  ( -57.91480052647060006, -298.1122424356454417, -200.2980390700794544 ) ) ;
#10097 =( BOUNDED_SURFACE ( )  B_SPLINE_SURFACE ( 3, 2, ( 
 ( #58744, #50222, #87133 ),
 ( #22284, #979, #93314 ),
 ( #21351, #57814, #29860 ),
 ( #51606, #43133, #21829 ) ),
 .UNSPECIFIED., .F., .F., .F. ) 
 B_SPLINE_SURFACE_WITH_KNOTS ( ( 4, 4 ),
 ( 3, 3 ),
 ( 1.570796326794896558, 2.004620063563922638 ),
 ( 0.000000000000000000, 1.000000000000000000 ),
 .UNSPECIFIED. ) 
 GEOMETRIC_REPRESENTATION_ITEM ( )  RATIONAL_B_SPLINE_SURFACE ( (
 ( 1.000000000000000000, 0.7071067811865475727, 1.000000000000000000),
 ( 1.000000000000000000, 0.7478056585118743049, 1.000000000000000000),
 ( 1.000000000000000000, 0.7849082635113588946, 1.000000000000000000),
 ( 1.000000000000000000, 0.8168508380123956636, 1.000000000000000000) ) ) 
 REPRESENTATION_ITEM ( '' )  SURFACE ( )  );
#10098 = CARTESIAN_POINT ( 'NONE',  ( -90.11020610653490337, -282.4638122541618372, -325.8303726090314285 ) ) ;
#10099 = CARTESIAN_POINT ( 'NONE',  ( 21.74668994224522933, -296.1889464478860532, -316.8424118259868578 ) ) ;
#10100 = DIRECTION ( 'NONE',  ( 0.000000000000000000, -0.000000000000000000, -1.000000000000000000 ) ) ;
#10101 = CARTESIAN_POINT ( 'NONE',  ( -51.05817383886850536, -282.4289799527325613, -342.2769875619526943 ) ) ;
#10102 = CARTESIAN_POINT ( 'NONE',  ( -96.61484122935095797, -281.9193463631676764, -316.5858210636096146 ) ) ;
#10103 = CARTESIAN_POINT ( 'NONE',  ( 34.15471692889155264, -274.3555753317088488, -287.8393355101522957 ) ) ;
#10104 = CARTESIAN_POINT ( 'NONE',  ( 33.33821948033345706, -283.8790948514794650, -295.5995821949775859 ) ) ;
#10105 = EDGE_CURVE ( 'NONE', #5562, #61290, #30617, .T. ) ;
#10106 = CARTESIAN_POINT ( 'NONE',  ( 175.2296996224750103, 250.0000000000000568, -12.00000000000000000 ) ) ;
#10107 = CARTESIAN_POINT ( 'NONE',  ( 175.2296996224750103, 150.9142415853029036, 0.000000000000000000 ) ) ;
#10108 = CARTESIAN_POINT ( 'NONE',  ( -71.03058452618282104, -272.0148575401698849, -202.0127494104979746 ) ) ;
#10109 = CARTESIAN_POINT ( 'NONE',  ( -87.95831559175432801, -279.7582887874198718, -325.9307739391316545 ) ) ;
#10110 = CARTESIAN_POINT ( 'NONE',  ( 194.7510731661265595, -164.3527196417747689, -22.50000000000000000 ) ) ;
#10111 = CARTESIAN_POINT ( 'NONE',  ( -35.21376069421063448, -287.9987906217879754, -194.8181858442258090 ) ) ;
#10112 = FACE_OUTER_BOUND ( 'NONE', #4144, .T. ) ;
#10113 = CARTESIAN_POINT ( 'NONE',  ( -97.53075140976511648, -287.9408460568409964, -315.1290064869051548 ) ) ;
#10114 = CARTESIAN_POINT ( 'NONE',  ( 115.2448031289451222, -299.5541904835127980, -195.3611179825600175 ) ) ;
#10115 = CARTESIAN_POINT ( 'NONE',  ( -78.18336557496067485, -294.4094986319782947, -331.4068473211712558 ) ) ;
#10116 = CARTESIAN_POINT ( 'NONE',  ( -51.00161388006192453, -287.3679922815639998, -343.3812852127429096 ) ) ;
#10117 = CARTESIAN_POINT ( 'NONE',  ( 163.5244876965996923, 234.8495348041943487, -191.6304063886470317 ) ) ;
#10118 = CARTESIAN_POINT ( 'NONE',  ( -105.7715854310686723, -294.1480482822815929, -301.1859095118218761 ) ) ;
#10119 = CARTESIAN_POINT ( 'NONE',  ( 33.22569780964552422, -285.6581705565193943, -241.1893890864233754 ) ) ;
#10120 = CARTESIAN_POINT ( 'NONE',  ( 13.87579997193738457, -282.3847970942553047, -217.1560524550129401 ) ) ;
#10121 = CARTESIAN_POINT ( 'NONE',  ( -97.25939844816508639, -282.1593267596914529, -317.0927287541347255 ) ) ;
#10122 = CARTESIAN_POINT ( 'NONE',  ( -50.75146506802662572, -289.2281088185788462, -342.1705713351223039 ) ) ;
#10123 = CARTESIAN_POINT ( 'NONE',  ( 20.12486279696889113, -282.3331824380979924, -224.3940747368134794 ) ) ;
#10124 = CARTESIAN_POINT ( 'NONE',  ( 33.80958396006374045, -282.5798754056833673, -287.4466660891641254 ) ) ;
#10125 = CARTESIAN_POINT ( 'NONE',  ( -3.770357505852217184, -290.5914139266557186, -337.8392912137360327 ) ) ;
#10126 = CARTESIAN_POINT ( 'NONE',  ( -9.112445462621307612, -298.5631240970153044, -193.3603398670499018 ) ) ;
#10127 = VERTEX_POINT ( 'NONE', #74165 ) ;
#10128 = CARTESIAN_POINT ( 'NONE',  ( 31.85528348125702536, -275.9871838248251947, -304.2579613512853030 ) ) ;
#10129 = CARTESIAN_POINT ( 'NONE',  ( 26.23587654574072658, -295.0036021948311031, -231.1511717593713229 ) ) ;
#10130 = CARTESIAN_POINT ( 'NONE',  ( 123.4306832106270946, -134.2391364535880882, 0.000000000000000000 ) ) ;
#10131 = CARTESIAN_POINT ( 'NONE',  ( 10.64812456238590066, -284.9090924074130271, -330.4860931364851808 ) ) ;
#10132 = CARTESIAN_POINT ( 'NONE',  ( 31.33417417030334562, -273.9515086924911316, -300.9168492442818774 ) ) ;
#10133 = DIRECTION ( 'NONE',  ( -1.000000000000000000, 0.000000000000000000, 0.000000000000000000 ) ) ;
#10134 = CARTESIAN_POINT ( 'NONE',  ( -82.48011783106134942, -295.8474271871073142, -208.9036852808880269 ) ) ;
#10135 = CARTESIAN_POINT ( 'NONE',  ( -109.7193533372791023, -291.9632885458884175, -284.8449515112957897 ) ) ;
#10136 = CARTESIAN_POINT ( 'NONE',  ( -21.90442576873983782, -273.6038279701614329, -198.9077539737049278 ) ) ;
#10137 = CARTESIAN_POINT ( 'NONE',  ( -107.6073616987122961, -291.7785837474815480, -292.7433668894856282 ) ) ;
#10138 = CARTESIAN_POINT ( 'NONE',  ( -32.15253962783823027, -293.0604326010470686, -197.2972348126272664 ) ) ;
#10139 = CARTESIAN_POINT ( 'NONE',  ( -93.31092270817983092, -285.6314681143583130, -318.8099351676286801 ) ) ;
#10140 = CARTESIAN_POINT ( 'NONE',  ( -88.27036707920395031, -292.7803576116512545, -213.3972946026031536 ) ) ;
#10141 = CARTESIAN_POINT ( 'NONE',  ( -68.14567209144453841, -292.9712162624673510, -200.3153229453337474 ) ) ;
#10142 = CARTESIAN_POINT ( 'NONE',  ( -23.52091616408201702, -294.7039990168211148, -342.0924676533860520 ) ) ;
#10143 = CARTESIAN_POINT ( 'NONE',  ( 36.53301821903620805, -289.3823685584699206, -257.1255174045505782 ) ) ;
#10144 = CARTESIAN_POINT ( 'NONE',  ( 30.72081916722495620, -281.2525881705676056, -234.2405979524541522 ) ) ;
#10145 = CARTESIAN_POINT ( 'NONE',  ( -59.69825073501958457, -295.8447726425897599, -198.1297826147653609 ) ) ;
#10146 = CARTESIAN_POINT ( 'NONE',  ( -73.61113752822717515, -285.4180740325126635, -202.3791087334140002 ) ) ;
#10147 = CARTESIAN_POINT ( 'NONE',  ( -4.316170957139710218, -278.5946439040762357, -337.3167994299263910 ) ) ;
#10148 = CARTESIAN_POINT ( 'NONE',  ( -67.96394637331074762, -282.2583143925389209, -337.0650049825287056 ) ) ;
#10149 = CARTESIAN_POINT ( 'NONE',  ( 0.5342371799079419503, -284.5567248701766516, -205.6127680648015996 ) ) ;
#10150 = CARTESIAN_POINT ( 'NONE',  ( -73.52809004499295042, -275.6665682240818001, -336.9405167085677704 ) ) ;
#10151 = CARTESIAN_POINT ( 'NONE',  ( -90.79075242949535607, -283.3441026381856886, -320.1726352228607198 ) ) ;
#10152 = CARTESIAN_POINT ( 'NONE',  ( -92.79695670519626560, -280.4841258988446953, -217.4390897427107916 ) ) ;
#10153 = CARTESIAN_POINT ( 'NONE',  ( 39.46685440826993130, -286.6259363707403054, -271.5596149658285299 ) ) ;
#10154 = CARTESIAN_POINT ( 'NONE',  ( 36.65600694997950626, -295.3532716960980906, -273.5100338923014647 ) ) ;
#10155 = CARTESIAN_POINT ( 'NONE',  ( 13.41624474028927949, -276.3482778430423537, -213.4569064507844018 ) ) ;
#10156 = CARTESIAN_POINT ( 'NONE',  ( 38.89054924633138910, -276.9488411776949874, -276.8374153150747929 ) ) ;
#10157 = CARTESIAN_POINT ( 'NONE',  ( -107.1172517035466427, -278.0992445922971683, -291.9866930412447346 ) ) ;
#10158 = CARTESIAN_POINT ( 'NONE',  ( -50.29569844190492489, -299.8865635541124561, -196.6575064599604445 ) ) ;
#10159 = CARTESIAN_POINT ( 'NONE',  ( 3.467602521227912238, -284.6021483056375700, -207.6344949091392209 ) ) ;
#10160 = CARTESIAN_POINT ( 'NONE',  ( -113.4512549875592669, -292.1053734450758270, -274.0727312007828687 ) ) ;
#10161 = CARTESIAN_POINT ( 'NONE',  ( 22.84956097576515788, -291.8914287828226293, -228.4911966137762249 ) ) ;
#10162 = ORIENTED_EDGE ( 'NONE', *, *, #76002, .T. ) ;
#10163 = CARTESIAN_POINT ( 'NONE',  ( -41.58982485106410110, -291.6640339373761890, -197.4137883815997441 ) ) ;
#10164 = ORIENTED_EDGE ( 'NONE', *, *, #49321, .F. ) ;
#10165 = CARTESIAN_POINT ( 'NONE',  ( 10.04777681131517753, -289.4963247613467843, -330.7257015966046652 ) ) ;
#10166 = CARTESIAN_POINT ( 'NONE',  ( -106.5439089563936363, -279.5180439181236807, -246.6483046272178399 ) ) ;
#10167 = CARTESIAN_POINT ( 'NONE',  ( -95.32831459019224951, -296.1539164530156540, -220.0917893130943526 ) ) ;
#10168 = CARTESIAN_POINT ( 'NONE',  ( 36.29019357390585299, -288.4827483429384642, -292.5802086880315187 ) ) ;
#10169 = CARTESIAN_POINT ( 'NONE',  ( 7.528161383712674848, -286.9787604703238912, -207.7459693148948645 ) ) ;
#10170 = CARTESIAN_POINT ( 'NONE',  ( -108.1126704104220408, -284.6480869448288331, -288.3488152268273552 ) ) ;
#10171 = CARTESIAN_POINT ( 'NONE',  ( -63.92340429282429426, -182.6668603218660110, -362.3860721358306591 ) ) ;
#10172 = CARTESIAN_POINT ( 'NONE',  ( -114.2273371156044419, -271.8154644092875287, -270.3517381826829364 ) ) ;
#10173 = CARTESIAN_POINT ( 'NONE',  ( -105.9079042852521724, -259.8726411093065281, -315.4770811649867142 ) ) ;
#10174 = CARTESIAN_POINT ( 'NONE',  ( 7.671714976775490413, -275.6170801770783783, -328.1005658895440433 ) ) ;
#10175 = CARTESIAN_POINT ( 'NONE',  ( -96.34996190552394069, -276.8651456401346991, -313.8821771061226400 ) ) ;
#10176 = CARTESIAN_POINT ( 'NONE',  ( -36.17924183282816841, -297.5739966270660943, -193.4227500555989820 ) ) ;
#10177 = CARTESIAN_POINT ( 'NONE',  ( -92.70013282893863504, -239.9236592119154068, -339.3243185181465833 ) ) ;
#10178 = ADVANCED_FACE ( 'NONE', ( #23038 ), #80617, .T. ) ;
#10179 = CARTESIAN_POINT ( 'NONE',  ( -112.0068190795022360, -277.0269596698151986, -287.0469888637583722 ) ) ;
#10180 = CARTESIAN_POINT ( 'NONE',  ( -56.07532559092211244, -289.7922409103848622, -341.0326937406983348 ) ) ;
#10181 = CARTESIAN_POINT ( 'NONE',  ( -54.56892408893858715, -298.6390384708890906, -195.4786662692471850 ) ) ;
#10182 = CARTESIAN_POINT ( 'NONE',  ( -9.144628575790221703, -298.8886658643957617, -193.4203677221946123 ) ) ;
#10183 = CARTESIAN_POINT ( 'NONE',  ( -84.47648351393847577, -295.8887955996117967, -326.1707564084852038 ) ) ;
#10184 = VERTEX_POINT ( 'NONE', #66157 ) ;
#10185 = CARTESIAN_POINT ( 'NONE',  ( -67.11819910758798358, -279.3596221247182712, -339.8065952184603589 ) ) ;
#10186 = CARTESIAN_POINT ( 'NONE',  ( 38.60608843914693011, -281.2148746239572574, -282.7502950367433527 ) ) ;
#10187 = CARTESIAN_POINT ( 'NONE',  ( -95.50993420718145899, -279.0067352305165969, -314.9781844332607648 ) ) ;
#10188 = CARTESIAN_POINT ( 'NONE',  ( -17.59929120633848498, -278.5610087195860274, -343.7383031384256924 ) ) ;
#10189 = CARTESIAN_POINT ( 'NONE',  ( -103.0503548012665220, -295.5743320823794988, -237.1154376743350554 ) ) ;
#10190 = CARTESIAN_POINT ( 'NONE',  ( 197.1858402786432976, 68.15263271079744811, -10.54024884218787861 ) ) ;
#10191 = CARTESIAN_POINT ( 'NONE',  ( -109.0428824163552122, -278.5371153705501683, -284.1362938232264810 ) ) ;
#10192 = CARTESIAN_POINT ( 'NONE',  ( -46.87112713944789277, -274.7368936531498207, -194.1157978571005742 ) ) ;
#10193 = CARTESIAN_POINT ( 'NONE',  ( -36.11167595217053616, -287.7218987114288211, -346.8711073633154456 ) ) ;
#10194 = CARTESIAN_POINT ( 'NONE',  ( -80.13080328560668875, -275.4735302345370656, -208.7019593804574242 ) ) ;
#10195 = CARTESIAN_POINT ( 'NONE',  ( -5.546632951704859593, -275.2167925460005904, -339.8426263003461258 ) ) ;
#10196 = CARTESIAN_POINT ( 'NONE',  ( 194.7453183674699915, 20.99999999999998934, -15.62500000000000355 ) ) ;
#10197 = CARTESIAN_POINT ( 'NONE',  ( -26.46094893164605111, -288.1074540088904428, -342.7601267447482201 ) ) ;
#10198 = CARTESIAN_POINT ( 'NONE',  ( -93.83920180759402285, -284.6126480565598058, -218.1165754562210282 ) ) ;
#10199 = CARTESIAN_POINT ( 'NONE',  ( 26.42078663225346347, -280.3023481343462890, -308.0431775669642889 ) ) ;
#10201 = CARTESIAN_POINT ( 'NONE',  ( -96.90372463458312779, -283.2466710020319169, -225.7104803923780025 ) ) ;
#10200 = CARTESIAN_POINT ( 'NONE',  ( 34.91624772855234227, -279.9436624269526988, -256.3603788803147836 ) ) ;
#10202 = CARTESIAN_POINT ( 'NONE',  ( 35.61719817010499867, -289.7761356342125509, -287.7933291413360166 ) ) ;
#10203 = CARTESIAN_POINT ( 'NONE',  ( -51.92116565394568539, -281.0666257315007783, -198.3746223163297202 ) ) ;
#10204 = CARTESIAN_POINT ( 'NONE',  ( -91.70447742415792902, -271.2771939939169670, -218.6733493027779502 ) ) ;
#10205 = CARTESIAN_POINT ( 'NONE',  ( -8.362205511353741016, -281.0790322659028107, -340.8913788330370949 ) ) ;
#10206 = CARTESIAN_POINT ( 'NONE',  ( 36.35513471837756327, -295.3735751972777166, -256.4407305996601281 ) ) ;
#10207 = CARTESIAN_POINT ( 'NONE',  ( -61.70127681933101371, -277.9798863685323909, -198.3293505369994421 ) ) ;
#10208 = CARTESIAN_POINT ( 'NONE',  ( -93.02351920001959229, -285.8494174591913293, -320.8734022832099413 ) ) ;
#10209 = EDGE_CURVE ( 'NONE', #16726, #49537, #91137, .T. ) ;
#10210 = DIRECTION ( 'NONE',  ( 1.124465274301078034E-16, 1.000000000000000000, 0.000000000000000000 ) ) ;
#10211 = CARTESIAN_POINT ( 'NONE',  ( -30.84590118463275488, -294.0536633378663964, -195.0290780358346012 ) ) ;
#10212 = CARTESIAN_POINT ( 'NONE',  ( -26.76394431292573728, -274.9174345958816161, -344.6114494878838173 ) ) ;
#10213 = CARTESIAN_POINT ( 'NONE',  ( 38.81658475733406988, -286.6214677874908716, -260.1594287254835649 ) ) ;
#10214 = CARTESIAN_POINT ( 'NONE',  ( -108.5181154060295370, -289.2069024782649080, -250.8583406240022953 ) ) ;
#10215 = CARTESIAN_POINT ( 'NONE',  ( -48.18343439339133027, -273.4097382618878100, -437.2279360942110884 ) ) ;
#10216 = CARTESIAN_POINT ( 'NONE',  ( -26.96834898235329447, -275.6023107238194143, -343.1185029215001236 ) ) ;
#10217 = CARTESIAN_POINT ( 'NONE',  ( 4.493271659766628900, -292.6205742437894060, -331.6856694591111250 ) ) ;
#10218 = CARTESIAN_POINT ( 'NONE',  ( -109.1409294045881921, -291.6610567551922486, -286.1075840467784133 ) ) ;
#10219 = DIRECTION ( 'NONE',  ( -0.000000000000000000, -0.000000000000000000, 1.000000000000000000 ) ) ;
#10220 = DIRECTION ( 'NONE',  ( -0.5877852522924792433, 0.000000000000000000, -0.8090169943749430104 ) ) ;
#10221 = CARTESIAN_POINT ( 'NONE',  ( -2.356313950823147430, -290.9863782981959730, -202.5325314325094155 ) ) ;
#10222 = CARTESIAN_POINT ( 'NONE',  ( -98.02524546373331304, -286.7313162073454009, -228.3393937628766537 ) ) ;
#10223 = CARTESIAN_POINT ( 'NONE',  ( -57.04997751865148814, -287.5426944628267165, -343.8018626579952866 ) ) ;
#10224 = CARTESIAN_POINT ( 'NONE',  ( 34.56795388107262568, -288.7728585527140694, -254.7285692698352761 ) ) ;
#10225 = DIRECTION ( 'NONE',  ( 0.000000000000000000, 0.000000000000000000, -1.000000000000000000 ) ) ;
#10226 = CARTESIAN_POINT ( 'NONE',  ( 32.42449883106665709, -288.0631121276574618, -248.2901417484223998 ) ) ;
#10227 = CARTESIAN_POINT ( 'NONE',  ( 36.18473302662236790, -295.7436520320890736, -286.9200640117798571 ) ) ;
#10228 = DIRECTION ( 'NONE',  ( 1.000000000000000000, 0.000000000000000000, -0.000000000000000000 ) ) ;
#10229 = CARTESIAN_POINT ( 'NONE',  ( 38.95335154249851684, -288.8434771316233878, -277.2221535033768305 ) ) ;
#10230 = CARTESIAN_POINT ( 'NONE',  ( -28.78878386451603077, -275.0244982364519046, -345.4880653501502366 ) ) ;
#10231 = CARTESIAN_POINT ( 'NONE',  ( -112.4628415868304927, -278.6751479787206449, -287.1705914307327134 ) ) ;
#10232 = CARTESIAN_POINT ( 'NONE',  ( -19.75692733029804771, -279.9388520060445558, -195.3629160498394413 ) ) ;
#10233 = CARTESIAN_POINT ( 'NONE',  ( -110.5503374789901443, -274.6503120203589106, -256.6012278311616797 ) ) ;
#10234 = CARTESIAN_POINT ( 'NONE',  ( -48.18343439339133738, -283.1093320178188151, -507.6442049081570076 ) ) ;
#10235 = CARTESIAN_POINT ( 'NONE',  ( -78.11557340748808542, -283.5042462359920705, -207.3511836032612337 ) ) ;
#10236 = CARTESIAN_POINT ( 'NONE',  ( -48.18343439339132317, -257.0657538259918056, -487.6787901984505993 ) ) ;
#10237 = CARTESIAN_POINT ( 'NONE',  ( -102.9596153327663899, -276.2267463756935513, -305.0764558297605049 ) ) ;
#10238 = CARTESIAN_POINT ( 'NONE',  ( 21.80942542596930522, -280.1846917477959096, -316.4920030215609472 ) ) ;
#10239 = DIRECTION ( 'NONE',  ( 0.000000000000000000, 0.000000000000000000, 1.000000000000000000 ) ) ;
#10240 = CARTESIAN_POINT ( 'NONE',  ( -64.86324294991916872, -275.8849138629798858, -341.5876313529131494 ) ) ;
#10241 = CARTESIAN_POINT ( 'NONE',  ( -109.8205513100066923, -297.8972559847620687, -283.7547328870899719 ) ) ;
#10242 = CARTESIAN_POINT ( 'NONE',  ( -24.59853707242006138, -281.8136528006235153, -346.0397750232514227 ) ) ;
#10243 = CARTESIAN_POINT ( 'NONE',  ( -109.5930965613321320, -297.3360860732462925, -282.3254049177900811 ) ) ;
#10244 = CARTESIAN_POINT ( 'NONE',  ( -95.20915907490611119, -298.5483749017658965, -220.2354958050128459 ) ) ;
#10245 = CARTESIAN_POINT ( 'NONE',  ( -38.07831613456096420, -273.7093883448439442, -197.3436893526007907 ) ) ;
#10246 = CARTESIAN_POINT ( 'NONE',  ( 34.53876013362178554, -295.2744938962945298, -248.7767584772300893 ) ) ;
#10247 = CARTESIAN_POINT ( 'NONE',  ( 39.57750989701042243, -287.6619923767982527, -265.8162808339412209 ) ) ;
#10248 = EDGE_CURVE ( 'NONE', #26035, #12543, #85155, .T. ) ;
#10249 = CARTESIAN_POINT ( 'NONE',  ( -110.3335092408794793, -276.8818024192555072, -250.7789467683004148 ) ) ;
#10250 = CARTESIAN_POINT ( 'NONE',  ( -103.7994992477873382, -289.8781369429692063, -309.3556701720384581 ) ) ;
#10251 = CARTESIAN_POINT ( 'NONE',  ( 33.94209871645041687, -286.3893603965388479, -253.5131804390862840 ) ) ;
#10252 = CIRCLE ( 'NONE', #76851, 1.000000000000000888 ) ;
#10253 = CARTESIAN_POINT ( 'NONE',  ( 32.60700415657181850, -291.1984148600584490, -243.1586569170810037 ) ) ;
#10254 = VERTEX_POINT ( 'NONE', #23518 ) ;
#10255 = CARTESIAN_POINT ( 'NONE',  ( -87.49538389815894845, -233.3606102865802825, -350.3678815354037965 ) ) ;
#10256 = CARTESIAN_POINT ( 'NONE',  ( -53.42817283331326195, -288.7717729141947416, -341.6297214300688552 ) ) ;
#10257 = CARTESIAN_POINT ( 'NONE',  ( 203.4339565214082484, 300.2380916213085698, -4.962874975894024487 ) ) ;
#10258 = CARTESIAN_POINT ( 'NONE',  ( -95.14962286871472941, -284.8081800909218373, -320.8691795352419263 ) ) ;
#10259 = CARTESIAN_POINT ( 'NONE',  ( 6.372108086694794338, -291.6889415811791082, -207.2586363850788302 ) ) ;
#10260 = CARTESIAN_POINT ( 'NONE',  ( 10.50148642365074458, -282.0119367044794103, -210.5912354193176270 ) ) ;
#10261 = CARTESIAN_POINT ( 'NONE',  ( -29.44676271388765443, -282.7828264192551160, -342.9834478464072731 ) ) ;
#10262 = CARTESIAN_POINT ( 'NONE',  ( -60.14808920178801799, -297.7646175120970042, -196.7605850772471285 ) ) ;
#10263 = CARTESIAN_POINT ( 'NONE',  ( -29.95685567321685028, -275.4627549194695462, -197.2399339783096366 ) ) ;
#10264 = CARTESIAN_POINT ( 'NONE',  ( 23.15217351307708071, -290.9737571614758735, -226.6090854255345732 ) ) ;
#10265 = CARTESIAN_POINT ( 'NONE',  ( 31.49601424749674194, -274.0093413072679027, -244.8954629979639037 ) ) ;
#10266 = EDGE_LOOP ( 'NONE', ( #14633, #78886, #92170, #83436 ) ) ;
#10267 = DIRECTION ( 'NONE',  ( -0.000000000000000000, -1.000000000000000000, -0.000000000000000000 ) ) ;
#10268 = CARTESIAN_POINT ( 'NONE',  ( -106.9193925465138619, -286.8187775050571986, -243.8987123139515916 ) ) ;
#10269 = CARTESIAN_POINT ( 'NONE',  ( -3.353359851643989309, -295.6936313495563695, -339.1236478617678358 ) ) ;
#10270 = CARTESIAN_POINT ( 'NONE',  ( -110.0967273144564729, -285.3038630400230886, -262.7476688479676454 ) ) ;
#10271 = ADVANCED_FACE ( 'NONE', ( #16872 ), #73066, .T. ) ;
#10272 = CARTESIAN_POINT ( 'NONE',  ( -42.80143333554335783, -276.1782196752573668, -346.9314224506559867 ) ) ;
#10273 = CARTESIAN_POINT ( 'NONE',  ( 33.22756055264529351, -293.8137437942107795, -239.8112860147130618 ) ) ;
#10274 = CARTESIAN_POINT ( 'NONE',  ( 36.89321148757449720, -285.8842855372855638, -285.5098268696603441 ) ) ;
#10275 = CARTESIAN_POINT ( 'NONE',  ( -61.68591932957613011, -292.0776848538222339, -197.2768761179004002 ) ) ;
#10276 = CARTESIAN_POINT ( 'NONE',  ( -105.1310912312631274, -290.5206457733049774, -297.6387637713704635 ) ) ;
#10277 = CARTESIAN_POINT ( 'NONE',  ( 184.5340210998923283, 2.974099043298211953, 8.999832278985701706 ) ) ;
#10278 = LINE ( 'NONE', #54305, #52323 ) ;
#10279 = CARTESIAN_POINT ( 'NONE',  ( -93.27324509058188085, -239.1325559268020413, -338.6579388652390890 ) ) ;
#10280 = CARTESIAN_POINT ( 'NONE',  ( -108.6480783087754673, -285.7235663197366762, -297.6764020543627112 ) ) ;
#10281 = CARTESIAN_POINT ( 'NONE',  ( -88.47809603358389552, -270.9094976428775681, -206.1857440867352693 ) ) ;
#10282 = VERTEX_POINT ( 'NONE', #67546 ) ;
#10283 = CARTESIAN_POINT ( 'NONE',  ( -76.30300386764839971, -282.5063803985242998, -332.5198139222908935 ) ) ;
#10284 = CARTESIAN_POINT ( 'NONE',  ( -101.8711769383539973, -278.7713472362274274, -228.2921695624654319 ) ) ;
#10285 = CARTESIAN_POINT ( 'NONE',  ( 19.91308581191904992, -284.2201907251176181, -318.5673018594951600 ) ) ;
#10286 = CARTESIAN_POINT ( 'NONE',  ( -37.46467321658223426, -140.8945144798868796, -363.2317121015391876 ) ) ;
#10287 = CARTESIAN_POINT ( 'NONE',  ( 15.33410500464692916, -280.8999378708354584, -325.7133161811123614 ) ) ;
#10288 = CARTESIAN_POINT ( 'NONE',  ( -10.12732785420929993, -284.4292567008990886, -200.8402730129305667 ) ) ;
#10289 = CARTESIAN_POINT ( 'NONE',  ( -36.92663226300399515, -299.8174149814702218, -194.3743222947530285 ) ) ;
#10290 = CARTESIAN_POINT ( 'NONE',  ( -103.9901835675098170, -296.6401548799878469, -300.4174900717001151 ) ) ;
#10291 = ORIENTED_EDGE ( 'NONE', *, *, #15662, .T. ) ;
#10292 = CARTESIAN_POINT ( 'NONE',  ( 36.02814424497211832, -292.1706409147439558, -265.2989475582161845 ) ) ;
#10293 = CARTESIAN_POINT ( 'NONE',  ( -87.02300592960000358, -278.3740139169520944, -329.1255920172828837 ) ) ;
#10294 = CARTESIAN_POINT ( 'NONE',  ( 7.330913109455482690, -274.6808826745287320, -212.6258806787310505 ) ) ;
#10295 = CARTESIAN_POINT ( 'NONE',  ( 35.76380224712765710, -274.7649475973900053, -293.5360620422601414 ) ) ;
#10296 = CARTESIAN_POINT ( 'NONE',  ( -43.18343439339132317, -296.0521521680024080, -507.6442049081570076 ) ) ;
#10297 = CARTESIAN_POINT ( 'NONE',  ( -86.98819434208871826, -271.3613346296446593, -214.0767188238760923 ) ) ;
#10298 = ADVANCED_FACE ( 'NONE', ( #74641 ), #39770, .T. ) ;
#10299 = CARTESIAN_POINT ( 'NONE',  ( -66.68128284574058284, -296.8542974108967201, -340.9287008893612665 ) ) ;
#10300 = CARTESIAN_POINT ( 'NONE',  ( 180.6209651459523968, 214.5000000000000568, -24.41176470588237635 ) ) ;
#10301 = DIRECTION ( 'NONE',  ( -1.000000000000000000, -0.000000000000000000, -0.000000000000000000 ) ) ;
#10302 = CARTESIAN_POINT ( 'NONE',  ( -108.0556988070586186, -285.3769238926561798, -289.7412608358204693 ) ) ;
#10303 = CARTESIAN_POINT ( 'NONE',  ( -19.13912501052385196, -284.5813070729971059, -344.1896083012179020 ) ) ;
#10304 = CARTESIAN_POINT ( 'NONE',  ( -85.78750485434918005, -284.7091102478266862, -215.5495495058500524 ) ) ;
#10305 = CARTESIAN_POINT ( 'NONE',  ( 18.90505728240352212, -274.6240509143686381, -318.1391746373007550 ) ) ;
#10306 = CARTESIAN_POINT ( 'NONE',  ( -0.6207420685548373784, -284.4191026330416321, -334.8780670751054913 ) ) ;
#10307 = CARTESIAN_POINT ( 'NONE',  ( -111.0858159587314304, -277.0286215410363297, -270.6213641411571302 ) ) ;
#10308 = CARTESIAN_POINT ( 'NONE',  ( -35.09444310858130223, -278.1029459916901487, -343.6357787480302477 ) ) ;
#10309 = CARTESIAN_POINT ( 'NONE',  ( 175.2296996224750103, 133.0000000000000000, 0.000000000000000000 ) ) ;
#10310 = CARTESIAN_POINT ( 'NONE',  ( -113.0790570439091454, -279.5174289858325665, -257.3991895727211272 ) ) ;
#10311 = CARTESIAN_POINT ( 'NONE',  ( 21.91929506839649022, -281.3843462366525046, -221.2931920857381556 ) ) ;
#10312 = ORIENTED_EDGE ( 'NONE', *, *, #29988, .F. ) ;
#10313 = EDGE_LOOP ( 'NONE', ( #27297, #14258 ) ) ;
#10314 = EDGE_CURVE ( 'NONE', #82861, #22798, #39670, .T. ) ;
#10315 = CARTESIAN_POINT ( 'NONE',  ( 175.2296996224750103, 250.0000000000000568, 0.000000000000000000 ) ) ;
#10316 = CARTESIAN_POINT ( 'NONE',  ( 34.66753030953182702, -289.1094158056665151, -246.6355643639198263 ) ) ;
#10317 = CARTESIAN_POINT ( 'NONE',  ( -69.31890438994363990, -296.8174145899420751, -204.5579255435971504 ) ) ;
#10318 = CARTESIAN_POINT ( 'NONE',  ( -111.8937015277938229, -290.1375104559436977, -251.4583844874519514 ) ) ;
#10319 = CARTESIAN_POINT ( 'NONE',  ( 35.75654100019524861, -285.9440182258103391, -282.0443685116068195 ) ) ;
#10321 = CARTESIAN_POINT ( 'NONE',  ( -102.5463514248387611, -288.3197446232850893, -305.4887994554308079 ) ) ;
#10320 = CARTESIAN_POINT ( 'NONE',  ( -30.45823730249263050, -284.7154833707213015, -197.0433212968430894 ) ) ;
#10322 = AXIS2_PLACEMENT_3D ( 'NONE', #81885, #74812, #9927 ) ;
#10323 = CARTESIAN_POINT ( 'NONE',  ( 9.270903025119748619, -287.9144461534589823, -213.6654767840914531 ) ) ;
#10324 = CARTESIAN_POINT ( 'NONE',  ( -42.68965519938510766, -275.1194821093689029, -345.1702085131020112 ) ) ;
#10325 = CARTESIAN_POINT ( 'NONE',  ( 26.76066079865502090, -286.4993076210790832, -311.6570068035015879 ) ) ;
#10326 = CARTESIAN_POINT ( 'NONE',  ( -0.7157412622314297534, -288.5387744371663530, -204.8977065826459238 ) ) ;
#10327 = CARTESIAN_POINT ( 'NONE',  ( 33.33962356623377588, -285.8846397867724818, -296.0893293781351190 ) ) ;
#10328 = CARTESIAN_POINT ( 'NONE',  ( -29.40728608658041665, -283.8905798774223967, -343.2159982785695433 ) ) ;
#10329 = CARTESIAN_POINT ( 'NONE',  ( -62.13433141903735901, -291.3738143722598579, -341.3763799180966885 ) ) ;
#10330 = CARTESIAN_POINT ( 'NONE',  ( 175.2296996224750103, 158.6892791692949629, 0.000000000000000000 ) ) ;
#10331 = FACE_OUTER_BOUND ( 'NONE', #85263, .T. ) ;
#10332 = CARTESIAN_POINT ( 'NONE',  ( -48.77666737481985137, -299.8279071822468609, -195.6187238604632626 ) ) ;
#10333 = CARTESIAN_POINT ( 'NONE',  ( 11.18383693049203309, -280.3803540264718208, -327.6156944722021649 ) ) ;
#10334 = CARTESIAN_POINT ( 'NONE',  ( -36.37011880712959311, -291.2612149078244670, -193.5157311925835870 ) ) ;
#10335 = CARTESIAN_POINT ( 'NONE',  ( -107.4605578002511805, -295.2561064065175742, -247.1821617651352483 ) ) ;
#10336 = CARTESIAN_POINT ( 'NONE',  ( 31.81298249496248332, -280.5678454737161474, -295.3886556471273366 ) ) ;
#10337 = CARTESIAN_POINT ( 'NONE',  ( 31.51597371762045086, -273.2586846197522163, -241.9425349285816651 ) ) ;
#10338 = CARTESIAN_POINT ( 'NONE',  ( -90.75420235055038631, -297.1443569384984471, -320.9155540161502813 ) ) ;
#10339 = DIRECTION ( 'NONE',  ( -0.000000000000000000, -0.000000000000000000, -1.000000000000000000 ) ) ;
#10340 = CARTESIAN_POINT ( 'NONE',  ( -31.95084658018009094, -296.5983711020932105, -194.0558108093565295 ) ) ;
#10341 = CARTESIAN_POINT ( 'NONE',  ( 37.07360994593462777, -291.9868439027692943, -285.7343298523142607 ) ) ;
#10342 = CARTESIAN_POINT ( 'NONE',  ( -72.92767687482512429, -292.9965010862782151, -205.8910156031611791 ) ) ;
#10343 = LINE ( 'NONE', #2791, #62600 ) ;
#10344 = CARTESIAN_POINT ( 'NONE',  ( 34.87167903853408291, -294.1994283913480217, -258.5427603614354553 ) ) ;
#10345 = CARTESIAN_POINT ( 'NONE',  ( 204.6539576904058606, 296.7472757692770529, -7.500000000000000000 ) ) ;
#10347 = CARTESIAN_POINT ( 'NONE',  ( 32.34680181013401068, -293.8402056837952614, -292.0984751725993647 ) ) ;
#10346 = CARTESIAN_POINT ( 'NONE',  ( -33.17544088809017211, -281.0200632758420625, -345.6139159875704081 ) ) ;
#10348 = CARTESIAN_POINT ( 'NONE',  ( 37.19180675334335007, -281.7941203473868654, -289.6938971918879133 ) ) ;
#10349 = CARTESIAN_POINT ( 'NONE',  ( -14.68332004295251991, -282.2635479267149776, -198.2235943804611225 ) ) ;
#10350 = CARTESIAN_POINT ( 'NONE',  ( -23.78545685063492954, -285.8874039504225948, -194.5311109862090007 ) ) ;
#10351 = CARTESIAN_POINT ( 'NONE',  ( -112.1399717792138375, -288.5055117233392252, -273.9726583450377007 ) ) ;
#10352 = FACE_OUTER_BOUND ( 'NONE', #47267, .T. ) ;
#10353 = CARTESIAN_POINT ( 'NONE',  ( -5.760299601673096959, -281.1242569195130159, -339.8256621444779171 ) ) ;
#10354 = CARTESIAN_POINT ( 'NONE',  ( 19.38629957467626852, -287.1769087218513050, -321.9890706773002762 ) ) ;
#10355 = CARTESIAN_POINT ( 'NONE',  ( 207.1352294840503134, 30.54719743553542344, 14.49999997652496475 ) ) ;
#10356 = CARTESIAN_POINT ( 'NONE',  ( -23.34738004351993013, -296.4705231276534505, -342.8743100118807661 ) ) ;
#10357 = CARTESIAN_POINT ( 'NONE',  ( 36.67255589461953491, -277.2168581614968161, -289.3478554576635133 ) ) ;
#10359 = CARTESIAN_POINT ( 'NONE',  ( -95.62606371277487938, -278.8368537839979240, -226.3514971737146482 ) ) ;
#10358 = CARTESIAN_POINT ( 'NONE',  ( 37.18600708022069767, -291.7145815150284989, -281.4978886730869476 ) ) ;
#10360 = CARTESIAN_POINT ( 'NONE',  ( -8.513188748562830810, -292.5859176008610802, -198.9614195507538454 ) ) ;
#10361 = CARTESIAN_POINT ( 'NONE',  ( -112.8858941111470813, -282.6729117403816645, -267.1507352859035791 ) ) ;
#10362 = CARTESIAN_POINT ( 'NONE',  ( -34.34483341811321822, -279.0146256576710471, -345.3012236743965673 ) ) ;
#10363 = CARTESIAN_POINT ( 'NONE',  ( 19.00648301982591093, -293.2722682122375204, -317.1402875428370862 ) ) ;
#10364 = CARTESIAN_POINT ( 'NONE',  ( -32.05918893263172720, -296.1181216209474769, -195.3629102556025998 ) ) ;
#10365 = ORIENTED_EDGE ( 'NONE', *, *, #40665, .F. ) ;
#10366 = DIRECTION ( 'NONE',  ( -1.000000000000000000, 0.000000000000000000, 0.000000000000000000 ) ) ;
#10367 = CARTESIAN_POINT ( 'NONE',  ( -104.8683284471737664, -280.9538156128166975, -238.4275723611758337 ) ) ;
#10368 = CARTESIAN_POINT ( 'NONE',  ( 33.70908018399811112, -292.8347742835921963, -253.2848703240079260 ) ) ;
#10369 = CARTESIAN_POINT ( 'NONE',  ( 175.2296996224750103, 250.0000000000000568, 24.50000000000000355 ) ) ;
#10370 = CARTESIAN_POINT ( 'NONE',  ( -67.68488546085839630, -289.1237833571631768, -207.2794874003663779 ) ) ;
#10371 = CARTESIAN_POINT ( 'NONE',  ( -40.41878504565425345, -297.0732436160367911, -193.6061401274947684 ) ) ;
#10372 = CARTESIAN_POINT ( 'NONE',  ( -29.53004843166437610, -287.4643031591140243, -194.2541119313540037 ) ) ;
#10373 = CARTESIAN_POINT ( 'NONE',  ( -34.58012825362258269, -288.8499472898386102, -343.3584463376331541 ) ) ;
#10374 = CARTESIAN_POINT ( 'NONE',  ( -91.82231812343631816, -280.7771267792291496, -220.7368294145919947 ) ) ;
#10375 = CARTESIAN_POINT ( 'NONE',  ( -107.0688381692570488, -274.4703356156919085, -246.1833051132217918 ) ) ;
#10376 = CARTESIAN_POINT ( 'NONE',  ( -93.38350063318468131, -278.0172278784405648, -222.9450911111168239 ) ) ;
#10377 = VERTEX_POINT ( 'NONE', #1730 ) ;
#10378 = CARTESIAN_POINT ( 'NONE',  ( -34.04382328403392677, -297.7591056291649920, -193.3824422723413079 ) ) ;
#10379 = CARTESIAN_POINT ( 'NONE',  ( -75.74301641984335731, -293.4558982481039493, -206.5306123059871481 ) ) ;
#10380 = CARTESIAN_POINT ( 'NONE',  ( 38.02829655723240165, -295.2940243517769545, -281.5773568860684577 ) ) ;
#10381 = CARTESIAN_POINT ( 'NONE',  ( 222.4306832106270804, -135.2391364535880882, -21.50000000000000000 ) ) ;
#10382 = CARTESIAN_POINT ( 'NONE',  ( -107.4954547383039909, -291.4756055206681822, -249.7656581408620013 ) ) ;
#10383 = CARTESIAN_POINT ( 'NONE',  ( 156.9788729827742202, 275.8411434044543284, 16.89623125813446336 ) ) ;
#10385 = ORIENTED_EDGE ( 'NONE', *, *, #40721, .T. ) ;
#10384 = ADVANCED_FACE ( 'NONE', ( #60446 ), #71600, .T. ) ;
#10386 = CARTESIAN_POINT ( 'NONE',  ( 36.22830416734981185, -291.4615720379416643, -252.2569761382982279 ) ) ;
#10387 = AXIS2_PLACEMENT_3D ( 'NONE', #36103, #92447, #6301 ) ;
#10388 = CARTESIAN_POINT ( 'NONE',  ( -33.80656489309921398, -297.7643252171774293, -197.3401806514473549 ) ) ;
#10389 = DIRECTION ( 'NONE',  ( -0.5335274993777934238, 0.8457827187922903889, 0.000000000000000000 ) ) ;
#10390 = CARTESIAN_POINT ( 'NONE',  ( 195.4192251500433031, 26.20723835156640291, 14.74561642346474777 ) ) ;
#10391 = CARTESIAN_POINT ( 'NONE',  ( -97.81081234157554150, -292.6991598215076920, -223.7975759294687919 ) ) ;
#10392 = CARTESIAN_POINT ( 'NONE',  ( -119.3990491898856732, -293.0519495502701943, -270.3937649182068412 ) ) ;
#10393 = CARTESIAN_POINT ( 'NONE',  ( -16.68977181470062732, -288.3195797923462464, -198.3797194067700502 ) ) ;
#10394 = CARTESIAN_POINT ( 'NONE',  ( -4.480570436723880334, -272.4859908324981461, -203.1147001390953903 ) ) ;
#10395 = CARTESIAN_POINT ( 'NONE',  ( 20.09463257291801597, -276.8141380411534556, -223.0073231278088315 ) ) ;
#10396 = CARTESIAN_POINT ( 'NONE',  ( -17.01637942941059478, -290.3963254354550259, -198.6960619842710969 ) ) ;
#10397 = CARTESIAN_POINT ( 'NONE',  ( -11.94606309947037204, -282.2395003475567705, -198.9242012499309453 ) ) ;
#10398 = ORIENTED_EDGE ( 'NONE', *, *, #37113, .T. ) ;
#10399 = CARTESIAN_POINT ( 'NONE',  ( -38.89555298335665867, -282.4207048524811512, -343.4590434138172554 ) ) ;
#10400 = CARTESIAN_POINT ( 'NONE',  ( -112.1797373119256775, -279.4214173614275296, -287.1170334106876680 ) ) ;
#10401 = CARTESIAN_POINT ( 'NONE',  ( -25.44206217947374071, -278.9955218419108860, -194.6880888746761116 ) ) ;
#10402 = CARTESIAN_POINT ( 'NONE',  ( 4.396380910141553855, -58.38232387978199256, -351.6302086872513541 ) ) ;
#10403 = CARTESIAN_POINT ( 'NONE',  ( 36.66199927469088493, -276.7503278752630536, -290.8129213564855036 ) ) ;
#10404 = ADVANCED_FACE ( 'NONE', ( #38164 ), #59038, .T. ) ;
#10405 = APPLICATION_PROTOCOL_DEFINITION ( 'draft international standard', 'automotive_design', 1998, #58995 ) ;
#10406 = CARTESIAN_POINT ( 'NONE',  ( -87.59445373597829132, -274.8859665885781283, -212.8681338081721321 ) ) ;
#10407 = CARTESIAN_POINT ( 'NONE',  ( -53.28691492658256834, -279.7662352645559736, -340.3683826091709079 ) ) ;
#10408 = VERTEX_POINT ( 'NONE', #87885 ) ;
#10409 = ORIENTED_EDGE ( 'NONE', *, *, #92815, .F. ) ;
#10410 = CARTESIAN_POINT ( 'NONE',  ( 208.4306832106271088, 20.44233620800389772, -7.500000000000013323 ) ) ;
#10411 = CARTESIAN_POINT ( 'NONE',  ( -94.33596509774943684, -290.9823965034725006, -316.4683824346556662 ) ) ;
#10412 = CARTESIAN_POINT ( 'NONE',  ( -108.9035566690691326, -291.9836875177282991, -296.0683934744686212 ) ) ;
#10413 = CARTESIAN_POINT ( 'NONE',  ( -98.93210732212988034, -289.3568454957165272, -309.7376898216074892 ) ) ;
#10414 = CARTESIAN_POINT ( 'NONE',  ( -7.361317943236533878, -285.9424251958917580, -199.4475819698151327 ) ) ;
#10415 = CARTESIAN_POINT ( 'NONE',  ( 198.4290158740602976, 26.16953160995604577, 11.14960445189099048 ) ) ;
#10416 = CARTESIAN_POINT ( 'NONE',  ( 21.63709376544842655, -280.5684566432405518, -314.7434893531541888 ) ) ;
#10417 = CARTESIAN_POINT ( 'NONE',  ( 16.92991528933320566, -290.1295590083218485, -321.0867030176503931 ) ) ;
#10418 = CARTESIAN_POINT ( 'NONE',  ( -40.28121171501673814, -281.5696464504039227, -343.9958042750290019 ) ) ;
#10419 = CARTESIAN_POINT ( 'NONE',  ( 33.20329212461374624, -282.5965481485999931, -249.7541398761201208 ) ) ;
#10420 = CARTESIAN_POINT ( 'NONE',  ( 20.40384084099146733, -289.1799449687768515, -320.9602950550949458 ) ) ;
#10421 = CARTESIAN_POINT ( 'NONE',  ( -81.32992359588129716, -279.9282673989548584, -211.9621379610919121 ) ) ;
#10422 = CARTESIAN_POINT ( 'NONE',  ( -84.01221970299478414, -290.2221554334811913, -209.5499630389306844 ) ) ;
#10423 = CARTESIAN_POINT ( 'NONE',  ( -99.22029928472194626, -285.9624415080560311, -224.7192184990594512 ) ) ;
#10424 = CARTESIAN_POINT ( 'NONE',  ( -76.08116222059351230, -286.0417780232569953, -203.8258521546716793 ) ) ;
#10425 = CARTESIAN_POINT ( 'NONE',  ( -107.3913212994303592, -284.4465008875876038, -290.9496140503081278 ) ) ;
#10426 = EDGE_LOOP ( 'NONE', ( #61792, #11771, #8647, #7642 ) ) ;
#10427 = DIRECTION ( 'NONE',  ( 0.000000000000000000, 0.000000000000000000, 1.000000000000000000 ) ) ;
#10428 = CARTESIAN_POINT ( 'NONE',  ( -44.79942596471324379, -293.8192604128157654, -194.9121756299024923 ) ) ;
#10429 = CARTESIAN_POINT ( 'NONE',  ( 34.00902022171862882, -291.8832910336687974, -242.6035284343190028 ) ) ;
#10430 = CARTESIAN_POINT ( 'NONE',  ( 24.17553975138443434, -275.1603718483514740, -310.1917077507918634 ) ) ;
#10431 = CARTESIAN_POINT ( 'NONE',  ( -79.42811998457050038, -294.9531504068605159, -334.7198473830778198 ) ) ;
#10432 = CARTESIAN_POINT ( 'NONE',  ( -106.3531781858590932, -289.3753385092677490, -244.3683360026673768 ) ) ;
#10433 = CARTESIAN_POINT ( 'NONE',  ( 15.01751454587202872, -292.5414745646988308, -322.7445946047343455 ) ) ;
#10434 = CARTESIAN_POINT ( 'NONE',  ( -5.885295437337413560, -293.6802368486648334, -204.0326708483576965 ) ) ;
#10435 = DIRECTION ( 'NONE',  ( -1.000000000000000000, -0.000000000000000000, -0.000000000000000000 ) ) ;
#10436 = CARTESIAN_POINT ( 'NONE',  ( 22.53075550974246255, -290.9314232919520009, -224.8941643023447625 ) ) ;
#10437 = CARTESIAN_POINT ( 'NONE',  ( 25.11433188523751170, -296.1135720362655093, -311.9081734441294884 ) ) ;
#10438 = CARTESIAN_POINT ( 'NONE',  ( -26.42802519558905061, -289.8512577627943188, -342.8298730236060692 ) ) ;
#10439 = CARTESIAN_POINT ( 'NONE',  ( -7.208754686653007226, -278.6387780073622480, -339.4432442664805194 ) ) ;
#10440 = CARTESIAN_POINT ( 'NONE',  ( -101.7713765416022227, -276.7995399529935412, -311.8925316507010166 ) ) ;
#10441 = CARTESIAN_POINT ( 'NONE',  ( -64.85585218110912820, -273.0506747801122742, -198.5396803778954506 ) ) ;
#10442 = CARTESIAN_POINT ( 'NONE',  ( 27.72922961401178910, -279.1472748416293825, -234.2074418495037946 ) ) ;
#10443 = CARTESIAN_POINT ( 'NONE',  ( -56.74025005335258953, -275.6979373405119418, -344.1050640318513274 ) ) ;
#10444 = CARTESIAN_POINT ( 'NONE',  ( -97.59723696607882459, -294.6542228942302017, -312.4385912776602936 ) ) ;
#10445 = CARTESIAN_POINT ( 'NONE',  ( -91.97293552038924247, -275.2725483744221719, -218.9574111575386439 ) ) ;
#10446 = CARTESIAN_POINT ( 'NONE',  ( -39.18261759023302204, -298.8313321062738623, -197.2103693235461321 ) ) ;
#10447 = CIRCLE ( 'NONE', #39229, 1.999999999999988454 ) ;
#10448 = CARTESIAN_POINT ( 'NONE',  ( 210.2502938138737250, 0.01288801604375340581, 7.290233312756248196 ) ) ;
#10450 = CARTESIAN_POINT ( 'NONE',  ( 5.178469112389147533, -274.4783030319850923, -210.9603282420799815 ) ) ;
#10449 = CARTESIAN_POINT ( 'NONE',  ( -45.86531372870712886, -287.1796816661181992, -345.2846993941365099 ) ) ;
#10451 = CARTESIAN_POINT ( 'NONE',  ( 39.60432534630992052, -287.6029507991769378, -274.4229353302731056 ) ) ;
#10452 = CARTESIAN_POINT ( 'NONE',  ( -86.84850476573345190, -275.3659278544479321, -213.7312673841425976 ) ) ;
#10453 = CARTESIAN_POINT ( 'NONE',  ( -110.0870769161513181, -294.3254077254051140, -287.9691065984814600 ) ) ;
#10454 = CARTESIAN_POINT ( 'NONE',  ( -2.974255308287749422, -281.8068451363273539, -339.1000989682818840 ) ) ;
#10455 = CARTESIAN_POINT ( 'NONE',  ( 156.4947056272797852, 20.00000000000000000, 15.00000000000000000 ) ) ;
#10456 = CARTESIAN_POINT ( 'NONE',  ( -74.48243906413325988, -277.5583867571803012, -205.1443982511464981 ) ) ;
#10457 = CARTESIAN_POINT ( 'NONE',  ( 197.3748232817348764, 214.9910457053126720, -12.45182892472558756 ) ) ;
#10458 = CARTESIAN_POINT ( 'NONE',  ( -66.70893448764876155, -290.4535263652925892, -203.0952570144076788 ) ) ;
#10459 = DIRECTION ( 'NONE',  ( 0.000000000000000000, 0.000000000000000000, 1.000000000000000000 ) ) ;
#10460 = DIRECTION ( 'NONE',  ( 0.000000000000000000, 0.000000000000000000, -1.000000000000000000 ) ) ;
#10461 = CARTESIAN_POINT ( 'NONE',  ( -50.00193338202542748, -289.8905829064393629, -196.3846497186790430 ) ) ;
#10462 = CARTESIAN_POINT ( 'NONE',  ( -5.021282101477411608, -276.0057029830579154, -204.1195395975817064 ) ) ;
#10463 = CARTESIAN_POINT ( 'NONE',  ( 30.56188935648144422, -283.4325423727615885, -305.3997941339107456 ) ) ;
#10465 = CARTESIAN_POINT ( 'NONE',  ( -34.84654087315310278, -283.0199734239710097, -343.3308994947895485 ) ) ;
#10464 = CARTESIAN_POINT ( 'NONE',  ( -94.91431266262259214, -271.3044901512987508, -221.4054459890624855 ) ) ;
#10466 = CARTESIAN_POINT ( 'NONE',  ( 3.239869799699233610, -276.0341177301520474, -208.9120267283728651 ) ) ;
#10467 = CARTESIAN_POINT ( 'NONE',  ( 0.6876917415886037999, -275.3762750066214835, -207.8601813420770839 ) ) ;
#10468 = ADVANCED_FACE ( 'NONE', ( #73712 ), #80337, .F. ) ;
#10469 = CARTESIAN_POINT ( 'NONE',  ( -75.71220310470822312, -285.5639878299744510, -334.8628066158308911 ) ) ;
#10470 = ORIENTED_EDGE ( 'NONE', *, *, #87659, .F. ) ;
#10471 = CARTESIAN_POINT ( 'NONE',  ( 204.9739665765744974, 293.8334707905521554, -54.00000000001804068 ) ) ;
#10472 = CARTESIAN_POINT ( 'NONE',  ( -5.799642124202470939, -294.4820825094672045, -340.6042570169652777 ) ) ;
#10473 = CARTESIAN_POINT ( 'NONE',  ( -57.87040969928217038, -287.7657409284143455, -198.5408942880984853 ) ) ;
#10474 = DIRECTION ( 'NONE',  ( 0.000000000000000000, 0.000000000000000000, 1.000000000000000000 ) ) ;
#10475 = CARTESIAN_POINT ( 'NONE',  ( -55.56934967048407970, -283.3380690714490697, -190.3538533559490702 ) ) ;
#10476 = CARTESIAN_POINT ( 'NONE',  ( -59.62796332002544375, -276.5308358882868447, -343.8966963989101941 ) ) ;
#10477 = CARTESIAN_POINT ( 'NONE',  ( -70.53067184166060599, -290.0217210693647303, -201.7686069082039637 ) ) ;
#10478 = CARTESIAN_POINT ( 'NONE',  ( -69.09102002166399359, -287.1469252974607684, -203.8438989350652548 ) ) ;
#10479 = CARTESIAN_POINT ( 'NONE',  ( -40.52725266688558037, -278.8528665413316503, -344.3185070341197047 ) ) ;
#10480 = CARTESIAN_POINT ( 'NONE',  ( -89.49741724719342528, -286.7600217122122217, -214.4466133842082627 ) ) ;
#10481 = CARTESIAN_POINT ( 'NONE',  ( -5.152059720449447155, -284.6287268084413427, -338.1161333162526716 ) ) ;
#10482 = CARTESIAN_POINT ( 'NONE',  ( -17.35585397138957475, -276.9678040294485868, -344.7221693326229683 ) ) ;
#10483 = CARTESIAN_POINT ( 'NONE',  ( -39.96507856654450563, -276.9175473676718866, -347.3294821416055242 ) ) ;
#10484 = CARTESIAN_POINT ( 'NONE',  ( -111.4869238625137342, -298.5651493233611404, -263.1846805494872683 ) ) ;
#10485 = DIRECTION ( 'NONE',  ( 0.000000000000000000, 1.000000000000000000, 0.000000000000000000 ) ) ;
#10486 = CARTESIAN_POINT ( 'NONE',  ( 186.6539576904058890, 293.9636489450775230, 0.000000000000000000 ) ) ;
#10487 = CARTESIAN_POINT ( 'NONE',  ( -107.1377320441797423, -271.1813315516205876, -240.1867042516654465 ) ) ;
#10488 = LINE ( 'NONE', #39356, #16822 ) ;
#10489 = CARTESIAN_POINT ( 'NONE',  ( -71.68865467144316028, -277.0265573997915567, -334.8599193487440857 ) ) ;
#10490 = CARTESIAN_POINT ( 'NONE',  ( 6.992617980718112136, -275.8456764013615725, -207.8262216018322874 ) ) ;
#10491 = CARTESIAN_POINT ( 'NONE',  ( 23.20990409826498535, -281.2434288437601140, -317.5662879070295048 ) ) ;
#10492 = CARTESIAN_POINT ( 'NONE',  ( -10.40172968695477351, -288.1686865617420494, -201.4111167750988329 ) ) ;
#10493 = CARTESIAN_POINT ( 'NONE',  ( -50.33028691975509616, -296.7350564382581979, -345.6076892880706737 ) ) ;
#10494 = CARTESIAN_POINT ( 'NONE',  ( -112.8099822336917981, -297.5883278254459015, -283.7962421834400288 ) ) ;
#10495 = CARTESIAN_POINT ( 'NONE',  ( -0.3725905512409277698, -294.5449658588265720, -205.2823641809736159 ) ) ;
#10496 = CARTESIAN_POINT ( 'NONE',  ( -11.07639805348886242, -278.3949851672785485, -200.2337590440926931 ) ) ;
#10497 = CARTESIAN_POINT ( 'NONE',  ( 35.15739103849399783, -283.2538329804272053, -253.4733714793716501 ) ) ;
#10498 = CARTESIAN_POINT ( 'NONE',  ( -66.10702130942968324, -295.7525589130432877, -201.7034855097575416 ) ) ;
#10499 = CARTESIAN_POINT ( 'NONE',  ( -87.77662108766821802, -285.3428265017375338, -327.5521216856410547 ) ) ;
#10500 = CARTESIAN_POINT ( 'NONE',  ( 35.30436796394098309, -286.3383739074523646, -260.1524026511864918 ) ) ;
#10501 = CARTESIAN_POINT ( 'NONE',  ( 25.01975656489566191, -281.4983696210121025, -315.3763720174604259 ) ) ;
#10502 = CARTESIAN_POINT ( 'NONE',  ( -46.52282107818741252, -155.8297569508557103, -364.8203920681885393 ) ) ;
#10503 = ORIENTED_EDGE ( 'NONE', *, *, #50543, .T. ) ;
#10504 = CARTESIAN_POINT ( 'NONE',  ( 9.047192352787497782, -286.3763368047199265, -213.9682271090025552 ) ) ;
#10505 = VERTEX_POINT ( 'NONE', #52387 ) ;
#10506 = CARTESIAN_POINT ( 'NONE',  ( -105.5030844990899084, -285.1756352417384051, -305.6268853121133020 ) ) ;
#10507 = CARTESIAN_POINT ( 'NONE',  ( 29.10352467592040426, -275.4757806086246319, -239.9548332820023404 ) ) ;
#10508 = CARTESIAN_POINT ( 'NONE',  ( 18.07490898210431851, -285.6194753566368263, -217.3978533250726741 ) ) ;
#10509 = CARTESIAN_POINT ( 'NONE',  ( -88.43328048440179145, -290.2758172184852015, -213.1672116141976119 ) ) ;
#10510 = CARTESIAN_POINT ( 'NONE',  ( 8.396702525093648006, -281.6021369168646515, -208.6442681985528793 ) ) ;
#10511 = CARTESIAN_POINT ( 'NONE',  ( 200.2296996224750387, 68.12454877777268791, -4.413917820073306686 ) ) ;
#10512 = CARTESIAN_POINT ( 'NONE',  ( -70.94685247331746325, -281.1368924751873237, -201.8527134510522103 ) ) ;
#10513 = CARTESIAN_POINT ( 'NONE',  ( 36.96348791680276946, -281.6329323207564244, -250.1993700939111989 ) ) ;
#10514 = CIRCLE ( 'NONE', #72590, 4.500000000000003553 ) ;
#10515 = CARTESIAN_POINT ( 'NONE',  ( -21.33282851196157992, -289.7666405000204009, -200.3683826091710216 ) ) ;
#10516 = CARTESIAN_POINT ( 'NONE',  ( -70.42391949612618873, -196.6322980649380554, -360.5434824908751921 ) ) ;
#10517 = EDGE_LOOP ( 'NONE', ( #40382, #46407, #10652, #28400 ) ) ;
#10518 = CARTESIAN_POINT ( 'NONE',  ( -21.23418448624794408, -278.8453654274079554, -343.4936675195637577 ) ) ;
#10519 = CARTESIAN_POINT ( 'NONE',  ( -64.41477511282899115, -182.3306986604505369, -361.9618145500567152 ) ) ;
#10520 = B_SPLINE_CURVE_WITH_KNOTS ( 'NONE', 3,
 ( #13149, #26404, #41985, #70898, #62881, #6031 ),
 .UNSPECIFIED., .F., .F.,
 ( 4, 2, 4 ),
 ( 5.204170427930421283E-18, 0.0006312149994345400694, 0.001262429998869074935 ),
 .UNSPECIFIED. ) ;
#10521 = VECTOR ( 'NONE', #88710, 1000.000000000000000 ) ;
#10522 = CARTESIAN_POINT ( 'NONE',  ( 27.90858972870336885, -279.0875463347991854, -234.1085805025546733 ) ) ;
#10523 = CARTESIAN_POINT ( 'NONE',  ( -105.8985381827449430, -296.2403504500983331, -244.8409028658976183 ) ) ;
#10524 = CARTESIAN_POINT ( 'NONE',  ( -69.59164127088642715, -291.1465974760457698, -200.4935980539915477 ) ) ;
#10525 = CARTESIAN_POINT ( 'NONE',  ( 9.339199855150265961, -285.8906705383787994, 54.50000000000000711 ) ) ;
#10527 = CARTESIAN_POINT ( 'NONE',  ( 18.39360481804174796, -285.2699266819970489, -221.9874040553980308 ) ) ;
#10526 = CARTESIAN_POINT ( 'NONE',  ( -36.88287069353361147, -296.6325250765249280, -193.9504510854497425 ) ) ;
#10528 = CARTESIAN_POINT ( 'NONE',  ( 33.80620824946854697, -295.1347719039209778, -248.9983186340460293 ) ) ;
#10529 = CARTESIAN_POINT ( 'NONE',  ( 25.36281638439481867, -288.3427149551805542, -232.0285328057815946 ) ) ;
#10530 = ORIENTED_EDGE ( 'NONE', *, *, #79777, .T. ) ;
#10531 = CARTESIAN_POINT ( 'NONE',  ( 37.82904797230479943, -294.2973698966376901, -254.7346436236097134 ) ) ;
#10532 = CARTESIAN_POINT ( 'NONE',  ( -91.70664553050789891, -284.3463132952726937, -319.1901979379171621 ) ) ;
#10533 = CARTESIAN_POINT ( 'NONE',  ( -73.08163471227459240, -296.3844663975170874, -202.5481309824065193 ) ) ;
#10534 = CARTESIAN_POINT ( 'NONE',  ( -34.97564950310230358, -292.8839554507575826, -193.5459080265265470 ) ) ;
#10535 = EDGE_CURVE ( 'NONE', #76692, #61220, #51887, .T. ) ;
#10536 = CARTESIAN_POINT ( 'NONE',  ( -19.40720996155652500, -292.7690958600406361, -195.4873527249994822 ) ) ;
#10537 = CARTESIAN_POINT ( 'NONE',  ( 1.313381584854082629, -288.6866308616935726, -332.2867561485459760 ) ) ;
#10538 = ORIENTED_EDGE ( 'NONE', *, *, #65821, .F. ) ;
#10539 = DIRECTION ( 'NONE',  ( -1.000000000000000000, 0.000000000000000000, 0.000000000000000000 ) ) ;
#10540 = CARTESIAN_POINT ( 'NONE',  ( -82.25767650301071399, -299.3074145657657255, -209.2806694197529112 ) ) ;
#10541 = CARTESIAN_POINT ( 'NONE',  ( -29.86230698156242269, -272.9397709358210591, -194.1242017514943541 ) ) ;
#10542 = ADVANCED_FACE ( 'NONE', ( #9767 ), #88823, .T. ) ;
#10543 = CARTESIAN_POINT ( 'NONE',  ( 33.54825666909618320, -280.8534280356370232, -288.7964247969299549 ) ) ;
#10544 = EDGE_LOOP ( 'NONE', ( #35103, #40798, #57160, #20694 ) ) ;
#10545 = ORIENTED_EDGE ( 'NONE', *, *, #8160, .T. ) ;
#10546 = CARTESIAN_POINT ( 'NONE',  ( -68.99579130527776272, -276.9650046599041389, -340.5007241235339848 ) ) ;
#10547 = CARTESIAN_POINT ( 'NONE',  ( 9.501111249989374841, -297.1288287902126513, -196.6801671452016649 ) ) ;
#10548 = CARTESIAN_POINT ( 'NONE',  ( -59.54220080878624799, -279.2031490689377051, -341.1989839014649419 ) ) ;
#10549 = CARTESIAN_POINT ( 'NONE',  ( 22.49055342951936964, -273.0863415453952712, -226.4183493338155984 ) ) ;
#10550 = CARTESIAN_POINT ( 'NONE',  ( -71.86526864358874889, -298.7902021470626437, -205.5760632716375085 ) ) ;
#10551 = CARTESIAN_POINT ( 'NONE',  ( -77.69354637296220289, -298.5763254413215009, -209.0959065072013630 ) ) ;
#10552 = CARTESIAN_POINT ( 'NONE',  ( -86.95697786558335451, -298.9754459570530116, -212.4576034322300586 ) ) ;
#10553 = CARTESIAN_POINT ( 'NONE',  ( -75.57595720050751709, -271.5652619612874901, -205.3658806995060786 ) ) ;
#10554 = CARTESIAN_POINT ( 'NONE',  ( 35.52670306924603949, -294.2804817817951175, -276.1996523395038139 ) ) ;
#10555 = CARTESIAN_POINT ( 'NONE',  ( -30.73615284537430270, -290.7120126532718700, -197.0689515375237875 ) ) ;
#10556 = DIRECTION ( 'NONE',  ( 0.000000000000000000, 0.000000000000000000, -1.000000000000000000 ) ) ;
#10557 = CARTESIAN_POINT ( 'NONE',  ( -1.335848643648253953, -275.0090871333285918, -202.3676950486506030 ) ) ;
#10558 = CARTESIAN_POINT ( 'NONE',  ( 94.45372940089858105, -300.0800948388032907, -197.3323955020603364 ) ) ;
#10559 = CARTESIAN_POINT ( 'NONE',  ( -0.6269036817332512834, -281.2596968438467684, -337.4976553236531345 ) ) ;
#10560 = B_SPLINE_CURVE_WITH_KNOTS ( 'NONE', 3,
 ( #18411, #25973, #54857, #33088, #4213, #4674, #61527, #69085 ),
 .UNSPECIFIED., .F., .F.,
 ( 4, 2, 2, 4 ),
 ( 2.845565583954363981E-21, 0.001369958260980387805, 0.002054937391470581382, 0.002739916521960775175 ),
 .UNSPECIFIED. ) ;
#10561 = DIRECTION ( 'NONE',  ( 0.000000000000000000, 0.000000000000000000, 1.000000000000000000 ) ) ;
#10562 = CARTESIAN_POINT ( 'NONE',  ( -66.63359273667273897, -282.6430907314793899, -337.4163993105046870 ) ) ;
#10563 = CARTESIAN_POINT ( 'NONE',  ( -33.18618578371622618, -280.9997982578522056, -345.4256567544264271 ) ) ;
#10564 = CARTESIAN_POINT ( 'NONE',  ( -6.042364950175674210, -275.2072546392021195, -336.9762458937328802 ) ) ;
#10565 = CARTESIAN_POINT ( 'NONE',  ( -4.171684523773215858, -282.4895854993828834, -203.0808589391315309 ) ) ;
#10566 = CARTESIAN_POINT ( 'NONE',  ( -43.18343439339132317, -296.0521521680024080, -507.6442049081570076 ) ) ;
#10567 = CARTESIAN_POINT ( 'NONE',  ( 221.8344101925596306, 35.72494958537217968, 7.000000000000000000 ) ) ;
#10568 = CARTESIAN_POINT ( 'NONE',  ( -102.0290388320079131, -271.4844634417097495, -230.0871980611412084 ) ) ;
#10569 = CARTESIAN_POINT ( 'NONE',  ( -108.0043536723064506, -280.2189563623049366, -296.1416942028620269 ) ) ;
#10570 =( REPRESENTATION_RELATIONSHIP ('NONE','NONE', #78428, #49383 ) REPRESENTATION_RELATIONSHIP_WITH_TRANSFORMATION ( #83777 )SHAPE_REPRESENTATION_RELATIONSHIP( ) );
#10571 = CARTESIAN_POINT ( 'NONE',  ( 184.1778392089217107, 3.000000000000000000, 10.00000000000000178 ) ) ;
#10572 = CARTESIAN_POINT ( 'NONE',  ( -75.99974213772705411, -285.4839943146464520, -335.3438004477348500 ) ) ;
#10573 = ORIENTED_EDGE ( 'NONE', *, *, #52296, .F. ) ;
#10574 = CARTESIAN_POINT ( 'NONE',  ( 156.4851178187871312, 15.09609934344103976, -9.999999999996333599 ) ) ;
#10575 = CARTESIAN_POINT ( 'NONE',  ( -64.29831819532192583, -289.7003837382890765, -200.3188087569270976 ) ) ;
#10576 = CARTESIAN_POINT ( 'NONE',  ( 82.13570310075333225, -300.5876282232119365, -197.0894904801451730 ) ) ;
#10577 = CARTESIAN_POINT ( 'NONE',  ( -105.1230614484717307, -295.7226269191929191, -242.2041017807349874 ) ) ;
#10578 = CARTESIAN_POINT ( 'NONE',  ( -101.3813065082240712, -288.1835819321852910, -308.0096444239943594 ) ) ;
#10579 = CARTESIAN_POINT ( 'NONE',  ( -117.0947446405890418, -269.4376451100752661, -283.8482964293340274 ) ) ;
#10580 = CARTESIAN_POINT ( 'NONE',  ( -80.86862163996777042, -295.4611348651387175, -209.2840539585544661 ) ) ;
#10581 = CARTESIAN_POINT ( 'NONE',  ( 32.08928784296128356, -285.6222640009506790, -238.5787440806087432 ) ) ;
#10582 = CARTESIAN_POINT ( 'NONE',  ( 30.75188450773570281, -282.7747022875940388, -241.9058171619225845 ) ) ;
#10583 = CARTESIAN_POINT ( 'NONE',  ( -2.123957662188769024, -280.8322464549225401, -337.6937596318705914 ) ) ;
#10584 = CARTESIAN_POINT ( 'NONE',  ( -53.40852788821273833, -289.2640408804089702, -341.5710684510602846 ) ) ;
#10585 = CARTESIAN_POINT ( 'NONE',  ( 35.14438090138292381, -282.8113116095946111, -257.6669076879501858 ) ) ;
#10586 = CARTESIAN_POINT ( 'NONE',  ( 35.19149507609770922, -282.2241032295702894, -260.4173409782697490 ) ) ;
#10587 = CARTESIAN_POINT ( 'NONE',  ( 21.68736377104704260, -288.8912987164727610, -223.5006587009104919 ) ) ;
#10588 = AXIS2_PLACEMENT_3D ( 'NONE', #73851, #44025, #52995 ) ;
#10589 = CARTESIAN_POINT ( 'NONE',  ( -36.89899258508963698, -298.2242305952832453, -193.3611058027246372 ) ) ;
#10590 = ORIENTED_EDGE ( 'NONE', *, *, #22050, .F. ) ;
#10591 = CARTESIAN_POINT ( 'NONE',  ( -10.34761437073554013, -274.3947278289446672, -198.1911549144437856 ) ) ;
#10593 = CARTESIAN_POINT ( 'NONE',  ( 21.46342811626096392, -294.8979961258236244, -224.3643124161924334 ) ) ;
#10592 = AXIS2_PLACEMENT_3D ( 'NONE', #87106, #35997, #64458 ) ;
#10594 = CARTESIAN_POINT ( 'NONE',  ( 123.4306832106270946, -178.2391364535880882, -4.999999999999990230 ) ) ;
#10595 = CARTESIAN_POINT ( 'NONE',  ( -37.30987171927208124, -279.5519495502701943, -345.3611179825600175 ) ) ;
#10596 = ORIENTED_EDGE ( 'NONE', *, *, #73376, .T. ) ;
#10597 = EDGE_CURVE ( 'NONE', #42154, #35472, #64044, .T. ) ;
#10598 = CARTESIAN_POINT ( 'NONE',  ( 35.80183551150867061, -273.7745680256415426, -287.7384755368569245 ) ) ;
#10599 = ADVANCED_FACE ( 'NONE', ( #40479 ), #65181, .F. ) ;
#10600 = DIRECTION ( 'NONE',  ( 1.000000000000000000, 1.359745199634109878E-15, 0.000000000000000000 ) ) ;
#10601 = CARTESIAN_POINT ( 'NONE',  ( -91.05699994692098187, -295.7042963624351160, -216.3138518182221333 ) ) ;
#10602 = CARTESIAN_POINT ( 'NONE',  ( -65.84525176567159122, -273.0177052169784702, -203.0451450457143210 ) ) ;
#10603 = CARTESIAN_POINT ( 'NONE',  ( -72.97905615242036959, -293.0913354385656930, -205.8003836415110470 ) ) ;
#10604 = CARTESIAN_POINT ( 'NONE',  ( -88.10228824416095961, -292.2620763513778002, -217.5011454341837123 ) ) ;
#10605 = CARTESIAN_POINT ( 'NONE',  ( -32.05120441753491178, -284.7446404507693956, -344.1851294501523739 ) ) ;
#10606 = CARTESIAN_POINT ( 'NONE',  ( -108.9282397320278193, -292.3196627312282203, -243.4899506931130873 ) ) ;
#10607 = CARTESIAN_POINT ( 'NONE',  ( -74.45443149787806192, -292.8842833087218764, -203.4586259248638100 ) ) ;
#10608 = CARTESIAN_POINT ( 'NONE',  ( 32.34616958529813502, -293.6735525414015342, -292.1005020428078751 ) ) ;
#10609 = CARTESIAN_POINT ( 'NONE',  ( 36.94479668947634821, -289.6860340955115589, -280.7755589985422944 ) ) ;
#10610 = CARTESIAN_POINT ( 'NONE',  ( 29.28552040893277919, -281.2168826662700098, -231.7630158530184872 ) ) ;
#10611 = CARTESIAN_POINT ( 'NONE',  ( -89.73160184683830209, -293.8636497118489501, -324.8814314600364241 ) ) ;
#10612 = CARTESIAN_POINT ( 'NONE',  ( -16.14387518094875418, -282.6188849751607677, -344.4410763332583656 ) ) ;
#10613 = CARTESIAN_POINT ( 'NONE',  ( 12.87240676034157083, -278.3275301578902372, -325.6616163387516849 ) ) ;
#10614 = CARTESIAN_POINT ( 'NONE',  ( -101.0710525930141728, -276.1443054044719361, -311.4309735074156151 ) ) ;
#10615 = CARTESIAN_POINT ( 'NONE',  ( 198.5720013812636751, 41.52711472736257292, 11.03083405179678778 ) ) ;
#10616 = CARTESIAN_POINT ( 'NONE',  ( -71.44315577849425836, -283.0230739108393436, -334.9759704882437745 ) ) ;
#10617 = CARTESIAN_POINT ( 'NONE',  ( -9.022245195677088603, -281.6194890971141263, -199.1851586208185267 ) ) ;
#10618 = CARTESIAN_POINT ( 'NONE',  ( 5.059727645143717645, -285.6686197322854355, -206.3060877940217495 ) ) ;
#10619 = CARTESIAN_POINT ( 'NONE',  ( 15.58467417205010186, -294.5732435225760355, -218.5501970754897911 ) ) ;
#10620 = CARTESIAN_POINT ( 'NONE',  ( 38.34547702410463188, -277.2694172178909184, -279.6301473563684112 ) ) ;
#10621 = CARTESIAN_POINT ( 'NONE',  ( -7.895966841277534343, -275.7450120130596929, -199.6915263846346704 ) ) ;
#10622 = CARTESIAN_POINT ( 'NONE',  ( -93.60738808868578076, -277.7259347629495778, -316.8906209122224027 ) ) ;
#10623 = CARTESIAN_POINT ( 'NONE',  ( -71.32223896733360391, -299.6026364329388798, -203.6733865007713575 ) ) ;
#10624 = CARTESIAN_POINT ( 'NONE',  ( 32.69931597076778473, -285.2072911839994163, -243.8654259879708661 ) ) ;
#10625 = CARTESIAN_POINT ( 'NONE',  ( -61.58893174056260023, -295.0253479603252913, -343.4772017382548484 ) ) ;
#10626 = CARTESIAN_POINT ( 'NONE',  ( -111.1420792891184988, -291.9117578233698964, -289.3854632699785725 ) ) ;
#10627 = CARTESIAN_POINT ( 'NONE',  ( 9.055060521613025770, -291.6264290658095319, -213.5364181560101713 ) ) ;
#10628 = ORIENTED_EDGE ( 'NONE', *, *, #83917, .T. ) ;
#10629 = CARTESIAN_POINT ( 'NONE',  ( 4.519237161608626430, -292.3008710849157978, -210.4681249279509530 ) ) ;
#10630 = ORIENTED_EDGE ( 'NONE', *, *, #12020, .T. ) ;
#10631 = CARTESIAN_POINT ( 'NONE',  ( 16.47886361846065029, -289.3888988437019520, -325.0686621205390452 ) ) ;
#10632 = CARTESIAN_POINT ( 'NONE',  ( -105.6124570289506863, -279.5537901636736819, -244.0850950118223182 ) ) ;
#10633 = CARTESIAN_POINT ( 'NONE',  ( -113.6371032447908931, -295.3748110933260591, -278.1395479345970898 ) ) ;
#10634 = CARTESIAN_POINT ( 'NONE',  ( -54.94933603908506825, -286.4828998665522590, -195.5060316898160977 ) ) ;
#10635 = CARTESIAN_POINT ( 'NONE',  ( -2.236336455902808051, -286.8371787043939207, -201.8382845890868680 ) ) ;
#10636 = CARTESIAN_POINT ( 'NONE',  ( -93.43558888736643553, -284.2222558878954146, -317.1111247282262866 ) ) ;
#10637 = CARTESIAN_POINT ( 'NONE',  ( -90.47616956948971279, -230.2765260022941902, -347.7368331188851016 ) ) ;
#10638 = CARTESIAN_POINT ( 'NONE',  ( 187.9667495628914082, 271.0942837926032780, -138.8879291161683511 ) ) ;
#10639 = CARTESIAN_POINT ( 'NONE',  ( 120.7416490522416126, 147.9237423001410434, -260.2612779276005313 ) ) ;
#10640 = CARTESIAN_POINT ( 'NONE',  ( -83.11573335683996788, -276.8943094913005325, -327.4994347394787724 ) ) ;
#10641 = CARTESIAN_POINT ( 'NONE',  ( -21.59999097431463255, -275.7660290891985824, -342.0123831557603467 ) ) ;
#10642 = CARTESIAN_POINT ( 'NONE',  ( -70.69668826749686730, -297.1316070035990720, -201.0287902427111817 ) ) ;
#10643 = CARTESIAN_POINT ( 'NONE',  ( 194.5757784920336064, 275.7176583187329015, -124.3598809796911411 ) ) ;
#10644 = CARTESIAN_POINT ( 'NONE',  ( -99.26056766693801592, -276.6367058874288318, -315.3206028598488615 ) ) ;
#10645 = CARTESIAN_POINT ( 'NONE',  ( -69.95742892865899876, -275.3766284193590081, -203.9217602844356065 ) ) ;
#10646 = EDGE_LOOP ( 'NONE', ( #84596, #37762, #15306, #93441 ) ) ;
#10647 =( BOUNDED_CURVE ( )  B_SPLINE_CURVE ( 3, ( #32312, #10511, #47424, #4355 ),
 .UNSPECIFIED., .F., .F. ) 
 B_SPLINE_CURVE_WITH_KNOTS ( ( 4, 4 ),
 ( 0.000000000000000000, 0.5235987755982978165 ),
 .UNSPECIFIED. ) 
 CURVE ( )  GEOMETRIC_REPRESENTATION_ITEM ( )  RATIONAL_B_SPLINE_CURVE ( ( 1.000000000000000000, 0.9772838841927122822, 0.9772838841927122822, 1.000000000000000000 ) ) 
 REPRESENTATION_ITEM ( '' )  );
#10648 = CARTESIAN_POINT ( 'NONE',  ( -110.4295239542293956, -291.0694758379698328, -268.4664138691078392 ) ) ;
#10649 = CARTESIAN_POINT ( 'NONE',  ( -89.50619830964393486, -298.1424108984377881, -213.8707378199553659 ) ) ;
#10650 = CARTESIAN_POINT ( 'NONE',  ( -70.70802993305116502, -298.1161419401509534, -201.0342477304540125 ) ) ;
#10651 = CARTESIAN_POINT ( 'NONE',  ( 1.571629225388392781, -294.6831277847397814, -332.1846717413249053 ) ) ;
#10652 = ORIENTED_EDGE ( 'NONE', *, *, #81790, .T. ) ;
#10653 =( BOUNDED_CURVE ( )  B_SPLINE_CURVE ( 3, ( #3134, #32014, #7682, #58822 ),
 .UNSPECIFIED., .F., .F. ) 
 B_SPLINE_CURVE_WITH_KNOTS ( ( 4, 4 ),
 ( 4.712388980384683457, 7.853981633974489007 ),
 .UNSPECIFIED. ) 
 CURVE ( )  GEOMETRIC_REPRESENTATION_ITEM ( )  RATIONAL_B_SPLINE_CURVE ( ( 1.000000000000000000, 0.3333333333333292070, 0.3333333333333292070, 1.000000000000000000 ) ) 
 REPRESENTATION_ITEM ( '' )  );
#10654 = CARTESIAN_POINT ( 'NONE',  ( -2.116939386304322657, -278.5096384412079260, -337.2081854660076488 ) ) ;
#10655 = AXIS2_PLACEMENT_3D ( 'NONE', #16797, #39017, #52770 ) ;
#10656 = CARTESIAN_POINT ( 'NONE',  ( -21.74459379324450836, -282.3650317885534946, -345.7020575641483902 ) ) ;
#10657 = CARTESIAN_POINT ( 'NONE',  ( -56.65070393972205665, -278.2483716366264161, -341.0577547131726419 ) ) ;
#10658 = CARTESIAN_POINT ( 'NONE',  ( 34.25385029062328357, -277.6396244676450920, -295.9731916860246770 ) ) ;
#10659 = CARTESIAN_POINT ( 'NONE',  ( -95.74572301409510544, -295.7519254657343026, -225.5706796945248698 ) ) ;
#10660 = CARTESIAN_POINT ( 'NONE',  ( 196.0143093133015384, 73.40565171261609123, -11.99999999999998046 ) ) ;
#10661 = CARTESIAN_POINT ( 'NONE',  ( -87.09398087807991828, -277.9354448429132276, -323.7812505606715945 ) ) ;
#10662 = CARTESIAN_POINT ( 'NONE',  ( 11.67480567098142608, -275.5152017053350733, -211.1181655909082338 ) ) ;
#10663 = CARTESIAN_POINT ( 'NONE',  ( 12.08440007273762618, -287.0660263978285229, -328.7593961284276247 ) ) ;
#10664 = EDGE_CURVE ( 'NONE', #76475, #64288, #20217, .T. ) ;
#10665 = CARTESIAN_POINT ( 'NONE',  ( -31.44343004379908990, -276.1267746473257603, -195.5804676336160810 ) ) ;
#10666 = CARTESIAN_POINT ( 'NONE',  ( 19.42718347035934201, -274.8267114237044666, -321.5265647942315468 ) ) ;
#10667 = CARTESIAN_POINT ( 'NONE',  ( 196.5845095011719081, 20.48014462998423824, -13.01238430412327673 ) ) ;
#10668 = CARTESIAN_POINT ( 'NONE',  ( -23.76521645923465798, -288.0715237638189592, -342.3036859560483549 ) ) ;
#10669 = CARTESIAN_POINT ( 'NONE',  ( -65.83187507613813239, -285.0376952101303232, -198.9213382334257290 ) ) ;
#10670 = CARTESIAN_POINT ( 'NONE',  ( 34.63034627907831009, -280.0173169810651075, -287.6776047824728835 ) ) ;
#10672 = CARTESIAN_POINT ( 'NONE',  ( -111.0343867755999412, -282.7681059504021164, -259.8396098831517520 ) ) ;
#10671 = CARTESIAN_POINT ( 'NONE',  ( 19.79816039281242368, -280.7779916982752866, -316.7535019160187630 ) ) ;
#10673 = CARTESIAN_POINT ( 'NONE',  ( -97.50034916441894950, -291.9405220406471813, -315.1698539241114077 ) ) ;
#10674 = CARTESIAN_POINT ( 'NONE',  ( -93.01787794354686412, -279.0799752551828874, -318.1867777227880651 ) ) ;
#10675 = CARTESIAN_POINT ( 'NONE',  ( -112.7898535754452070, -271.0197564485751514, -296.3298950837670986 ) ) ;
#10676 = CARTESIAN_POINT ( 'NONE',  ( 38.72911144306201692, -280.0185624848528505, -275.6261384257576879 ) ) ;
#10677 = CARTESIAN_POINT ( 'NONE',  ( 37.25082834313838021, -295.6587166317874562, -278.6479071567125629 ) ) ;
#10678 = CARTESIAN_POINT ( 'NONE',  ( -42.34070906176545179, -278.2297853337713605, -194.5390636451637363 ) ) ;
#10679 = CARTESIAN_POINT ( 'NONE',  ( -70.89690419347613215, -285.4939989572815193, -337.6223751132505981 ) ) ;
#10680 = CARTESIAN_POINT ( 'NONE',  ( 197.7360402925001779, 68.71846123420905883, 9.407289490885741401 ) ) ;
#10681 = CARTESIAN_POINT ( 'NONE',  ( -112.8118093759850495, -292.4253476089225501, -274.0457896863701990 ) ) ;
#10682 = CARTESIAN_POINT ( 'NONE',  ( 7.458099028678516262, -285.8428295890606137, -207.8685272506551485 ) ) ;
#10683 = CARTESIAN_POINT ( 'NONE',  ( -36.17324510314739427, -290.4668764990971113, -196.5577527448681394 ) ) ;
#10684 = CARTESIAN_POINT ( 'NONE',  ( -48.18343439336744183, -267.6629864561588761, -434.3825974374845487 ) ) ;
#10685 = CARTESIAN_POINT ( 'NONE',  ( 21.21980197018436343, -274.8568333750899342, -314.7660045527009061 ) ) ;
#10686 = CARTESIAN_POINT ( 'NONE',  ( -67.82370301165823889, -293.5960963828719628, -338.0634103063202360 ) ) ;
#10687 = FILL_AREA_STYLE ('',( #67545 ) ) ;
#10688 = CARTESIAN_POINT ( 'NONE',  ( 196.8803347170859865, 42.36571313990103960, 12.49999999999999289 ) ) ;
#10689 = CARTESIAN_POINT ( 'NONE',  ( 14.97700674828470291, -291.2534639919134634, -214.7416269469087240 ) ) ;
#10690 = CARTESIAN_POINT ( 'NONE',  ( -109.7174840115487626, -286.3405579096062183, -255.9324546953190520 ) ) ;
#10691 = CARTESIAN_POINT ( 'NONE',  ( -15.26831779957030832, -287.0102001816077859, -343.1261007486804147 ) ) ;
#10692 = CARTESIAN_POINT ( 'NONE',  ( -37.29860563804250972, -287.4779394910289056, -196.7593603668306343 ) ) ;
#10693 = DIRECTION ( 'NONE',  ( -1.000000000000000000, 0.000000000000000000, 0.000000000000000000 ) ) ;
#10694 = CARTESIAN_POINT ( 'NONE',  ( 35.84160461819834609, -288.3278303625476724, -268.2977278835032280 ) ) ;
#10695 = CARTESIAN_POINT ( 'NONE',  ( 7.844060603488878236, -294.6453547245783398, -209.9913339980942339 ) ) ;
#10696 = DIRECTION ( 'NONE',  ( 0.000000000000000000, 1.000000000000000000, 0.000000000000000000 ) ) ;
#10697 = CARTESIAN_POINT ( 'NONE',  ( -109.3029134487697434, -276.3348439394575280, -293.5709773389618817 ) ) ;
#10698 = CARTESIAN_POINT ( 'NONE',  ( -28.59922168061781278, -277.2775703214923055, -346.8954827347368450 ) ) ;
#10699 = CARTESIAN_POINT ( 'NONE',  ( 0.9910615056859225502, -290.6389232828684612, -205.1866954115612600 ) ) ;
#10700 = CARTESIAN_POINT ( 'NONE',  ( -112.7175445974691428, -278.7496880259101886, -254.5659702265035094 ) ) ;
#10701 = CARTESIAN_POINT ( 'NONE',  ( -50.26287168460399357, -299.8662985259423408, -196.8431601382698091 ) ) ;
#10702 = CARTESIAN_POINT ( 'NONE',  ( -8.706848857124272811, -284.4266351327742086, -201.0287989254448746 ) ) ;
#10703 = CARTESIAN_POINT ( 'NONE',  ( -113.5000000000000568, -212.3147208684173677, -516.1047766808072765 ) ) ;
#10704 = CARTESIAN_POINT ( 'NONE',  ( -111.6280718298464620, -276.6883823284501318, -270.6190943611029525 ) ) ;
#10705 = EDGE_CURVE ( 'NONE', #41724, #72750, #59560, .T. ) ;
#10706 = CARTESIAN_POINT ( 'NONE',  ( 10.20451192151873165, -280.3967150932363666, -328.4313936975426600 ) ) ;
#10707 = EDGE_CURVE ( 'NONE', #15284, #27807, #90669, .T. ) ;
#10708 = DIRECTION ( 'NONE',  ( -0.000000000000000000, -1.000000000000000000, 0.000000000000000000 ) ) ;
#10709 = CARTESIAN_POINT ( 'NONE',  ( 0.6845688316304823218, -275.0350042511108200, -336.5777569629277082 ) ) ;
#10710 = CARTESIAN_POINT ( 'NONE',  ( -108.6354617769533917, -297.8277384674277641, -289.0632322392954165 ) ) ;
#10711 = CARTESIAN_POINT ( 'NONE',  ( -30.25718915281167298, -281.8848392025566341, -346.7240816089750410 ) ) ;
#10712 = CARTESIAN_POINT ( 'NONE',  ( -88.29804044472858493, -298.2585208316266403, -217.6893557660566216 ) ) ;
#10713 = CARTESIAN_POINT ( 'NONE',  ( -65.37699570403054850, -299.0085430517990517, -199.1193739938315161 ) ) ;
#10714 = CARTESIAN_POINT ( 'NONE',  ( -31.33374103302742597, -273.7968042423041197, -197.5748986713184649 ) ) ;
#10715 = CARTESIAN_POINT ( 'NONE',  ( 10.09463929519419700, -294.7057653977937548, -212.2007941678915870 ) ) ;
#10716 = CARTESIAN_POINT ( 'NONE',  ( 37.14495329348281416, -287.9630790946376919, -289.8736387469426745 ) ) ;
#10717 = CARTESIAN_POINT ( 'NONE',  ( -38.12988750001531457, -278.1221983212080318, -194.8052250104931886 ) ) ;
#10718 = CARTESIAN_POINT ( 'NONE',  ( -114.3687848332295260, -290.4105918263243211, -268.3525939512876448 ) ) ;
#10719 = CARTESIAN_POINT ( 'NONE',  ( 35.23097408159468102, -286.4767709902948809, -260.1609494522082286 ) ) ;
#10720 = CARTESIAN_POINT ( 'NONE',  ( -85.21628041027933875, -289.3912532301557121, -212.5613459844066426 ) ) ;
#10721 = ORIENTED_EDGE ( 'NONE', *, *, #81598, .T. ) ;
#10722 = CARTESIAN_POINT ( 'NONE',  ( 198.4603912096053193, 279.4542985770845576, -127.2015713121144529 ) ) ;
#10723 = CARTESIAN_POINT ( 'NONE',  ( -29.17246090628071897, -288.4534831264834907, -342.9645061414113911 ) ) ;
#10724 = CARTESIAN_POINT ( 'NONE',  ( 139.1539576904058606, 249.5000000000000568, 12.50000000000000000 ) ) ;
#10725 = AXIS2_PLACEMENT_3D ( 'NONE', #88163, #37067, #632 ) ;
#10726 = CARTESIAN_POINT ( 'NONE',  ( -91.74471522434500059, -286.2405678004562901, -216.2027191778190343 ) ) ;
#10727 = CARTESIAN_POINT ( 'NONE',  ( -8.588195852930263996, -291.4781644400528080, -199.1848845544936637 ) ) ;
#10728 = CARTESIAN_POINT ( 'NONE',  ( -7.865464708224273238, -282.0320895933588758, -200.0789643550781136 ) ) ;
#10729 = CARTESIAN_POINT ( 'NONE',  ( -7.743340382072014805, -281.7471812536335847, -199.7973837385956983 ) ) ;
#10730 = CARTESIAN_POINT ( 'NONE',  ( -95.11774214064784871, -283.7570283898784282, -315.0013508448441826 ) ) ;
#10731 = CARTESIAN_POINT ( 'NONE',  ( 1.940068575895329328, -278.5270857289665400, -334.3122409987219044 ) ) ;
#10732 = CARTESIAN_POINT ( 'NONE',  ( -82.97057633259714748, -297.4472980442525341, -208.2706356750579744 ) ) ;
#10733 = CARTESIAN_POINT ( 'NONE',  ( -92.39863832334661709, -274.5581645179314023, -221.6787080653439546 ) ) ;
#10734 = CARTESIAN_POINT ( 'NONE',  ( 32.37336996393432997, -291.2238401860857380, -243.6842403021568089 ) ) ;
#10735 = CARTESIAN_POINT ( 'NONE',  ( -94.91467594722058720, -271.9860455555678982, -224.8365865566790944 ) ) ;
#10736 = ORIENTED_EDGE ( 'NONE', *, *, #18738, .T. ) ;
#10737 = CARTESIAN_POINT ( 'NONE',  ( 165.2494399300530290, 8.542400036368780647, 9.000000000000001776 ) ) ;
#10738 = CARTESIAN_POINT ( 'NONE',  ( -109.4291553198203815, -286.7126552196176590, -251.7946696248425837 ) ) ;
#10739 = CARTESIAN_POINT ( 'NONE',  ( 0.4004077071593539761, -295.6412293317794706, -337.1371981409969862 ) ) ;
#10740 = CARTESIAN_POINT ( 'NONE',  ( -103.5813378733372048, -285.6219723232832166, -239.3185583255447284 ) ) ;
#10741 = CARTESIAN_POINT ( 'NONE',  ( -45.63614427752890634, -276.2134521006823888, -346.7292975434579603 ) ) ;
#10742 = CARTESIAN_POINT ( 'NONE',  ( -11.19572241598899431, -293.0353898945530204, -197.9884879881219604 ) ) ;
#10743 = CARTESIAN_POINT ( 'NONE',  ( 37.34335100084359738, -285.5287685181241386, -257.5391240864649376 ) ) ;
#10744 = CARTESIAN_POINT ( 'NONE',  ( 28.03215758393609036, -293.3524563055941030, -229.6155661232588443 ) ) ;
#10745 = CARTESIAN_POINT ( 'NONE',  ( -50.75118453917053785, -289.5613363637224893, -342.1921481868440083 ) ) ;
#10746 = CARTESIAN_POINT ( 'NONE',  ( 73.43068321062709458, -178.2391364535880882, -4.999999999999990230 ) ) ;
#10747 = CARTESIAN_POINT ( 'NONE',  ( 153.7799452197002665, 19.44319250842783120, -11.58598955890918702 ) ) ;
#10748 = CARTESIAN_POINT ( 'NONE',  ( -11.96379597270533246, -92.71834851594391580, -356.3861524803674570 ) ) ;
#10749 = CARTESIAN_POINT ( 'NONE',  ( -100.8314115110139966, -285.5089738210984933, -312.7851289677623186 ) ) ;
#10750 = CARTESIAN_POINT ( 'NONE',  ( -55.56934967048407970, -271.3380690714491266, -190.3538533559490702 ) ) ;
#10751 = EDGE_LOOP ( 'NONE', ( #69305, #43017 ) ) ;
#10752 = CARTESIAN_POINT ( 'NONE',  ( -2.292921609286411311, -281.4971299140666474, -334.7634250203108763 ) ) ;
#10753 = CARTESIAN_POINT ( 'NONE',  ( -103.3912703137021083, -278.7357302904979974, -230.7201766575317095 ) ) ;
#10754 = CARTESIAN_POINT ( 'NONE',  ( -27.33789394480205104, -282.1795958632827137, -196.1469801832075461 ) ) ;
#10755 = CARTESIAN_POINT ( 'NONE',  ( 204.5909795363367891, 292.7457261787433254, -68.41955665847963530 ) ) ;
#10756 = CARTESIAN_POINT ( 'NONE',  ( 6.571430675641973806, -281.0432031440411151, -332.9577466885220360 ) ) ;
#10757 = CARTESIAN_POINT ( 'NONE',  ( 3.364626072031145831, -284.6224133318508507, -207.7924212691952448 ) ) ;
#10758 = CARTESIAN_POINT ( 'NONE',  ( -70.30993356764764712, -299.3837306600277657, -201.8989415500608686 ) ) ;
#10759 = CARTESIAN_POINT ( 'NONE',  ( -84.51305674767031917, -296.2144103521828242, -326.2204732505211950 ) ) ;
#10760 = ORIENTED_EDGE ( 'NONE', *, *, #93562, .T. ) ;
#10761 = CARTESIAN_POINT ( 'NONE',  ( 21.39797931591046520, -291.6209156172562302, -226.1921974834140769 ) ) ;
#10762 = CARTESIAN_POINT ( 'NONE',  ( -35.70535089044972921, -277.6835718867363880, -347.2548793080964060 ) ) ;
#10763 = CARTESIAN_POINT ( 'NONE',  ( -34.04067943773179650, -274.0948255241699485, -197.4357913641492530 ) ) ;
#10764 = CARTESIAN_POINT ( 'NONE',  ( 25.08332321250857788, -273.8797677761762088, -225.7896970097445717 ) ) ;
#10765 = DIRECTION ( 'NONE',  ( 0.000000000000000000, -0.000000000000000000, 1.000000000000000000 ) ) ;
#10766 = CARTESIAN_POINT ( 'NONE',  ( 20.52236573926490948, -272.8935817134516242, -222.6259801913265903 ) ) ;
#10767 = CARTESIAN_POINT ( 'NONE',  ( -53.14948574445699592, -296.6761351236754081, -345.1729843435741145 ) ) ;
#10768 = DIRECTION ( 'NONE',  ( 0.000000000000000000, 1.000000000000000000, -0.000000000000000000 ) ) ;
#10769 = CARTESIAN_POINT ( 'NONE',  ( 198.8852758280538353, 66.55360856415096293, 4.692040283685088298 ) ) ;
#10770 = CARTESIAN_POINT ( 'NONE',  ( -100.6612366153629949, -285.1269098186397173, -307.3051617790441696 ) ) ;
#10771 = CARTESIAN_POINT ( 'NONE',  ( -13.71544771838811272, -284.5097588080453193, -342.5814351326961855 ) ) ;
#10772 = CARTESIAN_POINT ( 'NONE',  ( -90.82168271424853856, -283.1850622910399125, -320.1986954802123364 ) ) ;
#10773 = CARTESIAN_POINT ( 'NONE',  ( 3.560745142417650388, -274.8916413858188434, -331.7893719442473639 ) ) ;
#10774 = CARTESIAN_POINT ( 'NONE',  ( 19.45443789176212590, -284.0804687698538373, -318.1832037913939075 ) ) ;
#10775 = CARTESIAN_POINT ( 'NONE',  ( -74.37831570381685253, -276.0341931432435558, -334.0713750799314994 ) ) ;
#10776 = CARTESIAN_POINT ( 'NONE',  ( 5.345624557889809836, -275.7244538737770085, -210.6995728644445478 ) ) ;
#10777 = PLANE ( 'NONE',  #80412 ) ;
#10778 = CARTESIAN_POINT ( 'NONE',  ( -88.83083171737196437, -280.1532866199092950, -213.3257942941159797 ) ) ;
#10779 = ORIENTED_EDGE ( 'NONE', *, *, #70232, .F. ) ;
#10780 = EDGE_CURVE ( 'NONE', #45114, #88143, #68943, .T. ) ;
#10781 = CARTESIAN_POINT ( 'NONE',  ( 196.5975808051811669, 18.84406744235270281, 11.77299963048721843 ) ) ;
#10782 = CARTESIAN_POINT ( 'NONE',  ( -109.9178383830745247, -286.1346626059899450, -292.1549054862393291 ) ) ;
#10783 = CARTESIAN_POINT ( 'NONE',  ( -55.85402052730736244, -294.4936941070247371, -341.1942362067428576 ) ) ;
#10784 = CARTESIAN_POINT ( 'NONE',  ( -106.4255897000815310, -289.4650977865974824, -304.2568610767687574 ) ) ;
#10785 = CARTESIAN_POINT ( 'NONE',  ( 36.12742990191152614, -285.9085694237666644, -279.3199653169455132 ) ) ;
#10787 = CARTESIAN_POINT ( 'NONE',  ( -55.23595138817798045, -290.0586605688069994, -198.5435032715879800 ) ) ;
#10786 = CARTESIAN_POINT ( 'NONE',  ( 31.53244297848572941, -285.7820867721393938, -244.2994724476738213 ) ) ;
#10788 = CARTESIAN_POINT ( 'NONE',  ( -70.37998880068430196, -284.7027265713878137, -335.9160135341392106 ) ) ;
#10789 = CARTESIAN_POINT ( 'NONE',  ( -23.33797735764125747, -274.8730716069424602, -344.0949378249958954 ) ) ;
#10790 = CARTESIAN_POINT ( 'NONE',  ( -26.28101928264467801, -287.3134790043345106, -345.7541001039717230 ) ) ;
#10791 = CARTESIAN_POINT ( 'NONE',  ( -4.391616713646087078, -288.4865236114843583, -202.9726973185919405 ) ) ;
#10792 = CARTESIAN_POINT ( 'NONE',  ( 37.16158397909956079, -285.4243330105232985, -260.3967272066142300 ) ) ;
#10793 = VECTOR ( 'NONE', #60490, 1000.000000000000000 ) ;
#10794 = CARTESIAN_POINT ( 'NONE',  ( -21.32511947821312503, -283.7830491607134604, -341.8757210210810058 ) ) ;
#10795 = CARTESIAN_POINT ( 'NONE',  ( -36.09117268585716687, -291.0366967902178317, -345.5301837841675479 ) ) ;
#10796 = FACE_OUTER_BOUND ( 'NONE', #914, .T. ) ;
#10797 = DIRECTION ( 'NONE',  ( -0.8786741093294601068, 0.000000000000000000, 0.4774220455677345987 ) ) ;
#10798 = CARTESIAN_POINT ( 'NONE',  ( -110.5669710796004352, -298.2340350577171648, -289.0512529991289625 ) ) ;
#10799 = CARTESIAN_POINT ( 'NONE',  ( -73.06037851496463986, -277.5785202567057581, -204.4128301731372801 ) ) ;
#10800 = CARTESIAN_POINT ( 'NONE',  ( 36.13556649406574905, -292.4664911062952228, -247.8833487367799080 ) ) ;
#10801 = CARTESIAN_POINT ( 'NONE',  ( -99.10605657217521980, -295.5068704226681007, -229.8755504850865066 ) ) ;
#10802 = CARTESIAN_POINT ( 'NONE',  ( 36.05760788783123871, -280.2856208235211852, -274.0739416475793746 ) ) ;
#10803 = CARTESIAN_POINT ( 'NONE',  ( -27.06770729667313091, -272.2634707912317253, -196.5816123494329020 ) ) ;
#10804 = CARTESIAN_POINT ( 'NONE',  ( -12.82807071576416291, -296.0420645993426660, -339.6991220518505088 ) ) ;
#10805 = CARTESIAN_POINT ( 'NONE',  ( 207.9699384896711933, 0.04196010845019407243, 7.500000000000011546 ) ) ;
#10806 = CARTESIAN_POINT ( 'NONE',  ( -36.88240502880744032, -296.5376888537812761, -194.0545626491387168 ) ) ;
#10807 = CARTESIAN_POINT ( 'NONE',  ( 27.23279826132012005, -292.3239484210758405, -310.5112463240487841 ) ) ;
#10808 = CARTESIAN_POINT ( 'NONE',  ( -19.95037179710934794, -293.7052263745741243, -198.8037682244255393 ) ) ;
#10809 = EDGE_CURVE ( 'NONE', #14834, #31737, #27800, .T. ) ;
#10810 = CARTESIAN_POINT ( 'NONE',  ( 29.33919985515026596, -282.8906705383787994, 74.50000000000001421 ) ) ;
#10811 = CARTESIAN_POINT ( 'NONE',  ( 29.64199254337842859, -294.7499597974837684, -299.7853706077844436 ) ) ;
#10812 = DIRECTION ( 'NONE',  ( -0.000000000000000000, -1.000000000000000000, -0.000000000000000000 ) ) ;
#10814 = CARTESIAN_POINT ( 'NONE',  ( 22.93299158719334230, -294.1262432090257448, -311.6315678334925678 ) ) ;
#10813 = CARTESIAN_POINT ( 'NONE',  ( -13.95681954484038023, -280.7703279347120997, -341.9959849197629183 ) ) ;
#10815 = CARTESIAN_POINT ( 'NONE',  ( 4.545697659568949334, -282.5040189849777903, -335.0340880772603782 ) ) ;
#10816 = CARTESIAN_POINT ( 'NONE',  ( -24.54127771001219571, -282.5599228706585677, -346.3223557989367123 ) ) ;
#10817 = CARTESIAN_POINT ( 'NONE',  ( -108.3018575485358355, -288.8598716072951902, -246.5980271723541080 ) ) ;
#10818 = EDGE_CURVE ( 'NONE', #71850, #19571, #80687, .T. ) ;
#10819 = LINE ( 'NONE', #17941, #18494 ) ;
#10820 = CARTESIAN_POINT ( 'NONE',  ( 0.5074842209121356307, -281.0371973676857920, -336.6343954390261501 ) ) ;
#10821 = CARTESIAN_POINT ( 'NONE',  ( 10.02618436395603574, -287.3373294296103495, -330.7426462517533992 ) ) ;
#10822 = DIRECTION ( 'NONE',  ( -0.000000000000000000, -0.000000000000000000, -1.000000000000000000 ) ) ;
#10823 = CARTESIAN_POINT ( 'NONE',  ( -93.68005681340099500, -297.4819076684323704, -318.0506995621724400 ) ) ;
#10824 = CARTESIAN_POINT ( 'NONE',  ( -2.973746193010138761, -278.0322934168884217, -338.6211980143785354 ) ) ;
#10825 = CARTESIAN_POINT ( 'NONE',  ( -96.42031208133099085, -278.8193177483025238, -227.4448611967359000 ) ) ;
#10826 = CARTESIAN_POINT ( 'NONE',  ( -0.8057297394032891802, -292.6904119392962116, -202.5811587595218839 ) ) ;
#10827 = CARTESIAN_POINT ( 'NONE',  ( -107.9659192529368994, -282.2838443460601070, -297.3684241014060490 ) ) ;
#10828 = CARTESIAN_POINT ( 'NONE',  ( -100.4012304306613430, -280.0042594209836011, -311.0575154519202670 ) ) ;
#10829 = CARTESIAN_POINT ( 'NONE',  ( 35.53072565946914096, -292.5086950613564341, -262.5888175399512647 ) ) ;
#10830 = CARTESIAN_POINT ( 'NONE',  ( -92.18247048047500414, -295.2687883225282803, -219.1239768872219713 ) ) ;
#10831 = VERTEX_POINT ( 'NONE', #3603 ) ;
#10832 = CARTESIAN_POINT ( 'NONE',  ( 197.3507970371305476, 24.88295298518901078, 12.40598166297186111 ) ) ;
#10833 = CARTESIAN_POINT ( 'NONE',  ( 19.73791417178628649, -293.7036940799531521, -315.9870467865972046 ) ) ;
#10834 = DIRECTION ( 'NONE',  ( -0.000000000000000000, -1.000000000000000000, -0.000000000000000000 ) ) ;
#10835 = CARTESIAN_POINT ( 'NONE',  ( -21.33282851196157992, -283.7666405000204009, -200.3683826091710216 ) ) ;
#10836 = CARTESIAN_POINT ( 'NONE',  ( -30.49857286833661973, -297.1946158561257221, -193.5974729951946927 ) ) ;
#10837 = CARTESIAN_POINT ( 'NONE',  ( 29.69134896089387965, -288.3853977817511236, -233.3748410405109723 ) ) ;
#10838 = CARTESIAN_POINT ( 'NONE',  ( 33.70059731441377693, -287.6070069351031293, -287.1537347717867874 ) ) ;
#10839 = CARTESIAN_POINT ( 'NONE',  ( -109.7206254024223284, -279.8903384900612537, -284.2840710866177005 ) ) ;
#10840 = CARTESIAN_POINT ( 'NONE',  ( -44.69171579865019339, -299.7181538927221709, -196.6625565816640631 ) ) ;
#10841 = CARTESIAN_POINT ( 'NONE',  ( -106.6441851294882071, -277.0254538375502875, -294.6875665123658337 ) ) ;
#10842 = VERTEX_POINT ( 'NONE', #76510 ) ;
#10843 = CARTESIAN_POINT ( 'NONE',  ( -35.82440477963562842, -297.7373833247249877, -193.3823448134014029 ) ) ;
#10844 = CARTESIAN_POINT ( 'NONE',  ( -95.20855611956925202, -291.8227431082970611, -317.1878323606499634 ) ) ;
#10845 = CARTESIAN_POINT ( 'NONE',  ( 19.76548821246756660, -294.4617080423584525, -219.8913421643067636 ) ) ;
#10846 = CARTESIAN_POINT ( 'NONE',  ( -113.7095423085087020, -274.0181020978040465, -270.3797830366729045 ) ) ;
#10847 = CARTESIAN_POINT ( 'NONE',  ( -109.0370756374908154, -291.0147268003102567, -284.6962616743735452 ) ) ;
#10848 = CARTESIAN_POINT ( 'NONE',  ( -48.18343439339133027, -249.2485278041818901, -457.7706553364274100 ) ) ;
#10849 = CARTESIAN_POINT ( 'NONE',  ( -47.55307952463697063, -290.0633954504446592, -195.2346694022549514 ) ) ;
#10850 = CARTESIAN_POINT ( 'NONE',  ( -23.36885445191075661, -298.5558941747436847, -193.3814952637580404 ) ) ;
#10852 = CARTESIAN_POINT ( 'NONE',  ( -37.14529423159790866, -297.7214037756789367, -197.3371356321057419 ) ) ;
#10851 = AXIS2_PLACEMENT_3D ( 'NONE', #55757, #77528, #84610 ) ;
#10853 = DIRECTION ( 'NONE',  ( -1.000000000000000000, -0.000000000000000000, -0.000000000000000000 ) ) ;
#10854 = VECTOR ( 'NONE', #83352, 1000.000000000000000 ) ;
#10855 = CARTESIAN_POINT ( 'NONE',  ( 196.4767969875140352, 25.16014212029416086, 13.66798976973107749 ) ) ;
#10856 = CARTESIAN_POINT ( 'NONE',  ( -107.0896973209595302, -291.6722254895928472, -301.4413591983838501 ) ) ;
#10857 = CARTESIAN_POINT ( 'NONE',  ( 13.84574458161073096, -296.9090924074130839, -334.4957818155094174 ) ) ;
#10858 = CARTESIAN_POINT ( 'NONE',  ( -97.24852301069863358, -287.1663516274887229, -225.5147022773129493 ) ) ;
#10859 = CARTESIAN_POINT ( 'NONE',  ( 31.88014990409208949, -273.1786910828441250, -241.7931953196790289 ) ) ;
#10860 = CARTESIAN_POINT ( 'NONE',  ( -88.33724893539921652, -275.2516448583933766, -216.0616695809800092 ) ) ;
#10862 = CARTESIAN_POINT ( 'NONE',  ( 21.33273617967000746, -290.9985811533958326, -224.5297248194005135 ) ) ;
#10861 = CIRCLE ( 'NONE', #1751, 4.999999999999990230 ) ;
#10863 = CARTESIAN_POINT ( 'NONE',  ( -38.50189744499982680, -278.9269643535832870, -346.1170380564475408 ) ) ;
#10864 = CARTESIAN_POINT ( 'NONE',  ( -65.36243024302865479, -282.7769334377372275, -337.8931141727234149 ) ) ;
#10865 = CARTESIAN_POINT ( 'NONE',  ( -86.88498033598381198, -278.8022031872486650, -328.9707981743637788 ) ) ;
#10866 = CARTESIAN_POINT ( 'NONE',  ( -5.097092581668983158, -279.2621815445925222, -200.8751913184327123 ) ) ;
#10867 = CARTESIAN_POINT ( 'NONE',  ( -104.0266749948802669, -253.6705548287846455, -324.5544463287839108 ) ) ;
#10868 = CARTESIAN_POINT ( 'NONE',  ( 21.66229184770098115, -275.8308804817950772, -221.2556280171031347 ) ) ;
#10869 = SHAPE_DEFINITION_REPRESENTATION ( #16322, #67633 ) ;
#10870 = CARTESIAN_POINT ( 'NONE',  ( -68.57811553201872812, -275.1692114448493953, -200.7264935143020068 ) ) ;
#10871 = CARTESIAN_POINT ( 'NONE',  ( -37.37352853689063181, -276.5519495502701375, -200.3611179825600459 ) ) ;
#10872 = VERTEX_POINT ( 'NONE', #68000 ) ;
#10873 = ORIENTED_EDGE ( 'NONE', *, *, #70157, .T. ) ;
#10874 = CARTESIAN_POINT ( 'NONE',  ( 155.0193446949349152, 20.65816215000725720, -12.95286603764679256 ) ) ;
#10875 = CARTESIAN_POINT ( 'NONE',  ( -34.55252550378722987, -290.0960972906104871, -343.6669433406570988 ) ) ;
#10876 = CARTESIAN_POINT ( 'NONE',  ( 38.68889953193243514, -289.3268948880912603, -271.5132555848437050 ) ) ;
#10877 = CARTESIAN_POINT ( 'NONE',  ( -103.6452925671211034, -290.3157169835753848, -239.5759543886024687 ) ) ;
#10878 = CARTESIAN_POINT ( 'NONE',  ( 27.08965273544284003, -286.5069571964024817, -228.3120077498088847 ) ) ;
#10879 = CARTESIAN_POINT ( 'NONE',  ( 200.4644824113734387, 214.9910457053126720, -2.942835885954282471 ) ) ;
#10880 = CARTESIAN_POINT ( 'NONE',  ( 36.36388678617412040, -280.0007123266805706, -274.0929902922406427 ) ) ;
#10881 = CARTESIAN_POINT ( 'NONE',  ( 8.765337633554176833, -290.2726655128453785, -328.5419270717350742 ) ) ;
#10882 = CARTESIAN_POINT ( 'NONE',  ( -56.51778961428590975, -281.7837064650937577, -341.5157758952734639 ) ) ;
#10883 = CARTESIAN_POINT ( 'NONE',  ( -68.74913522007797440, -280.9455571570364327, -203.9170324626630872 ) ) ;
#10884 = CARTESIAN_POINT ( 'NONE',  ( 39.34188165271749682, -288.4364396345058026, -265.8203297771192410 ) ) ;
#10885 = CARTESIAN_POINT ( 'NONE',  ( -83.04036938952030766, -278.1892808830866102, -327.4316655560248819 ) ) ;
#10886 = CARTESIAN_POINT ( 'NONE',  ( -111.2456412186606514, -289.6013897656955010, -250.1565755494168286 ) ) ;
#10887 = CARTESIAN_POINT ( 'NONE',  ( -104.2713272462240468, -284.8629556578851520, -308.2125189117822970 ) ) ;
#10888 = CARTESIAN_POINT ( 'NONE',  ( -33.73648894178771940, -286.5887254025682296, -193.5071697713474350 ) ) ;
#10889 = CARTESIAN_POINT ( 'NONE',  ( -70.21302376918448829, -283.6644988937621292, -335.5554315235995659 ) ) ;
#10890 = VERTEX_POINT ( 'NONE', #76971 ) ;
#10891 = CARTESIAN_POINT ( 'NONE',  ( -26.41588298435790350, -486.4924983417995463, -472.6442049081569508 ) ) ;
#10892 = CARTESIAN_POINT ( 'NONE',  ( -111.9597024112458570, -292.5794805507978822, -257.2287451113072621 ) ) ;
#10893 = CARTESIAN_POINT ( 'NONE',  ( 29.05601480467808528, -291.7399915758287534, -232.3526751914484691 ) ) ;
#10894 = CARTESIAN_POINT ( 'NONE',  ( -31.30841593742026419, -273.1889315191523337, -197.3620731682969449 ) ) ;
#10895 = CARTESIAN_POINT ( 'NONE',  ( -72.03548057987100606, -294.8474461953565537, -338.9880397041938522 ) ) ;
#10896 = CARTESIAN_POINT ( 'NONE',  ( -90.30125678704624193, -289.7656129742889561, -219.1166733008099925 ) ) ;
#10897 = CARTESIAN_POINT ( 'NONE',  ( -68.97045614702022931, -293.7136667199707176, -337.2898813892948624 ) ) ;
#10898 = CARTESIAN_POINT ( 'NONE',  ( -7.120697760712635827, -293.6628054910511878, -203.4744861206333724 ) ) ;
#10899 = DIRECTION ( 'NONE',  ( 0.000000000000000000, 0.000000000000000000, 1.000000000000000000 ) ) ;
#10900 = CARTESIAN_POINT ( 'NONE',  ( 37.87703502512747633, -291.5516737012878252, -270.3365989762054369 ) ) ;
#10901 = CARTESIAN_POINT ( 'NONE',  ( -78.60353246568196539, -297.6075134645395224, -333.0516871339069098 ) ) ;
#10902 = CARTESIAN_POINT ( 'NONE',  ( 34.22339099837354581, -288.2889165938020142, -254.8097135135828921 ) ) ;
#10903 = CARTESIAN_POINT ( 'NONE',  ( -25.99226979892631206, -278.8881998667927178, -344.8567368587943633 ) ) ;
#10904 = CARTESIAN_POINT ( 'NONE',  ( -45.62202854961023490, -275.9496708821050674, -346.5679896372945450 ) ) ;
#10905 = CARTESIAN_POINT ( 'NONE',  ( -93.53765840327440628, -296.4659230409811244, -217.8795776110415829 ) ) ;
#10906 = CARTESIAN_POINT ( 'NONE',  ( 1.382771120973315337, -274.7673902280189964, -333.4958028998477744 ) ) ;
#10907 = CARTESIAN_POINT ( 'NONE',  ( -100.6803746712757288, -277.1620261672334209, -231.1536718745393273 ) ) ;
#10908 = CARTESIAN_POINT ( 'NONE',  ( -109.9111147165462228, -276.6548180003418906, -293.7716438872411686 ) ) ;
#10909 = ADVANCED_FACE ( 'NONE', ( #61387 ), #3129, .F. ) ;
#10910 = DIRECTION ( 'NONE',  ( 0.000000000000000000, 0.000000000000000000, -1.000000000000000000 ) ) ;
#10911 = CARTESIAN_POINT ( 'NONE',  ( -87.40915018039754614, -273.9831083231292723, -217.0269643228989764 ) ) ;
#10912 = PLANE ( 'NONE',  #20227 ) ;
#10913 = CIRCLE ( 'NONE', #38145, 23.00000000000000711 ) ;
#10915 = CARTESIAN_POINT ( 'NONE',  ( -21.93195891545083853, -274.0884831370159986, -199.0060909680411783 ) ) ;
#10914 = CARTESIAN_POINT ( 'NONE',  ( -20.88079449138717791, -286.8621482966319149, -343.9499475225034075 ) ) ;
#10916 = AXIS2_PLACEMENT_3D ( 'NONE', #29721, #58603, #87444 ) ;
#10917 = CARTESIAN_POINT ( 'NONE',  ( 37.37682736240206083, -287.3193898071705235, -251.7562355681538975 ) ) ;
#10918 = CARTESIAN_POINT ( 'NONE',  ( -112.5083667949886888, -274.5519907589103354, -270.3865271280112097 ) ) ;
#10919 = CARTESIAN_POINT ( 'NONE',  ( -98.70085006719020271, -293.9693470209815587, -313.1989884521789804 ) ) ;
#10920 = AXIS2_PLACEMENT_3D ( 'NONE', #13417, #5839, #42262 ) ;
#10921 = CARTESIAN_POINT ( 'NONE',  ( 17.70344643396533613, -281.4866221237117543, -324.0486128710462026 ) ) ;
#10922 = AXIS2_PLACEMENT_3D ( 'NONE', #60219, #89522, #88131 ) ;
#10923 = CARTESIAN_POINT ( 'NONE',  ( 10.92051741093306205, -278.7192061292386711, -212.8853281000835125 ) ) ;
#10924 = CARTESIAN_POINT ( 'NONE',  ( 200.7510921130352415, 288.0788353042884751, -5.420371282781244027 ) ) ;
#10925 = CARTESIAN_POINT ( 'NONE',  ( -109.3311876663043307, -289.1585381048878958, -284.7308602091442822 ) ) ;
#10926 = CARTESIAN_POINT ( 'NONE',  ( 200.1030226942293098, 214.6007075219629030, -2.515500450062353899 ) ) ;
#10927 = DIRECTION ( 'NONE',  ( -0.000000000000000000, 1.000000000000000000, -0.000000000000000000 ) ) ;
#10928 = CARTESIAN_POINT ( 'NONE',  ( -111.2431445606223548, -288.7200106620329620, -257.2754408121874121 ) ) ;
#10929 = CARTESIAN_POINT ( 'NONE',  ( 5.564858526132587357, -276.1648335446911346, -210.3836622949784498 ) ) ;
#10930 = CARTESIAN_POINT ( 'NONE',  ( 13.30392837838768472, -283.7856787407495176, -327.6471775522419989 ) ) ;
#10932 = CARTESIAN_POINT ( 'NONE',  ( -26.74277571119780816, -282.9137202105658275, -342.6388864808363905 ) ) ;
#10931 = CARTESIAN_POINT ( 'NONE',  ( -51.46703495452751298, -295.8926230805512319, -196.2884743318714413 ) ) ;
#10933 = CARTESIAN_POINT ( 'NONE',  ( -5.065874897012928813, -275.9108686779624122, -204.2136374346252978 ) ) ;
#10934 = CARTESIAN_POINT ( 'NONE',  ( -2.846534649821085949, -275.3233428741677926, -205.8422425588160820 ) ) ;
#10935 = EDGE_CURVE ( 'NONE', #74457, #43263, #11136, .T. ) ;
#10936 = CARTESIAN_POINT ( 'NONE',  ( -68.33606214928872191, -285.4594106713332735, -338.6712030926112789 ) ) ;
#10937 = CARTESIAN_POINT ( 'NONE',  ( -37.81203744875236339, -297.1048641811096331, -197.1273332126014566 ) ) ;
#10938 = ORIENTED_EDGE ( 'NONE', *, *, #71944, .T. ) ;
#10939 = CARTESIAN_POINT ( 'NONE',  ( 175.2296996224750103, 21.00000000000000000, -15.00000000000000000 ) ) ;
#10940 = CARTESIAN_POINT ( 'NONE',  ( 39.44122556016269243, -293.3132138825386050, -264.5833738515132154 ) ) ;
#10941 = CARTESIAN_POINT ( 'NONE',  ( -97.22656306484043398, -285.9207346792924227, -314.9217507922982691 ) ) ;
#10942 = ADVANCED_FACE ( 'NONE', ( #84060 ), #5006, .T. ) ;
#10943 = DIRECTION ( 'NONE',  ( 0.2456588035076310295, -0.9693563597868428694, 0.000000000000000000 ) ) ;
#10944 = CARTESIAN_POINT ( 'NONE',  ( 36.60358173371529489, -278.6237833571632905, -234.7871824221999191 ) ) ;
#10945 = CARTESIAN_POINT ( 'NONE',  ( -84.77474732016597159, -276.8840595240507696, -330.8792488849715596 ) ) ;
#10946 = CARTESIAN_POINT ( 'NONE',  ( -111.4890281604978668, -288.7293136408266605, -287.9844273774644421 ) ) ;
#10947 = CARTESIAN_POINT ( 'NONE',  ( -56.48049038906741970, -284.8234610527591144, -341.5258175041921618 ) ) ;
#10948 = CARTESIAN_POINT ( 'NONE',  ( -39.16050599114966246, -278.8354312450923089, -344.3521036569139255 ) ) ;
#10949 = CARTESIAN_POINT ( 'NONE',  ( -93.49911713459866291, -286.6889984507919280, -218.4670415465290034 ) ) ;
#10950 = CARTESIAN_POINT ( 'NONE',  ( -24.55992040486605887, -282.2154531726777691, -196.4582983260262381 ) ) ;
#10951 = CARTESIAN_POINT ( 'NONE',  ( 26.92939223182577280, -275.1611961526215850, -227.9556149037361195 ) ) ;
#10952 = CARTESIAN_POINT ( 'NONE',  ( -31.45238450712145450, -276.8131841377852425, -347.1881899096321717 ) ) ;
#10953 = CARTESIAN_POINT ( 'NONE',  ( -99.93106445781967295, -297.9242670308082666, -310.7529661689855516 ) ) ;
#10954 = PLANE ( 'NONE',  #33883 ) ;
#10955 = CARTESIAN_POINT ( 'NONE',  ( -106.6662871844225293, -281.4805209788417528, -237.0123917617630980 ) ) ;
#10956 = CARTESIAN_POINT ( 'NONE',  ( -109.1369972974880937, -271.1099784194080371, -245.4731828104865201 ) ) ;
#10957 = CARTESIAN_POINT ( 'NONE',  ( -16.36919670121143611, -276.2814407686956315, -340.4009013751984867 ) ) ;
#10958 = CARTESIAN_POINT ( 'NONE',  ( -21.45220796181182621, -275.4566289245137227, -195.4242595204761983 ) ) ;
#10959 = CARTESIAN_POINT ( 'NONE',  ( 35.99716102564403997, -289.1777284591159969, -260.0183744527114413 ) ) ;
#10960 = CARTESIAN_POINT ( 'NONE',  ( -44.70923719324815693, -296.6637711608207155, -346.3642052802466651 ) ) ;
#10961 = CARTESIAN_POINT ( 'NONE',  ( -33.43963587920578817, -296.2091580762302669, -346.8776506496019465 ) ) ;
#10962 = CARTESIAN_POINT ( 'NONE',  ( -104.0552475132521550, -293.0027907728751870, -236.3445484442329700 ) ) ;
#10963 = CARTESIAN_POINT ( 'NONE',  ( -1.055344631209611528, -278.5348183071635617, -204.9139726459793565 ) ) ;
#10964 = CARTESIAN_POINT ( 'NONE',  ( -3.718603246501502646, -282.4194396576424992, -203.9330890450153788 ) ) ;
#10965 = CARTESIAN_POINT ( 'NONE',  ( -89.10994746790565557, -295.3975757147995864, -216.7974677063391482 ) ) ;
#10966 = CARTESIAN_POINT ( 'NONE',  ( -58.12480224572666998, -285.1781700703280080, -343.2742699700966114 ) ) ;
#10967 = CARTESIAN_POINT ( 'NONE',  ( 24.49172460557148412, -287.0147056594360038, -309.7419973420132919 ) ) ;
#10968 = CARTESIAN_POINT ( 'NONE',  ( -20.36879062156694786, -109.3229610787347923, -362.1159644462802021 ) ) ;
#10969 = ORIENTED_EDGE ( 'NONE', *, *, #21310, .F. ) ;
#10970 = CARTESIAN_POINT ( 'NONE',  ( 35.70163485141603132, -287.1918994139536494, -268.3161009710789813 ) ) ;
#10971 = ORIENTED_EDGE ( 'NONE', *, *, #90632, .T. ) ;
#10972 = CARTESIAN_POINT ( 'NONE',  ( -33.06219580151827131, -284.0791327376361437, -346.9455939830428974 ) ) ;
#10973 = CARTESIAN_POINT ( 'NONE',  ( -56.87135073797514195, -274.1266875804957408, -199.9473149587551291 ) ) ;
#10974 = CARTESIAN_POINT ( 'NONE',  ( -1.143572649972678601, -285.3165631670063931, -202.8503463500382225 ) ) ;
#10975 = CARTESIAN_POINT ( 'NONE',  ( -6.336425542486779250, -281.3908171536571672, -200.1222997126138807 ) ) ;
#10976 = CARTESIAN_POINT ( 'NONE',  ( 195.7317764926344239, 19.56557103583841695, -12.90780099963700600 ) ) ;
#10977 = CARTESIAN_POINT ( 'NONE',  ( -113.3550901977310730, -280.1639160325332796, -263.0993373856484823 ) ) ;
#10978 = CARTESIAN_POINT ( 'NONE',  ( 28.28919821757781961, -282.4123239606552147, -310.6906093150817014 ) ) ;
#10979 = CARTESIAN_POINT ( 'NONE',  ( -6.941161984400256557, -289.9809262143061233, -207.3071070584150277 ) ) ;
#10980 = CARTESIAN_POINT ( 'NONE',  ( 139.6957795963261333, 180.2233390436421985, -241.5434084867537763 ) ) ;
#10981 = ORIENTED_EDGE ( 'NONE', *, *, #7600, .F. ) ;
#10982 = AXIS2_PLACEMENT_3D ( 'NONE', #57536, #14456, #43313 ) ;
#10983 = CARTESIAN_POINT ( 'NONE',  ( 23.98249658564035869, -278.1367644760755979, -313.3380138231381693 ) ) ;
#10984 = CARTESIAN_POINT ( 'NONE',  ( 202.6185701365793363, 295.9433668349635127, -68.63232107392525450 ) ) ;
#10985 = CARTESIAN_POINT ( 'NONE',  ( 34.70767268040145836, -279.3196168398559962, -250.7997294482875361 ) ) ;
#10986 = CARTESIAN_POINT ( 'NONE',  ( 25.68394968003943291, -295.8789684273773446, -312.8080434303172410 ) ) ;
#10987 = CARTESIAN_POINT ( 'NONE',  ( -61.05406336697056702, -294.7167022270934922, -339.5640031186309784 ) ) ;
#10988 = CARTESIAN_POINT ( 'NONE',  ( -7.208520942112449426, -291.9445882052895058, -199.5547283942408114 ) ) ;
#10989 = CARTESIAN_POINT ( 'NONE',  ( -110.6395504404451202, -271.5021484970271217, -270.3477489206637756 ) ) ;
#10990 = AXIS2_PLACEMENT_3D ( 'NONE', #10309, #3215, #58669 ) ;
#10992 = CARTESIAN_POINT ( 'NONE',  ( 6.301493406326240887, -286.8486100140940493, -329.9370774783134266 ) ) ;
#10991 = CARTESIAN_POINT ( 'NONE',  ( -113.5317549249391931, -295.2082840836710034, -263.9020585142498589 ) ) ;
#10993 = CARTESIAN_POINT ( 'NONE',  ( 36.76614841840203241, -295.3457196071952353, -265.2073783910465750 ) ) ;
#10994 = CARTESIAN_POINT ( 'NONE',  ( -109.6813983477632490, -286.0382018756369575, -257.3205931007504432 ) ) ;
#10995 = ORIENTED_EDGE ( 'NONE', *, *, #53031, .T. ) ;
#10996 = CARTESIAN_POINT ( 'NONE',  ( 35.26778301244063840, -294.8101879553623803, -295.4376004276389267 ) ) ;
#10997 = VECTOR ( 'NONE', #33030, 1000.000000000000000 ) ;
#10998 = CARTESIAN_POINT ( 'NONE',  ( -104.1670597106370053, -284.6473490094984982, -299.8968549486609163 ) ) ;
#10999 = CARTESIAN_POINT ( 'NONE',  ( -111.8844013291345192, -295.5689325182196399, -252.7147467386035089 ) ) ;
#11000 = CARTESIAN_POINT ( 'NONE',  ( -89.37461083492657110, -290.5658807097030376, -326.9007945244755433 ) ) ;
#11001 = CARTESIAN_POINT ( 'NONE',  ( -112.8657572861379776, -291.2291570634452569, -255.6076462779012672 ) ) ;
#11002 = CARTESIAN_POINT ( 'NONE',  ( -68.75605496183426624, -289.6437065493519754, -336.2560215405648592 ) ) ;
#11003 = ORIENTED_EDGE ( 'NONE', *, *, #10664, .F. ) ;
#11004 = CARTESIAN_POINT ( 'NONE',  ( -113.5000000000000568, -192.7866584945343504, -447.4016117689005796 ) ) ;
#11005 = CARTESIAN_POINT ( 'NONE',  ( -102.7948592003603068, -298.9183566516531414, -232.0976227465491206 ) ) ;
#11006 = CARTESIAN_POINT ( 'NONE',  ( -41.15755585938099870, -272.8001929367039224, -193.8012977609677705 ) ) ;
#11007 = EDGE_CURVE ( 'NONE', #71850, #7049, #81988, .T. ) ;
#11008 = CARTESIAN_POINT ( 'NONE',  ( -6.659937873120455265, -279.5238850640776604, -203.8490222498963931 ) ) ;
#11009 = CARTESIAN_POINT ( 'NONE',  ( -7.708479792108360762, -273.9377827044723404, -199.3017526767342815 ) ) ;
#11010 = CARTESIAN_POINT ( 'NONE',  ( -105.6114186778319066, -294.6638368010980003, -298.1091499861007605 ) ) ;
#11011 = CARTESIAN_POINT ( 'NONE',  ( 17.45871661260689223, -278.1191088163350855, -320.4578222363978739 ) ) ;
#11012 = CARTESIAN_POINT ( 'NONE',  ( 23.30336918773956612, -273.1038502388787492, -227.5250752061944013 ) ) ;
#11013 = CARTESIAN_POINT ( 'NONE',  ( -68.22853613027979236, -298.8423152017647340, -203.7655948570242970 ) ) ;
#11014 = CARTESIAN_POINT ( 'NONE',  ( -110.4060775363904838, -297.5453956666506201, -276.9410109938169171 ) ) ;
#11015 = CARTESIAN_POINT ( 'NONE',  ( 144.7857639756989272, -299.5541904835127980, -197.2582414438974183 ) ) ;
#11016 = CARTESIAN_POINT ( 'NONE',  ( -110.4421046932612569, -297.8790715365221899, -291.9192175517947021 ) ) ;
#11017 = CARTESIAN_POINT ( 'NONE',  ( 28.79935195122864400, -296.8780820938325746, -195.2169294587867796 ) ) ;
#11018 = CARTESIAN_POINT ( 'NONE',  ( 25.88497798491060919, -294.7062408111802370, -307.0528042718527786 ) ) ;
#11019 = CARTESIAN_POINT ( 'NONE',  ( 26.75664534524298332, -291.6348076457171601, -234.1076558627702013 ) ) ;
#11020 = CARTESIAN_POINT ( 'NONE',  ( 154.9842916688210153, 275.0000000000000568, 12.88888888888891771 ) ) ;
#11021 = CARTESIAN_POINT ( 'NONE',  ( 37.18070276567564747, -276.2840839297336402, -289.4906336686852910 ) ) ;
#11022 = CARTESIAN_POINT ( 'NONE',  ( -49.96174262937216781, -298.2199525940888520, -198.4387847754279051 ) ) ;
#11023 = AXIS2_PLACEMENT_3D ( 'NONE', #8988, #11797, #10389 ) ;
#11024 = CARTESIAN_POINT ( 'NONE',  ( 35.39070111244882355, -283.2792772165214501, -250.6042633343988939 ) ) ;
#11025 = CARTESIAN_POINT ( 'NONE',  ( -88.00757297697549575, -282.4279933527611774, -327.7578456336591444 ) ) ;
#11026 = CIRCLE ( 'NONE', #71556, 0.9999999999999991118 ) ;
#11027 = CARTESIAN_POINT ( 'NONE',  ( -87.03565260565629558, -277.0713971588913296, -329.1148982752972074 ) ) ;
#11028 = CARTESIAN_POINT ( 'NONE',  ( 208.4306832106271088, -74.55766379199613425, 0.000000000000000000 ) ) ;
#11029 = CARTESIAN_POINT ( 'NONE',  ( -71.49329828238441564, -282.7126387187799992, -335.0625095507746778 ) ) ;
#11030 = CARTESIAN_POINT ( 'NONE',  ( -99.90764157670690793, -281.9892592117703884, -312.1142658533706253 ) ) ;
#11031 = ADVANCED_FACE ( 'NONE', ( #40026 ), #23243, .T. ) ;
#11032 = CARTESIAN_POINT ( 'NONE',  ( 35.96690450626989843, -274.0355544208524066, -263.3827790019315671 ) ) ;
#11033 = CARTESIAN_POINT ( 'NONE',  ( -104.6145755453458293, -280.1136154768362871, -303.6337203406936851 ) ) ;
#11034 = DIRECTION ( 'NONE',  ( -0.000000000000000000, -0.000000000000000000, -1.000000000000000000 ) ) ;
#11035 = DIRECTION ( 'NONE',  ( 0.000000000000000000, 1.000000000000000000, 0.000000000000000000 ) ) ;
#11036 = CARTESIAN_POINT ( 'NONE',  ( -93.54132735638877705, -271.6595100805591301, -218.8827261971229916 ) ) ;
#11037 = CARTESIAN_POINT ( 'NONE',  ( -103.3531063362100184, -280.0757008758207576, -306.3127893519672966 ) ) ;
#11038 = CARTESIAN_POINT ( 'NONE',  ( 200.1126601882107252, 250.0000000000000568, -2.416251949619908412 ) ) ;
#11039 = CARTESIAN_POINT ( 'NONE',  ( -103.1506025912072460, -285.9800972611657812, -307.5952228160468849 ) ) ;
#11040 = CARTESIAN_POINT ( 'NONE',  ( 208.6451419912077085, 38.33121871055298868, 12.00000001296747598 ) ) ;
#11041 = CARTESIAN_POINT ( 'NONE',  ( 31.49988911538259018, -285.1611304524824959, -240.4689079486662706 ) ) ;
#11042 = DIRECTION ( 'NONE',  ( 1.000000000000000000, 0.000000000000000000, 0.000000000000000000 ) ) ;
#11043 = CARTESIAN_POINT ( 'NONE',  ( -86.76863518983608969, -294.5530777084238139, -324.6207585483201115 ) ) ;
#11044 = CARTESIAN_POINT ( 'NONE',  ( -29.05842763463842005, -287.0856349043655769, -344.1327444805640994 ) ) ;
#11045 = CARTESIAN_POINT ( 'NONE',  ( 156.1965750133424251, 18.75975317436470391, -8.718057073926514633 ) ) ;
#11046 = CARTESIAN_POINT ( 'NONE',  ( -101.5974894090540204, -295.0712285570374434, -231.5795083821487879 ) ) ;
#11047 = CARTESIAN_POINT ( 'NONE',  ( -49.21755219762061273, -284.3834541991189440, -194.9310016894561670 ) ) ;
#11048 = CARTESIAN_POINT ( 'NONE',  ( 29.69088422181411957, -282.7388465408901652, -239.3668416304933260 ) ) ;
#11049 = CARTESIAN_POINT ( 'NONE',  ( -8.445278346757712384, -280.9190452645461278, -340.6947165030421161 ) ) ;
#11050 = CARTESIAN_POINT ( 'NONE',  ( -94.95056600423031057, -289.9202355592743743, -315.2167747613553388 ) ) ;
#11051 = CIRCLE ( 'NONE', #51877, 24.00000000000000355 ) ;
#11052 = CARTESIAN_POINT ( 'NONE',  ( -96.09304980416767705, -280.5951228408779343, -226.0270613269139233 ) ) ;
#11053 = CARTESIAN_POINT ( 'NONE',  ( -72.21566148290209242, -280.3810604414051113, -206.0462009982429663 ) ) ;
#11054 = EDGE_CURVE ( 'NONE', #75279, #54193, #61836, .T. ) ;
#11055 = CARTESIAN_POINT ( 'NONE',  ( 28.67810496033440515, -289.0500089654581757, -233.9239704021375701 ) ) ;
#11056 = AXIS2_PLACEMENT_3D ( 'NONE', #16292, #45145, #60326 ) ;
#11057 = ORIENTED_EDGE ( 'NONE', *, *, #32100, .F. ) ;
#11058 = CARTESIAN_POINT ( 'NONE',  ( -112.4432852073904883, -272.7646693551740782, -253.3684160615795520 ) ) ;
#11059 = CARTESIAN_POINT ( 'NONE',  ( -108.5787140985212318, -292.8215292307491495, -248.0214957618943004 ) ) ;
#11060 = CARTESIAN_POINT ( 'NONE',  ( 209.6287663260175975, 29.00782453271232697, 10.49999999999999822 ) ) ;
#11061 = CARTESIAN_POINT ( 'NONE',  ( -55.63300648810263738, -294.3376638359845288, -190.3683826091709363 ) ) ;
#11062 = ORIENTED_EDGE ( 'NONE', *, *, #17386, .T. ) ;
#11063 = CARTESIAN_POINT ( 'NONE',  ( -4.811872070706630922, -274.6246261199796095, -338.1383761130663856 ) ) ;
#11064 = CARTESIAN_POINT ( 'NONE',  ( -83.63170945779077670, -296.0521521680024080, -421.1172536214571096 ) ) ;
#11065 = CARTESIAN_POINT ( 'NONE',  ( -71.73141684349430136, -293.8988845066755289, -338.3595576862630878 ) ) ;
#11066 = CARTESIAN_POINT ( 'NONE',  ( -11.44636086817499177, -273.7470456629229147, -201.9452788165103243 ) ) ;
#11067 = AXIS2_PLACEMENT_3D ( 'NONE', #16409, #31554, #46205 ) ;
#11068 = CARTESIAN_POINT ( 'NONE',  ( -37.24788492967900311, -290.5710802136277948, -344.0543941582762386 ) ) ;
#11069 = B_SPLINE_SURFACE_WITH_KNOTS ( 'NONE', 3, 3, ( 
 ( #74222, #59101, #45318, #29293, #65770, #81781, #8879, #30677, #66664, #36854, #9341, #72833, #73315, #65299, #15075, #87481, #37758, #7501, #43936, #38226, #59577, #31156, #7959, #879, #22630, #60042, #1328, #29759, #67139, #2273, #43488, #22182, #51503, #24028, #73767, #79938, #8427, #52903, #405, #72384 ),
 ( #87942, #51050, #23577, #58188, #66212, #58639, #87030, #23093, #88879, #80391, #15535, #44864, #37306, #51976, #16012, #52444, #81318, #75166, #76568, #11691, #76097, #10748, #33462, #46262, #11230, #69001, #89818, #3666, #25428, #53374, #91208, #60502, #10279, #24979, #62365, #53853, #61894, #39605, #90727, #40542 ),
 ( #39149, #17870, #26376, #68060, #69457, #82718, #83646, #89338, #4132, #54306, #55264, #68529, #32554, #16931, #4588, #45792, #3186, #74703, #33003, #24493, #9824, #25887, #32070, #60967, #40084, #38697, #67604, #2732, #83180, #31612, #61446, #54769, #18329, #82260, #46722, #75625, #18810, #47667, #90277, #47185 ),
 ( #63790, #21135, #48127, #92154, #50004, #28256, #56684, #93555, #84580, #78898, #71342, #71821, #48598, #19729, #34416, #6941, #41960, #55728, #14045, #42908, #28713, #62855, #63323, #64728, #20678, #26840, #20207, #84119, #77030, #19269, #6472, #6004, #34878, #91688, #78444, #12160, #13124, #77498, #41004, #70873 ),
 ( #64272, #27791, #92620, #12645, #69927, #41490, #85056, #5546, #85531, #70420, #27310, #56197, #49549, #35350, #57144, #49085, #5069, #13580, #77983, #42431, #93101, #35814, #85985, #33951, #88313, #44295, #59461, #43376, #79830, #37204, #29175, #14970, #50947, #58534, #9232, #22077, #16360, #65656, #30563, #7390 ),
 ( #7848, #21601, #58071, #87379, #66560, #769, #22988, #15428, #36735, #51862, #38112, #23470, #22526, #43826, #66112, #1225, #51398, #52336, #15906, #72271, #50482, #36271, #73203, #65191, #295, #79383, #8322, #80288, #81214, #30107, #44763, #14521, #58989, #45211, #86924, #29654, #74113, #1681, #87837, #67022 ),
 ( #80755, #72726, #73663, #2158, #8774, #37652, #57598, #86442, #61785, #67497, #89700, #89233, #24866, #75982, #60857, #24385, #75062, #68420, #82146, #16821, #45679, #53749, #88776, #3550, #59937, #11110, #32439, #82615, #2628, #23924, #38594, #31963, #46158, #75517, #9714, #10173, #53264, #61338, #18225, #68892 ),
 ( #39043, #17762, #39498, #31507, #11582, #74586, #17302, #67954, #47556, #3079, #39977, #46616, #4022, #90617, #10639, #32897, #90175, #25323, #83534, #25779, #54660, #54203, #83071, #60395, #52794, #47075, #81673, #18693, #76461, #40430, #69348, #31047, #56088, #77390, #92510, #78794, #64161, #34309, #84472, #13019 ),
 ( #92994, #56575, #84014, #91087, #19162, #84941, #12052, #40899, #62252, #48973, #92047, #35236, #20092, #85428, #26258, #77870, #28152, #55152, #12527, #57041, #42325, #70768, #13938, #42796, #63686, #20576, #27677, #91580, #6364, #33839, #5442, #48019, #69818, #48490, #49448, #76924, #4953, #85879, #78336, #21031 ),
 ( #5901, #49899, #4478, #41377, #62748, #41855, #70311, #63215, #26736, #33355, #34771, #27201, #13478, #71236, #55623, #19622, #72621, #29546, #72170, #35713, #21971, #64627, #7286, #7743, #80638, #79727, #37095, #58426, #50844, #66004, #53507, #37541, #36626, #57958, #80182, #15320, #65547, #66452, #29997, #57497 ),
 ( #58882, #44180, #28608, #86813, #86340, #1116, #87728, #93453, #22418, #44653, #662, #17533, #71712, #87272, #36164, #8663, #22880, #31732, #65085, #43723, #73086, #29067, #51290, #15794, #8217, #51746, #21491, #73554, #2851, #14415, #60623, #185, #89461, #24622, #6839, #79274, #50370, #82384, #43272, #14869 ),
 ( #54898, #83299, #18447, #39267, #12287, #83775, #69120, #47305, #54428, #75283, #11351, #91337, #76220, #39730, #90391, #18931, #3789, #32195, #61100, #40204, #10402, #47786, #68184, #26499, #76687, #4246, #17989, #3305, #53969, #33126, #61558, #90850, #25095, #25547, #10867, #11812, #33589, #84241, #62015, #89940 ),
 ( #40663, #82836, #26966, #46841, #68653, #26012, #62981, #69583, #55390, #4711, #19391, #41131, #32672, #48254, #62498, #77156, #5205, #70064, #75744, #34079, #91814, #55857, #84710, #46383, #49671, #78106, #79510, #14647, #79032, #13705, #36403, #20340, #14186, #71950, #92755, #6606, #28379, #56328, #424, #63449 ),
 ( #50620, #35484, #21744, #5665, #42083, #93226, #85192, #70999, #13247, #20801, #65317, #6131, #72400, #27923, #86575, #92280, #7070, #57270, #58205, #71474, #64400, #19857, #43504, #48728, #49210, #7518, #35941, #27436, #77630, #64859, #35002, #63918, #43047, #29311, #70543, #12780, #86114, #34541, #21263, #93686 ),
 ( #56811, #41622, #50133, #42557, #85653, #28844, #57728, #78567, #22525, #73662, #6940, #50946, #8773, #80754, #15427, #52335, #81213, #8321, #30106, #66111, #36270, #44762, #72270, #43825, #64727, #14520, #86923, #37203, #35813, #43375, #37651, #58988, #30562, #7389, #65190, #22076, #59460, #768, #294, #66559 ),
 ( #21600, #79829, #23469, #73202, #79382, #72725, #42907, #93554, #71820, #87836, #58533, #87378, #50481, #1224, #28712, #65655, #29174, #57597, #29653, #88312, #58070, #86441, #51397, #14969, #1680, #7847, #36734, #80287, #44294, #22987, #51861, #15905, #46157, #90616, #9231, #54659, #3549, #31962, #60856, #23923 ),
 ( #2157, #31046, #75061, #74112, #82614, #45210, #90174, #53748, #39042, #81672, #38111, #52793, #17301, #31506, #89699, #88775, #60394, #74585, #46615, #32438, #54202, #24384, #67021, #24865, #16820, #68419, #45678, #47074, #9713, #83070, #75981, #3078, #18224, #59936, #38593, #17761, #67496, #2627, #89232, #10172 ),
 ( #11109, #39976, #67953, #75516, #53263, #82145, #10638, #39497, #61337, #25322, #68891, #4021, #32896, #61784, #25778, #16359, #64160, #49447, #19621, #69817, #92046, #27200, #77389, #78335, #41854, #69347, #76460, #4477, #41376, #91086, #26257, #47555, #34308, #12526, #20575, #5441, #70767, #11581, #63214, #13477 ),
 ( #48018, #42324, #5900, #71235, #19161, #55622, #56087, #40898, #48489, #92509, #84940, #20091, #40429, #34770, #6363, #55151, #70310, #76923, #63685, #48972, #18692, #84013, #33354, #77869, #35235, #92993, #28151, #62251, #33838, #83533, #13018, #12051, #27676, #4952, #62747, #91579, #56574, #85427, #26735, #84471 ),
 ( #42795, #71711, #86812, #21030, #29545, #85878, #37094, #661, #79726, #28607, #49898, #64626, #57957, #72169, #7742, #35712, #7285, #21490, #87271, #44179, #1115, #65084, #78793, #36625, #57496, #15319, #86339, #87727, #50369, #29996, #22879, #43722, #58881, #6838, #79273, #65546, #14414, #43271, #36163, #21970 ),
 ( #51745, #80637, #50843, #14868, #184, #13937, #29066, #93452, #72620, #58425, #66003, #22417, #51289, #80181, #73085, #8216, #37540, #15793, #44652, #73553, #8662, #66451, #1569, #57040, #82503, #16249, #23356, #45099, #82024, #37995, #66903, #88196, #74950, #24269, #61222, #46045, #17651, #52223, #10060, #90056 ),
 ( #25209, #68303, #2964, #39853, #68776, #89580, #46502, #53633, #23812, #32319, #59822, #31391, #81106, #2042, #74460, #24750, #74001, #30932, #54082, #75405, #18106, #88663, #52675, #9592, #46959, #17181, #81556, #10519, #16704, #45559, #39388, #75861, #9118, #30452, #67839, #38480, #38930, #3424, #31850, #67384 ),
 ( #82952, #10984, #2514, #60739, #59345, #89118, #60281, #53144, #4827, #62135, #34651, #19967, #56445, #33239, #69698, #70189, #55026, #33710, #12898, #48369, #41248, #54544, #84818, #63564, #40318, #62622, #90966, #48841, #5323, #32782, #11467, #25662, #34191, #85307, #42198, #76805, #69233, #12401, #40779, #91462 ),
 ( #78218, #63095, #4362, #26613, #13357, #90502, #3905, #77746, #19502, #77272, #26131, #91923, #61670, #55504, #83896, #83412, #84353, #49324, #19047, #18565, #27078, #47431, #47903, #11931, #55964, #41736, #70649, #92391, #27551, #5777, #20456, #76341, #72849, #37776, #30695, #51520, #59118, #80882, #15092, #52921 ),
 ( #16482, #9359, #87959, #74239, #56924, #895, #51995, #43952, #29778, #65786, #73332, #24046, #36871, #31173, #80407, #45338, #22198, #59595, #16030, #16947, #30227, #23112, #71111, #38243, #6242, #7977, #2290, #88445, #51067, #35111, #23594, #92872, #44881, #67157, #64031, #15554, #60059, #88897, #73783, #81800 ) ),
 .UNSPECIFIED., .F., .F., .F.,
 ( 4, 3, 3, 3, 3, 3, 3, 3, 4 ),
 ( 4, 3, 3, 3, 3, 3, 3, 3, 3, 3, 3, 3, 3, 4 ),
 ( 0.4999999999999952816, 0.5624999999999958922, 0.6249999999999964473, 0.6874999999999971134, 0.7499999999999976685, 0.8124999999999982236, 0.8749999999999988898, 0.9374999999999994449, 1.000000000000000000 ),
 ( -3.628684052071867067E-13, 0.06249999999944978735, 0.1249999999992624372, 0.1874999999990751010, 0.2499999999988877508, 0.3749999999985130783, 0.4999999999981383780, 0.6249999999977636778, 0.6874999999975763831, 0.7499999999973889775, 0.8124999999972015718, 0.8749999999970142772, 0.9374999999968269826, 0.9999999999966395769 ),
 .UNSPECIFIED. ) ;
#11070 = CARTESIAN_POINT ( 'NONE',  ( -4.355686057685435486, -284.3713770222227026, -336.6174149818518231 ) ) ;
#11071 = CARTESIAN_POINT ( 'NONE',  ( -111.3467839346178465, -291.7369300115220767, -289.4358684843848550 ) ) ;
#11072 = CARTESIAN_POINT ( 'NONE',  ( -33.58046804292548160, -293.4137363237697400, -193.9467776616444326 ) ) ;
#11073 = CARTESIAN_POINT ( 'NONE',  ( 18.83173772143145897, -294.0467148364512582, -316.9824101643395693 ) ) ;
#11074 = CARTESIAN_POINT ( 'NONE',  ( -82.70804606998876807, -287.4321626089407005, -210.6376276157305654 ) ) ;
#11075 = CARTESIAN_POINT ( 'NONE',  ( 21.61138255414765297, -282.3857777287969384, -319.8942790647038805 ) ) ;
#11076 = CARTESIAN_POINT ( 'NONE',  ( -73.93090063162645720, -293.6136506036418155, -336.5298171532111269 ) ) ;
#11077 = CARTESIAN_POINT ( 'NONE',  ( -21.72806210196183230, -282.6906465273069102, -345.7614781413406604 ) ) ;
#11078 = CIRCLE ( 'NONE', #57949, 1.000000000000000888 ) ;
#11079 = CARTESIAN_POINT ( 'NONE',  ( 35.43180877955224872, -277.3171048313345750, -253.6949273144960557 ) ) ;
#11080 = EDGE_CURVE ( 'NONE', #55107, #91332, #46662, .T. ) ;
#11081 = CARTESIAN_POINT ( 'NONE',  ( 30.89617123739170168, -295.8376638359844719, -254.7536222014695397 ) ) ;
#11082 = CARTESIAN_POINT ( 'NONE',  ( -90.47988972230045590, -275.9340790327501622, -324.4405203246855081 ) ) ;
#11083 = CYLINDRICAL_SURFACE ( 'NONE', #25795, 7.500000000000007105 ) ;
#11084 = CARTESIAN_POINT ( 'NONE',  ( -24.06045461068103108, -282.3855664621608526, -342.2053728606200025 ) ) ;
#11085 = AXIS2_PLACEMENT_3D ( 'NONE', #46770, #69049, #68580 ) ;
#11086 = CARTESIAN_POINT ( 'NONE',  ( -109.2388601609837480, -280.0947830713159874, -243.7729323447709362 ) ) ;
#11087 = CARTESIAN_POINT ( 'NONE',  ( 20.11862170518067217, -285.9185702876018240, -219.3794757253718331 ) ) ;
#11088 = CARTESIAN_POINT ( 'NONE',  ( -3.188310742052926194, -294.2699080036458668, -204.6989522474358125 ) ) ;
#11089 = CARTESIAN_POINT ( 'NONE',  ( 33.96587379092136416, -276.8088303427197729, -243.4971957844319093 ) ) ;
#11090 = CARTESIAN_POINT ( 'NONE',  ( 35.59756893262619570, -277.1594066246558441, -293.4514038526494915 ) ) ;
#11091 = CARTESIAN_POINT ( 'NONE',  ( -68.03935441109793203, -277.3000987560183717, -336.6066861282340028 ) ) ;
#11092 = CARTESIAN_POINT ( 'NONE',  ( -70.08206762311330351, -299.6199537713510495, -203.0699835924160084 ) ) ;
#11093 = CARTESIAN_POINT ( 'NONE',  ( -108.2618046777853209, -282.8633569964112553, -246.3166656167947792 ) ) ;
#11094 = CARTESIAN_POINT ( 'NONE',  ( 17.47753067357390577, -292.4757889552715824, -216.2435132604818193 ) ) ;
#11095 = CARTESIAN_POINT ( 'NONE',  ( 37.04844308345818149, -289.3616629136205347, -286.9297551506215314 ) ) ;
#11096 = CIRCLE ( 'NONE', #6600, 4.000000000000003553 ) ;
#11097 = CARTESIAN_POINT ( 'NONE',  ( 35.73145807775177474, -292.5496759711669483, -276.2381599965387977 ) ) ;
#11098 = ORIENTED_EDGE ( 'NONE', *, *, #84781, .T. ) ;
#11099 = CARTESIAN_POINT ( 'NONE',  ( -76.84894947634538198, -290.1091620702991918, -204.8953367990457650 ) ) ;
#11100 = CARTESIAN_POINT ( 'NONE',  ( 24.86810874138845406, -292.6908015312446878, -232.0286543885544290 ) ) ;
#11101 = VERTEX_POINT ( 'NONE', #43324 ) ;
#11102 = CARTESIAN_POINT ( 'NONE',  ( -54.41934902124399542, -290.3461143080086799, -345.1808836089857095 ) ) ;
#11103 = CARTESIAN_POINT ( 'NONE',  ( -108.9888072818816482, -279.3955602562056129, -255.7866873382242829 ) ) ;
#11104 = CARTESIAN_POINT ( 'NONE',  ( -101.2843389529055713, -296.0319792565589978, -227.9953709198669287 ) ) ;
#11105 = CARTESIAN_POINT ( 'NONE',  ( -4.824601086436063113, -287.1206635216473728, -200.6764635957316329 ) ) ;
#11106 = CARTESIAN_POINT ( 'NONE',  ( 16.28141815142114979, -287.1219776718527328, -215.1315473029715122 ) ) ;
#11107 = CARTESIAN_POINT ( 'NONE',  ( -101.7878928193862151, -284.4164033898601929, -304.8020270895105455 ) ) ;
#11108 = CARTESIAN_POINT ( 'NONE',  ( 25.10643563140649448, -22.76097397130827815, -345.0702719944544583 ) ) ;
#11109 = CARTESIAN_POINT ( 'NONE',  ( 201.5605228849236426, 295.4036489450776344, -54.00000000002459188 ) ) ;
#11110 = CARTESIAN_POINT ( 'NONE',  ( -47.88318689526796845, -154.9995436933450605, -361.3103295439817089 ) ) ;
#11111 = CARTESIAN_POINT ( 'NONE',  ( 20.81610211598217930, -274.1262451277162882, -225.9527498682777775 ) ) ;
#11112 = CARTESIAN_POINT ( 'NONE',  ( 11.94540050142956567, -275.2684591037336190, -324.6979152150947243 ) ) ;
#11113 = CARTESIAN_POINT ( 'NONE',  ( -112.5390163706340729, -296.2642382456113523, -254.0241914527857148 ) ) ;
#11114 = CARTESIAN_POINT ( 'NONE',  ( 185.8120907569735891, 260.3495500449395195, -151.3467373205649835 ) ) ;
#11115 = CARTESIAN_POINT ( 'NONE',  ( 38.88771076079248701, -274.3189168564398983, -276.8707406564970483 ) ) ;
#11116 = CARTESIAN_POINT ( 'NONE',  ( -57.15413860319132766, -275.5533179835579176, -198.9953851041864823 ) ) ;
#11117 = ORIENTED_EDGE ( 'NONE', *, *, #56881, .T. ) ;
#11118 = CARTESIAN_POINT ( 'NONE',  ( -31.94217931762041118, -299.0594502518147237, -193.5955712977170151 ) ) ;
#11119 = CARTESIAN_POINT ( 'NONE',  ( -66.34769653104673637, -289.9346832550450586, -337.4721724312433935 ) ) ;
#11120 = CARTESIAN_POINT ( 'NONE',  ( -111.8096161828856339, -297.1168942843181640, -289.3532753395764416 ) ) ;
#11121 = CARTESIAN_POINT ( 'NONE',  ( -112.2444462341738642, -296.8237278202183802, -287.9994803679311985 ) ) ;
#11122 = CARTESIAN_POINT ( 'NONE',  ( -58.40620969087483161, -295.4988571916826459, -340.2559421211702215 ) ) ;
#11123 = ORIENTED_EDGE ( 'NONE', *, *, #266, .F. ) ;
#11124 = AXIS2_PLACEMENT_3D ( 'NONE', #91135, #39538, #68459 ) ;
#11125 = CARTESIAN_POINT ( 'NONE',  ( -69.66243976247527314, -279.3943817688218019, -338.6737756042700767 ) ) ;
#11126 = ORIENTED_EDGE ( 'NONE', *, *, #61815, .T. ) ;
#11127 = CARTESIAN_POINT ( 'NONE',  ( -14.24025656469665080, -279.8514351758454382, -196.9169089891026374 ) ) ;
#11128 = CIRCLE ( 'NONE', #2090, 2.000000000000000000 ) ;
#11129 = CARTESIAN_POINT ( 'NONE',  ( -16.30184157120112332, -277.7148091657475106, -340.5622356392174765 ) ) ;
#11130 = CARTESIAN_POINT ( 'NONE',  ( 26.80558192295882947, -277.8543387554825586, -311.1910231098851227 ) ) ;
#11131 = CARTESIAN_POINT ( 'NONE',  ( -39.93221443359873746, -275.1046283449192629, -345.6845682911584845 ) ) ;
#11132 = CARTESIAN_POINT ( 'NONE',  ( -36.74185794118342585, -274.5522376084319944, -197.2896163155269846 ) ) ;
#11133 = CARTESIAN_POINT ( 'NONE',  ( -58.05337773407750745, -296.3539720910771393, -199.7466624756449391 ) ) ;
#11134 = DIRECTION ( 'NONE',  ( -1.000000000000000000, -4.095251346825558428E-15, 0.000000000000000000 ) ) ;
#11135 = CARTESIAN_POINT ( 'NONE',  ( -85.10363866667154298, -277.8996709114925920, -325.6349349247532814 ) ) ;
#11136 = CIRCLE ( 'NONE', #77668, 5.000000000000000888 ) ;
#11137 = CARTESIAN_POINT ( 'NONE',  ( -52.52374249793685834, -274.6654095900231027, -194.9830589272008012 ) ) ;
#11138 = CARTESIAN_POINT ( 'NONE',  ( 25.43738772882143095, -286.8196198140358320, -314.1794402345108210 ) ) ;
#11139 = CARTESIAN_POINT ( 'NONE',  ( -27.29044299662773199, -276.1799215197347621, -195.9856428099257926 ) ) ;
#11140 = CARTESIAN_POINT ( 'NONE',  ( 208.4306832106271088, 0.000000000000000000, 0.000000000000000000 ) ) ;
#11141 = VECTOR ( 'NONE', #68705, 1000.000000000000000 ) ;
#11142 = CARTESIAN_POINT ( 'NONE',  ( -56.11687207286747991, -288.4972695515995724, -341.1251405500296983 ) ) ;
#11143 = CIRCLE ( 'NONE', #51965, 0.4999999999999989453 ) ;
#11144 = CARTESIAN_POINT ( 'NONE',  ( -112.8965053268430694, -284.0833714990520775, -255.7739410976076044 ) ) ;
#11145 = CARTESIAN_POINT ( 'NONE',  ( 36.70165498353557609, -279.7688454439426096, -268.5812678106142357 ) ) ;
#11147 = CARTESIAN_POINT ( 'NONE',  ( -33.13326652609070777, -284.1852695871455126, -195.9893681649109567 ) ) ;
#11146 = CARTESIAN_POINT ( 'NONE',  ( 28.31524924824635647, -279.6779163578821681, -237.0134559978289133 ) ) ;
#11148 = CARTESIAN_POINT ( 'NONE',  ( 34.14175854281398159, -289.8456935641403902, -293.0993790409129360 ) ) ;
#11149 = CARTESIAN_POINT ( 'NONE',  ( -110.3627934562378385, -279.8609853202134445, -262.4534051004393405 ) ) ;
#11150 = DIRECTION ( 'NONE',  ( 0.000000000000000000, 0.000000000000000000, 1.000000000000000000 ) ) ;
#11151 = CARTESIAN_POINT ( 'NONE',  ( -47.49843290267460816, -293.9233500554501575, -195.9996247949634380 ) ) ;
#11153 = CARTESIAN_POINT ( 'NONE',  ( -113.0323485360361246, -276.8841812740284922, -263.0883200953797996 ) ) ;
#11152 = CIRCLE ( 'NONE', #51974, 1.499999999999999556 ) ;
#11154 = CARTESIAN_POINT ( 'NONE',  ( -61.81614764838461440, -278.0301026354008513, -339.2981228691048159 ) ) ;
#11155 = CARTESIAN_POINT ( 'NONE',  ( -13.96727668575623404, -284.7497394021139030, -341.8010560670164182 ) ) ;
#11156 = FACE_BOUND ( 'NONE', #90130, .T. ) ;
#11157 = CARTESIAN_POINT ( 'NONE',  ( -56.89424512180426063, -291.2223974544353382, -343.4015707551772607 ) ) ;
#11158 = CARTESIAN_POINT ( 'NONE',  ( -96.08379003318228229, -295.1929095770927347, -223.7107914564602993 ) ) ;
#11159 = CIRCLE ( 'NONE', #3595, 4.000000000000003553 ) ;
#11160 = CARTESIAN_POINT ( 'NONE',  ( -2.287430849810337730, -285.7012486814879253, -201.9698130193444570 ) ) ;
#11161 = CARTESIAN_POINT ( 'NONE',  ( -95.73502178914699812, -289.5805541775005167, -225.2317439257451213 ) ) ;
#11162 = CYLINDRICAL_SURFACE ( 'NONE', #16418, 0.5000000000000004441 ) ;
#11163 = CARTESIAN_POINT ( 'NONE',  ( 25.79069818050878737, -274.7507879289541393, -307.9848307317479907 ) ) ;
#11164 = CARTESIAN_POINT ( 'NONE',  ( 17.98560915142196137, -292.3882150695460496, -319.8752689016915269 ) ) ;
#11165 = CARTESIAN_POINT ( 'NONE',  ( -22.78264641048746597, -118.9815703160634541, 22.50000000000000000 ) ) ;
#11166 = CARTESIAN_POINT ( 'NONE',  ( 191.4749582765727212, -21.37379927922774314, 13.00000000000000178 ) ) ;
#11167 = CARTESIAN_POINT ( 'NONE',  ( -27.91536765317002988, -290.6495020049017626, -194.5857227514489125 ) ) ;
#11168 = CARTESIAN_POINT ( 'NONE',  ( -73.97020223445493059, -287.1571125274352312, -206.2778005892703845 ) ) ;
#11169 = CARTESIAN_POINT ( 'NONE',  ( 0.1988940112167022212, -286.7996880825637618, -336.4862777388386803 ) ) ;
#11170 = CARTESIAN_POINT ( 'NONE',  ( -62.78348526920450468, -287.1397898224032588, -201.2554080310264055 ) ) ;
#11171 = DIRECTION ( 'NONE',  ( -1.000000000000000000, -0.000000000000000000, 0.000000000000000000 ) ) ;
#11172 = CARTESIAN_POINT ( 'NONE',  ( -54.80477001058553554, -286.6248540998305998, -199.2619370136571604 ) ) ;
#11173 = CARTESIAN_POINT ( 'NONE',  ( 36.46481204283844590, -295.7262723003140081, -285.5599852940453047 ) ) ;
#11174 = CARTESIAN_POINT ( 'NONE',  ( -107.3319585571128414, -276.2635152955796229, -298.8335242858804008 ) ) ;
#11175 = CARTESIAN_POINT ( 'NONE',  ( -114.3567419237675580, -278.9057259920187448, -268.7389283780404412 ) ) ;
#11176 = VECTOR ( 'NONE', #86013, 1000.000000000000000 ) ;
#11177 = CARTESIAN_POINT ( 'NONE',  ( -76.40349984469487765, -289.6143601046818503, -205.6208816450483141 ) ) ;
#11178 = CARTESIAN_POINT ( 'NONE',  ( -107.5761041906091435, -278.1476022556817043, -302.0523627193825860 ) ) ;
#11179 = CARTESIAN_POINT ( 'NONE',  ( 98.12082082284621265, -301.7359631804335436, -195.6703527335122601 ) ) ;
#11180 = CARTESIAN_POINT ( 'NONE',  ( -48.18343439339133027, -257.8434817577961553, -488.9450021219734595 ) ) ;
#11181 = CARTESIAN_POINT ( 'NONE',  ( 150.6539576904058606, 293.9636489450775230, 9.103929867429224387 ) ) ;
#11182 = CARTESIAN_POINT ( 'NONE',  ( -104.2544786422812138, -276.2626393102725615, -302.6289431065487747 ) ) ;
#11183 = CARTESIAN_POINT ( 'NONE',  ( 37.28529038273786966, -279.6543336527219026, -278.3319625602289875 ) ) ;
#11184 = DIRECTION ( 'NONE',  ( 0.000000000000000000, 1.000000000000000000, 0.000000000000000000 ) ) ;
#11185 = CARTESIAN_POINT ( 'NONE',  ( -9.483136583787503682, -275.1744817237452594, -341.4006013002754685 ) ) ;
#11186 = CARTESIAN_POINT ( 'NONE',  ( -100.7532965277512318, -297.5600158377420712, -308.0072204082302960 ) ) ;
#11187 = CARTESIAN_POINT ( 'NONE',  ( -13.53101158818511962, -281.6704036963191697, -343.2620344406865911 ) ) ;
#11188 = CARTESIAN_POINT ( 'NONE',  ( -106.9341234464503714, -297.7970769889863618, -247.3901114819853149 ) ) ;
#11189 = CARTESIAN_POINT ( 'NONE',  ( -97.85428625583519135, -298.4965165734280390, -223.5262396483698240 ) ) ;
#11190 = CARTESIAN_POINT ( 'NONE',  ( -71.91399351379897098, -273.2488685131103239, -205.9864766387333930 ) ) ;
#11191 = CARTESIAN_POINT ( 'NONE',  ( -1.505615463905816354, -294.5273562414528215, -204.4619727063512471 ) ) ;
#11192 = CARTESIAN_POINT ( 'NONE',  ( 39.34763579612192075, -287.8052487256001655, -277.2709486604872495 ) ) ;
#11193 = CARTESIAN_POINT ( 'NONE',  ( 34.02929029170060460, -274.0196506963127376, -295.9417315768594108 ) ) ;
#11194 = CARTESIAN_POINT ( 'NONE',  ( -60.02930083976117714, -289.1716111294249458, -343.9428601366946623 ) ) ;
#11195 = EDGE_CURVE ( 'NONE', #13726, #23799, #50419, .T. ) ;
#11196 = CARTESIAN_POINT ( 'NONE',  ( 34.98972816454642754, -286.7627752598561983, -281.9114786876830863 ) ) ;
#11197 = CARTESIAN_POINT ( 'NONE',  ( -106.5125022705141475, -288.9305696947652677, -241.3714512539633859 ) ) ;
#11198 = VERTEX_POINT ( 'NONE', #50425 ) ;
#11199 = CARTESIAN_POINT ( 'NONE',  ( -104.9628119525177112, -256.0684274861638983, -326.9234398911233939 ) ) ;
#11200 = CIRCLE ( 'NONE', #82306, 4.025000000000000355 ) ;
#11201 = CARTESIAN_POINT ( 'NONE',  ( 34.58116575261266235, -287.2291563452496916, -283.2098457517813017 ) ) ;
#11202 = FACE_OUTER_BOUND ( 'NONE', #10646, .T. ) ;
#11203 = CARTESIAN_POINT ( 'NONE',  ( -112.1332027681788759, -285.7103376914195678, -253.0680168422167355 ) ) ;
#11204 = CARTESIAN_POINT ( 'NONE',  ( 37.53447219344495522, -292.3979470227529305, -253.3794029679523021 ) ) ;
#11205 = CARTESIAN_POINT ( 'NONE',  ( 20.44595780854720246, -282.4745828335325086, -220.6721084005253601 ) ) ;
#11206 = CARTESIAN_POINT ( 'NONE',  ( 28.85147717333750350, -282.3651916689637460, -231.9975734320101708 ) ) ;
#11207 = CARTESIAN_POINT ( 'NONE',  ( -16.13452854233381117, -282.6034857096240103, -340.2127885268016598 ) ) ;
#11208 = CARTESIAN_POINT ( 'NONE',  ( 30.98655835208749210, -277.9579614454664807, -301.2844059510375132 ) ) ;
#11209 = CARTESIAN_POINT ( 'NONE',  ( -112.8886848000154401, -296.7391954051330458, -255.4052924458295024 ) ) ;
#11210 = CIRCLE ( 'NONE', #91283, 0.5000000000000004441 ) ;
#11211 = CARTESIAN_POINT ( 'NONE',  ( -96.68945355043678092, -274.4712446624611175, -226.9280982618618623 ) ) ;
#11212 = CARTESIAN_POINT ( 'NONE',  ( -111.8866982839125797, -288.6335967337550983, -265.6062723070377274 ) ) ;
#11213 = CARTESIAN_POINT ( 'NONE',  ( -108.3201243057135343, -271.5948065558897611, -251.4796499309283035 ) ) ;
#11214 = ORIENTED_EDGE ( 'NONE', *, *, #3119, .F. ) ;
#11215 = DIRECTION ( 'NONE',  ( 1.000000000000000000, 0.000000000000000000, 0.000000000000000000 ) ) ;
#11216 = CARTESIAN_POINT ( 'NONE',  ( -111.3005844235002542, -286.3572657036031615, -279.2541925294103748 ) ) ;
#11218 =( BOUNDED_CURVE ( )  B_SPLINE_CURVE ( 2, ( #17928, #39667, #68589, #83239, #33521, #56255, #70929, #19323, #12217, #18386, #84638, #12708, #48658, #18868, #27366, #54828, #26432, #47243, #90787, #69515, #19787, #83706, #91746, #54365, #5600, #62910, #48185, #25947, #76155, #33061, #55325, #40601, #69989, #4187, #4646, #47725, #55785, #41548, #34932, #20265, #5129, #84175, #76625, #77559, #34006, #11288, #91268, #34474, #26897, #11748, #70472, #61950, #42013, #62427, #63380, #41063, #92210, #77086, #69058, #78038, #85115, #49141, #13178, #6060, #63847, #25486, #40142, #14572, #92679, #57198, #346, #6996, #22127, #50995, #42486, #27849, #79880, #56738, #71399, #42969, #20731, #58586, #15020, #78497, #85584, #71874, #29703, #43428, #49601, #13635, #72323, #86499, #87425, #7444, #43880, #6532, #36326, #22573, #35408, #35868, #51447, #64328, #50059, #28768, #64785, #65240, #78955, #57651, #7901, #29233, #58128, #93154, #72776, #80336, #28309, #21662, #86039, #36790, #86973, #21188, #14105, #93610, #50538 ),
 .UNSPECIFIED., .F., .F. ) 
 B_SPLINE_CURVE_WITH_KNOTS ( ( 3, 2, 2, 2, 2, 2, 2, 2, 2, 2, 2, 2, 2, 2, 2, 2, 2, 2, 2, 2, 2, 2, 2, 2, 2, 2, 2, 2, 2, 2, 2, 2, 2, 2, 2, 2, 2, 2, 2, 2, 2, 2, 2, 2, 2, 2, 2, 2, 2, 2, 2, 2, 2, 2, 2, 2, 2, 2, 2, 2, 2, 3 ),
 ( -0.05135551144988959038, 0.000000000000000000, 0.01428571428571429047, 0.02857142857142856707, 0.04285714285714285754, 0.05714285714285713413, 0.07142857142857142461, 0.08571428571428571508, 0.1000000000000000056, 0.1142857142857142405, 0.1285714285714285587, 0.1428571428571428492, 0.1571428571428571397, 0.1714285714285714302, 0.1857142857142857206, 0.2000000000000000111, 0.2142857142857143016, 0.2285714285714285365, 0.2428571428571429380, 0.2571428571428571175, 0.2714285714285713524, 0.2857142857142856984, 0.2999999999999999889, 0.3142857142857142794, 0.3285714285714285698, 0.3428571428571428603, 0.3571428571428571508, 0.3714285714285714413, 0.3857142857142857317, 0.4000000000000000222, 0.4142857142857143127, 0.4285714285714285476, 0.4428571428571428381, 0.4571428571428570731, 0.4714285714285714191, 0.4857142857142857650, 0.5000000000000000000, 0.5142857142857142350, 0.5285714285714285809, 0.5428571428571428159, 0.5571428571428571619, 0.5714285714285713969, 0.5857142857142857428, 0.5999999999999999778, 0.6142857142857143238, 0.6285714285714285587, 0.6428571428571429047, 0.6571428571428571397, 0.6714285714285713746, 0.6857142857142857206, 0.6999999999999999556, 0.7142857142857143016, 0.7285714285714285365, 0.7428571428571428825, 0.7571428571428571175, 0.7714285714285714635, 0.7857142857142856984, 0.8000000000000000444, 0.8142857142857142794, 0.8285714285714287364, 0.8428571428571428603, 0.8500000000000000888 ),
 .UNSPECIFIED. ) 
 CURVE ( )  GEOMETRIC_REPRESENTATION_ITEM ( )  RATIONAL_B_SPLINE_CURVE ( ( 1.000000000000000000, 1.000000000000000000, 1.000000000000000000, 0.9749279121818236193, 1.000000000000000000, 0.9749279121818236193, 1.000000000000000000, 0.9749279121818236193, 1.000000000000000000, 0.9749279121818236193, 1.000000000000000000, 0.9749279121818236193, 1.000000000000000000, 0.9749279121818236193, 1.000000000000000000, 0.9749279121818236193, 1.000000000000000000, 0.9749279121818236193, 1.000000000000000000, 0.9749279121818236193, 1.000000000000000000, 0.9749279121818236193, 1.000000000000000000, 0.9749279121818236193, 1.000000000000000000, 0.9749279121818236193, 1.000000000000000000, 0.9749279121818236193, 1.000000000000000000, 0.9749279121818236193, 1.000000000000000000, 0.9749279121818236193, 1.000000000000000000, 0.9749279121818236193, 1.000000000000000000, 0.9749279121818236193, 1.000000000000000000, 0.9749279121818236193, 1.000000000000000000, 0.9749279121818236193, 1.000000000000000000, 0.9749279121818236193, 1.000000000000000000, 0.9749279121818236193, 1.000000000000000000, 0.9749279121818236193, 1.000000000000000000, 0.9749279121818236193, 1.000000000000000000, 0.9749279121818236193, 1.000000000000000000, 0.9749279121818236193, 1.000000000000000000, 0.9749279121818236193, 1.000000000000000000, 0.9749279121818236193, 1.000000000000000000, 0.9749279121818236193, 1.000000000000000000, 0.9749279121818236193, 1.000000000000000000, 0.9749279121818236193, 1.000000000000000000, 0.9749279121818236193, 1.000000000000000000, 0.9749279121818236193, 1.000000000000000000, 0.9749279121818236193, 1.000000000000000000, 0.9749279121818236193, 1.000000000000000000, 0.9749279121818236193, 1.000000000000000000, 0.9749279121818236193, 1.000000000000000000, 0.9749279121818236193, 1.000000000000000000, 0.9749279121818236193, 1.000000000000000000, 0.9749279121818236193, 1.000000000000000000, 0.9749279121818236193, 1.000000000000000000, 0.9749279121818236193, 1.000000000000000000, 0.9749279121818236193, 1.000000000000000000, 0.9749279121818236193, 1.000000000000000000, 0.9749279121818236193, 1.000000000000000000, 0.9749279121818236193, 1.000000000000000000, 0.9749279121818236193, 1.000000000000000000, 0.9749279121818236193, 1.000000000000000000, 0.9749279121818236193, 1.000000000000000000, 0.9749279121818236193, 1.000000000000000000, 0.9749279121818236193, 1.000000000000000000, 0.9749279121818236193, 1.000000000000000000, 0.9749279121818236193, 1.000000000000000000, 0.9749279121818236193, 1.000000000000000000, 0.9749279121818236193, 1.000000000000000000, 0.9749279121818236193, 1.000000000000000000, 0.9749279121818236193, 1.000000000000000000, 0.9749279121818236193, 1.000000000000000000, 0.9749279121818236193, 1.000000000000000000, 0.9749279121818236193, 1.000000000000000000, 0.9874639560909115321, 0.9874639560909117542 ) ) 
 REPRESENTATION_ITEM ( '' )  );
#11217 = VECTOR ( 'NONE', #42131, 1000.000000000000000 ) ;
#11219 = CARTESIAN_POINT ( 'NONE',  ( 1.624269386226377510, -295.6235624648946896, -336.4152301141319867 ) ) ;
#11220 = AXIS2_PLACEMENT_3D ( 'NONE', #68307, #26618, #10064 ) ;
#11221 = CARTESIAN_POINT ( 'NONE',  ( -95.99858010412029330, -284.5924704743349594, -313.9875216841513179 ) ) ;
#11222 = CARTESIAN_POINT ( 'NONE',  ( 12.54259940834403686, -275.4351481904558909, -328.7081562284523670 ) ) ;
#11223 = CARTESIAN_POINT ( 'NONE',  ( -58.91804095993250456, -292.4315309027696230, -196.5520785455045996 ) ) ;
#11224 = CARTESIAN_POINT ( 'NONE',  ( -105.5565534029861539, -283.1216778404532306, -237.3908393902971170 ) ) ;
#11225 = CARTESIAN_POINT ( 'NONE',  ( -56.18771979708773046, -292.1492153310924778, -195.6699206426692399 ) ) ;
#11226 = CARTESIAN_POINT ( 'NONE',  ( -110.3272207071332929, -290.8385778176651684, -273.9142166232599038 ) ) ;
#11227 = DIRECTION ( 'NONE',  ( -1.000000000000000000, 0.000000000000000000, 0.000000000000000000 ) ) ;
#11228 = CIRCLE ( 'NONE', #12737, 4.000000000000003553 ) ;
#11229 = FACE_OUTER_BOUND ( 'NONE', #45322, .T. ) ;
#11230 = CARTESIAN_POINT ( 'NONE',  ( -38.49763412114499062, -140.3826428618228590, -361.0438956898904621 ) ) ;
#11231 = CARTESIAN_POINT ( 'NONE',  ( -112.9099497434466457, -285.9339238109115513, -281.3236272611336517 ) ) ;
#11232 = CARTESIAN_POINT ( 'NONE',  ( -54.49178911615187104, -292.7666405000204009, -345.3538533559490702 ) ) ;
#11233 = ORIENTED_EDGE ( 'NONE', *, *, #64718, .F. ) ;
#11234 = CARTESIAN_POINT ( 'NONE',  ( -3.490821103498019884, -281.5146541893625454, -335.4008997861424746 ) ) ;
#11235 = CARTESIAN_POINT ( 'NONE',  ( 24.34816871883806755, -275.8315699416610300, -316.4057091225723184 ) ) ;
#11236 = CARTESIAN_POINT ( 'NONE',  ( -108.1884511879738824, -280.8665737776762512, -246.1027318723067765 ) ) ;
#11237 = CARTESIAN_POINT ( 'NONE',  ( 181.6399435233035149, 251.7122595193576728, -165.5316943122344071 ) ) ;
#11238 = CARTESIAN_POINT ( 'NONE',  ( -81.23801407186208223, -282.2103034980410712, -332.9692416852994370 ) ) ;
#11239 = CARTESIAN_POINT ( 'NONE',  ( -109.6935897988081621, -282.3352877322018344, -288.7200631314100860 ) ) ;
#11240 = CARTESIAN_POINT ( 'NONE',  ( 52.07892576469384949, -300.9172225385302113, -194.3480566079236382 ) ) ;
#11241 = AXIS2_PLACEMENT_3D ( 'NONE', #77241, #62588, #91431 ) ;
#11242 = CARTESIAN_POINT ( 'NONE',  ( -50.47612140227846567, -295.7167720108961362, -342.2323599314181592 ) ) ;
#11243 = VERTEX_POINT ( 'NONE', #63265 ) ;
#11244 = CARTESIAN_POINT ( 'NONE',  ( 35.39821468066580934, -292.0994536180252794, -259.8659633004283478 ) ) ;
#11245 = CARTESIAN_POINT ( 'NONE',  ( 38.63635908846916323, -276.3562667224822462, -282.5550258268467587 ) ) ;
#11246 = CARTESIAN_POINT ( 'NONE',  ( -31.33971031512739103, -274.1300316492268507, -197.5956257076479119 ) ) ;
#11247 = CARTESIAN_POINT ( 'NONE',  ( 11.59904624462071432, -273.6330006578010625, -211.2472377990444556 ) ) ;
#11248 = CARTESIAN_POINT ( 'NONE',  ( 165.4421947725420523, 275.5000000000000568, 22.46007009812167254 ) ) ;
#11249 = CARTESIAN_POINT ( 'NONE',  ( -5.483631870131095987, -272.4710459953950590, -202.4497445252075067 ) ) ;
#11250 = CARTESIAN_POINT ( 'NONE',  ( 152.9190334681021000, 20.54289017631687742, 11.30277777986246335 ) ) ;
#11251 = CARTESIAN_POINT ( 'NONE',  ( -43.30935424508157183, -271.8540379715383324, -505.8138214194312923 ) ) ;
#11252 = CARTESIAN_POINT ( 'NONE',  ( 22.07049152028501382, -283.2303133990907327, -313.3292992823072609 ) ) ;
#11253 = CARTESIAN_POINT ( 'NONE',  ( 30.18700024344522248, -283.7673574052660683, -305.2014485994206439 ) ) ;
#11254 = CARTESIAN_POINT ( 'NONE',  ( -104.6882332572437235, -284.2833620694008800, -241.7997736497220842 ) ) ;
#11255 = CARTESIAN_POINT ( 'NONE',  ( -76.80059102335336263, -275.9895532070642616, -332.7865749132354836 ) ) ;
#11256 = CARTESIAN_POINT ( 'NONE',  ( -43.00388115797979083, -284.9846585319517658, -344.4310038557687221 ) ) ;
#11257 = CARTESIAN_POINT ( 'NONE',  ( -85.57350775601103976, -276.2131403585453882, -326.1458772527687984 ) ) ;
#11258 = EDGE_CURVE ( 'NONE', #26346, #69103, #36834, .T. ) ;
#11259 = CARTESIAN_POINT ( 'NONE',  ( -19.20840370434564548, -275.3705625465728986, -199.2774243313589579 ) ) ;
#11260 = EDGE_CURVE ( 'NONE', #35472, #42154, #551, .T. ) ;
#11261 = CARTESIAN_POINT ( 'NONE',  ( 194.5337174367984687, 40.88867648032507418, 14.26073298213507812 ) ) ;
#11262 = CARTESIAN_POINT ( 'NONE',  ( -113.8840200522656971, -279.4467421975192565, -263.0395027813385127 ) ) ;
#11263 = EDGE_LOOP ( 'NONE', ( #75878, #62352 ) ) ;
#11264 = ORIENTED_EDGE ( 'NONE', *, *, #39673, .F. ) ;
#11265 = DIRECTION ( 'NONE',  ( -0.000000000000000000, -1.000000000000000000, -0.000000000000000000 ) ) ;
#11266 = CARTESIAN_POINT ( 'NONE',  ( -112.3726856812481856, -286.2741628816356751, -281.2502084701395120 ) ) ;
#11267 = CARTESIAN_POINT ( 'NONE',  ( -0.6858837335020224746, -293.7493308390761513, -333.7352271971253117 ) ) ;
#11268 = CARTESIAN_POINT ( 'NONE',  ( -102.2197270515946883, -289.3578092508161603, -311.7405282011702070 ) ) ;
#11269 = CARTESIAN_POINT ( 'NONE',  ( 34.99636457891098473, -285.9964633386975947, -286.0786469452647793 ) ) ;
#11271 = CARTESIAN_POINT ( 'NONE',  ( -63.13313071697616863, -289.9514142737637030, -200.9869432382342609 ) ) ;
#11270 = CARTESIAN_POINT ( 'NONE',  ( -42.69905825203463934, -284.5579945653087748, -196.9544286588893556 ) ) ;
#11272 = CARTESIAN_POINT ( 'NONE',  ( -64.18638933987271855, -284.6154590157877919, -338.6728531838838308 ) ) ;
#11273 = CARTESIAN_POINT ( 'NONE',  ( 37.32873527455178930, -273.4550046209459424, -262.8077666946611544 ) ) ;
#11274 = CARTESIAN_POINT ( 'NONE',  ( 24.07073671188498309, -285.3465645313724508, -225.2506644459180052 ) ) ;
#11275 = CARTESIAN_POINT ( 'NONE',  ( -35.55779474766005421, -300.0746396841030901, -195.3605010756353408 ) ) ;
#11276 = CARTESIAN_POINT ( 'NONE',  ( 24.33251116992141760, -286.1347439301002282, -313.4192726471200672 ) ) ;
#11277 = CARTESIAN_POINT ( 'NONE',  ( -35.66940553494461597, -281.0148643754564546, -197.1324754626337210 ) ) ;
#11278 = CARTESIAN_POINT ( 'NONE',  ( -84.00610051449423565, -291.6913500165445043, -329.3551105709826174 ) ) ;
#11279 = DIRECTION ( 'NONE',  ( 0.000000000000000000, 0.000000000000000000, 1.000000000000000000 ) ) ;
#11280 = CARTESIAN_POINT ( 'NONE',  ( -147.0026986695707762, 31.65052214425332622, -22.50000000000000000 ) ) ;
#11281 = CARTESIAN_POINT ( 'NONE',  ( -52.96712810417530903, -297.1709372653128298, -344.3413590588211832 ) ) ;
#11282 = CARTESIAN_POINT ( 'NONE',  ( -13.65368674449415920, -278.3593261084973278, -199.1452728415090974 ) ) ;
#11283 = CARTESIAN_POINT ( 'NONE',  ( -68.25440222016531777, -290.8535520384341453, -200.0007541048808264 ) ) ;
#11284 = CARTESIAN_POINT ( 'NONE',  ( -97.85085635573823026, -294.3693145329717140, -312.6113538220226928 ) ) ;
#11285 = CARTESIAN_POINT ( 'NONE',  ( 34.24452696001080199, -280.0190287886448459, -253.7281515909492384 ) ) ;
#11286 = CARTESIAN_POINT ( 'NONE',  ( -3.427220608014195591, -272.5832734608253531, -204.0812626408091148 ) ) ;
#11287 = CARTESIAN_POINT ( 'NONE',  ( 36.13569879432272103, -294.9083761019044232, -273.4933972702096980 ) ) ;
#11288 = CARTESIAN_POINT ( 'NONE',  ( -20.19161114001083490, -291.3376638359845288, -345.3538533559490702 ) ) ;
#11289 = CARTESIAN_POINT ( 'NONE',  ( -101.0600855105126072, -294.4739017096634939, -312.4409384456258181 ) ) ;
#11290 = CARTESIAN_POINT ( 'NONE',  ( 38.22679833462696308, -291.8990209280674435, -278.8048312412259406 ) ) ;
#11291 = VECTOR ( 'NONE', #52517, 1000.000000000000000 ) ;
#11292 = CARTESIAN_POINT ( 'NONE',  ( -38.92833475056011849, -293.4571351699126467, -196.7889934427387857 ) ) ;
#11293 = CARTESIAN_POINT ( 'NONE',  ( 199.0061125298537377, 275.0000000000000568, -7.725424859374024678 ) ) ;
#11294 = CARTESIAN_POINT ( 'NONE',  ( 30.73957360934411653, -294.7140600771061827, -297.2867503812493624 ) ) ;
#11295 = DIRECTION ( 'NONE',  ( 0.000000000000000000, 1.000000000000000000, 0.000000000000000000 ) ) ;
#11297 = CARTESIAN_POINT ( 'NONE',  ( 10.29152059668689922, -294.3730051613461001, -325.6790742299260728 ) ) ;
#11296 = CARTESIAN_POINT ( 'NONE',  ( -4.895389037928816300, -280.6471767272557258, -338.3873798393946117 ) ) ;
#11298 = CARTESIAN_POINT ( 'NONE',  ( 15.75353287994514240, -282.3249805648094366, -326.1275615828414516 ) ) ;
#11299 = CARTESIAN_POINT ( 'NONE',  ( -69.18158589412249171, -283.1263464489459807, -340.4609476158051962 ) ) ;
#11300 = CARTESIAN_POINT ( 'NONE',  ( -81.50960561043548580, -287.6540168513712388, -330.8344276423498513 ) ) ;
#11301 = CARTESIAN_POINT ( 'NONE',  ( 156.4851178187871312, 1.000000000000000000, 10.00000000000000000 ) ) ;
#11302 = CARTESIAN_POINT ( 'NONE',  ( 21.97200015200688838, -280.6818441227378003, -318.3879005566156479 ) ) ;
#11303 = CIRCLE ( 'NONE', #85390, 8.000000000000000000 ) ;
#11304 = CARTESIAN_POINT ( 'NONE',  ( -31.86264499555948504, -287.9050084939606222, -346.9083810122533578 ) ) ;
#11305 = FACE_OUTER_BOUND ( 'NONE', #69939, .T. ) ;
#11306 = CARTESIAN_POINT ( 'NONE',  ( -38.33281831385887983, -296.6649102561964355, -344.1544652583818333 ) ) ;
#11307 = CARTESIAN_POINT ( 'NONE',  ( -1.726156742267933364, -278.0148366805206024, -337.9639238675458728 ) ) ;
#11308 = CARTESIAN_POINT ( 'NONE',  ( -109.6421324285941807, -278.3584588987321808, -259.7764014511412825 ) ) ;
#11309 = CARTESIAN_POINT ( 'NONE',  ( 35.45191640392692989, -293.4006018236302680, -245.0981516801702469 ) ) ;
#11310 = UNCERTAINTY_MEASURE_WITH_UNIT (LENGTH_MEASURE( 1.000000000000000082E-05 ), #27421, 'distance_accuracy_value', 'NONE');
#11311 = CARTESIAN_POINT ( 'NONE',  ( -11.22317909835527239, -280.7944196730981048, -341.3190038640871080 ) ) ;
#11312 = CARTESIAN_POINT ( 'NONE',  ( -7.162368059646126994, -291.5168249590747109, -203.6331900611855019 ) ) ;
#11313 = CARTESIAN_POINT ( 'NONE',  ( -112.3093488958750612, -294.5976597207110217, -266.8040562119289802 ) ) ;
#11314 = ORIENTED_EDGE ( 'NONE', *, *, #62646, .T. ) ;
#11315 = DIRECTION ( 'NONE',  ( 0.000000000000000000, 1.000000000000000000, 0.000000000000000000 ) ) ;
#11316 = CARTESIAN_POINT ( 'NONE',  ( -20.84036663345083085, -294.3423741473930022, -341.5869574905818808 ) ) ;
#11317 = DIRECTION ( 'NONE',  ( 0.000000000000000000, 0.000000000000000000, -1.000000000000000000 ) ) ;
#11318 = CARTESIAN_POINT ( 'NONE',  ( 34.45848030099739390, -291.0523547857347353, -270.3937649182068412 ) ) ;
#11319 = CARTESIAN_POINT ( 'NONE',  ( -9.205420001057850854, -297.4550882046272022, -193.6007765762892916 ) ) ;
#11320 = CARTESIAN_POINT ( 'NONE',  ( 35.28768738530330040, -279.9688531837792311, -292.1117000145759448 ) ) ;
#11321 = CARTESIAN_POINT ( 'NONE',  ( 0.02818890718441586715, -287.8538985787386650, -203.5869766456557386 ) ) ;
#11322 = CARTESIAN_POINT ( 'NONE',  ( 5.842915620406163413, -288.2818276730639013, -329.2806252334829651 ) ) ;
#11323 = CARTESIAN_POINT ( 'NONE',  ( -79.00821737978208148, -279.1450924438626657, -331.2065406280355546 ) ) ;
#11324 = CARTESIAN_POINT ( 'NONE',  ( -37.85168605816453891, -299.8058200165792186, -196.3495382743187179 ) ) ;
#11325 = CARTESIAN_POINT ( 'NONE',  ( -108.5610877620571983, -277.1135405807749521, -288.1592224866163860 ) ) ;
#11326 = VERTEX_POINT ( 'NONE', #65136 ) ;
#11327 = CARTESIAN_POINT ( 'NONE',  ( -110.1011692115127261, -272.7031827280777065, -245.1607278428051586 ) ) ;
#11328 = CARTESIAN_POINT ( 'NONE',  ( -110.8370009187345602, -292.3183412605241074, -282.2629316736753253 ) ) ;
#11329 = CARTESIAN_POINT ( 'NONE',  ( 10.70979577105156011, -296.0011728215579296, -329.5687454362955577 ) ) ;
#11330 = DIRECTION ( 'NONE',  ( 1.000000000000000000, 0.000000000000000000, 0.000000000000000000 ) ) ;
#11331 = CARTESIAN_POINT ( 'NONE',  ( -90.66143039088635192, -290.4842294239578564, -320.4440202816364831 ) ) ;
#11332 = CARTESIAN_POINT ( 'NONE',  ( -43.48485865067390677, -254.2615844090929045, -445.7244014337675253 ) ) ;
#11333 = CARTESIAN_POINT ( 'NONE',  ( -110.7000583586131199, -296.9128819636652565, -293.4673548077265082 ) ) ;
#11334 = CARTESIAN_POINT ( 'NONE',  ( -83.49484891535782083, -289.5669206786536733, -210.2101347911883806 ) ) ;
#11335 = CARTESIAN_POINT ( 'NONE',  ( -93.65018486062362513, -297.6018534989476620, -217.7943255906305922 ) ) ;
#11336 = CARTESIAN_POINT ( 'NONE',  ( 180.2288731078812702, 214.9910457053126720, -24.90909090909092782 ) ) ;
#11337 = CARTESIAN_POINT ( 'NONE',  ( 195.5071814400074572, 25.58662921606786256, 14.62325102173291924 ) ) ;
#11338 = CARTESIAN_POINT ( 'NONE',  ( -101.1152550013760276, -292.6291387553094410, -228.3658891274201892 ) ) ;
#11339 = CARTESIAN_POINT ( 'NONE',  ( 13.79469577742117714, -295.1948066931273615, -206.1857440867352693 ) ) ;
#11340 = CARTESIAN_POINT ( 'NONE',  ( -108.7272761255729847, -286.2619989184202041, -292.8139121584833902 ) ) ;
#11341 = CARTESIAN_POINT ( 'NONE',  ( -69.03645266834649874, -271.6342739652374121, -202.5571738175895860 ) ) ;
#11342 = CARTESIAN_POINT ( 'NONE',  ( -97.45849390208093155, -275.0761269559565676, -226.3745845701654389 ) ) ;
#11343 = CARTESIAN_POINT ( 'NONE',  ( -111.7772303698380654, -288.6214340210744353, -271.1772261372534558 ) ) ;
#11344 = CARTESIAN_POINT ( 'NONE',  ( -39.89717350363931558, -278.9443156487969873, -346.0956694798783246 ) ) ;
#11345 = ORIENTED_EDGE ( 'NONE', *, *, #83721, .F. ) ;
#11347 = CARTESIAN_POINT ( 'NONE',  ( 33.21414182896251788, -280.6478811249043019, -251.1882004953533283 ) ) ;
#11346 = CARTESIAN_POINT ( 'NONE',  ( 18.83610338561120656, -280.8908376603206989, -223.7256858430666853 ) ) ;
#11348 = CARTESIAN_POINT ( 'NONE',  ( -6.685583423570927941, -277.7387027321283313, -340.6725089521601149 ) ) ;
#11349 = CARTESIAN_POINT ( 'NONE',  ( -11.62811137551423535, -279.1745028002294475, -198.1471210626963568 ) ) ;
#11350 = AXIS2_PLACEMENT_3D ( 'NONE', #60580, #75240, #25502 ) ;
#11351 = CARTESIAN_POINT ( 'NONE',  ( 166.0636734013047260, 231.1879126283853907, -190.4032150769705822 ) ) ;
#11352 = CARTESIAN_POINT ( 'NONE',  ( -0.1699131758216758381, -275.4753885196952297, -203.1816090986692416 ) ) ;
#11353 = ITEM_DEFINED_TRANSFORMATION ( 'NONE', 'NONE', #64343,  #18940 ) ;
#11354 = CARTESIAN_POINT ( 'NONE',  ( -29.92569908550941093, -275.6645291668938853, -194.4156725579751992 ) ) ;
#11355 = CARTESIAN_POINT ( 'NONE',  ( -95.99890600148557951, -299.6948066931273615, -223.6242672951989618 ) ) ;
#11356 = ORIENTED_EDGE ( 'NONE', *, *, #21572, .F. ) ;
#11357 = CARTESIAN_POINT ( 'NONE',  ( 211.1232656141943949, 0.000000000000000000, 7.000000000000000000 ) ) ;
#11358 = CARTESIAN_POINT ( 'NONE',  ( 34.86946505646591987, -288.4620281699108659, -257.4349115767386138 ) ) ;
#11359 = CARTESIAN_POINT ( 'NONE',  ( 4.601412699341469015, -288.3695778352252432, -206.9364085998001883 ) ) ;
#11360 = CARTESIAN_POINT ( 'NONE',  ( -109.7250503732969804, -289.7648599649226071, -280.6756346987486381 ) ) ;
#11361 = AXIS2_PLACEMENT_3D ( 'NONE', #57143, #5068, #85984 ) ;
#11362 = CARTESIAN_POINT ( 'NONE',  ( 26.30998212857352669, -286.4892510101543621, -227.1173277260599548 ) ) ;
#11363 = CARTESIAN_POINT ( 'NONE',  ( 199.5287591260213560, 25.00736135706073426, 9.179409580711885397 ) ) ;
#11364 = CARTESIAN_POINT ( 'NONE',  ( 1.505277314044181525, -280.9238368440570639, -333.1691106938492908 ) ) ;
#11365 = CARTESIAN_POINT ( 'NONE',  ( -0.3558064006185132078, -290.4156692189535534, -334.7857317213698138 ) ) ;
#11366 = CARTESIAN_POINT ( 'NONE',  ( -85.32777244585830090, -282.2094553273086035, -326.2900426472295976 ) ) ;
#11367 = EDGE_CURVE ( 'NONE', #54755, #91019, #49495, .T. ) ;
#11368 = CARTESIAN_POINT ( 'NONE',  ( -110.8853594847917776, -279.8634613372489639, -270.6566394101948845 ) ) ;
#11369 = CARTESIAN_POINT ( 'NONE',  ( -18.99544303858672833, -277.3018856978719100, -341.0817181798996103 ) ) ;
#11370 = CARTESIAN_POINT ( 'NONE',  ( -109.0964789659408751, -289.6897383788099773, -243.3910039210418006 ) ) ;
#11371 = VECTOR ( 'NONE', #41606, 1000.000000000000000 ) ;
#11372 = CARTESIAN_POINT ( 'NONE',  ( -109.8283219981287857, -285.6772374939705514, -244.8689923333030265 ) ) ;
#11373 = CARTESIAN_POINT ( 'NONE',  ( -78.49484393398729765, -286.0062345702976927, -205.3538440969740861 ) ) ;
#11374 = CARTESIAN_POINT ( 'NONE',  ( 21.01118224543156998, -282.3349793459746593, -314.2445284700164621 ) ) ;
#11375 = VERTEX_POINT ( 'NONE', #48538 ) ;
#11376 = DIRECTION ( 'NONE',  ( 0.000000000000000000, 0.000000000000000000, -1.000000000000000000 ) ) ;
#11377 = CARTESIAN_POINT ( 'NONE',  ( -85.74245417775968292, -293.2512084317741596, -212.0034216803959737 ) ) ;
#11378 = CARTESIAN_POINT ( 'NONE',  ( 31.77725959581172077, -292.6614447000270047, -303.2849806446945422 ) ) ;
#11379 = CARTESIAN_POINT ( 'NONE',  ( -29.95425096144462529, -273.2066927464597939, -197.4993718956545194 ) ) ;
#11380 = CARTESIAN_POINT ( 'NONE',  ( -113.5527564093087278, -295.7674166560302638, -281.0075193327135707 ) ) ;
#11381 = CARTESIAN_POINT ( 'NONE',  ( -55.16144963479948871, -290.2986411969301344, -198.8547247155877074 ) ) ;
#11382 = CARTESIAN_POINT ( 'NONE',  ( -35.64961170260739465, -293.2705259172656156, -344.3677798217680674 ) ) ;
#11383 = CARTESIAN_POINT ( 'NONE',  ( -105.4759555427107358, -291.3922999811293266, -297.7894596594096583 ) ) ;
#11384 = CARTESIAN_POINT ( 'NONE',  ( 85.55100297371598117, -373.0521521680024648, -417.1172536214571096 ) ) ;
#11385 = CARTESIAN_POINT ( 'NONE',  ( 36.55020258979707393, -291.7294831565670279, -284.2151388565059733 ) ) ;
#11386 = CARTESIAN_POINT ( 'NONE',  ( -55.96901422286584449, -297.2920558577019960, -343.0641538239559054 ) ) ;
#11387 = CARTESIAN_POINT ( 'NONE',  ( -87.86546529836977015, -286.2657948846150475, -217.3445394364528909 ) ) ;
#11388 = CARTESIAN_POINT ( 'NONE',  ( 37.98597651331754577, -277.5060199872726798, -268.3244708241073226 ) ) ;
#11389 = CARTESIAN_POINT ( 'NONE',  ( -107.2202210201238017, -276.9427204500062203, -301.8749748085886040 ) ) ;
#11390 = CARTESIAN_POINT ( 'NONE',  ( -34.75589845781152576, -297.2809260219823386, -193.5229350376594084 ) ) ;
#11391 = CARTESIAN_POINT ( 'NONE',  ( 23.28315414248127624, -274.3770698639895613, -312.9061203951491166 ) ) ;
#11392 = CARTESIAN_POINT ( 'NONE',  ( -94.17406662523710281, -277.3022651727242192, -222.2645355134858960 ) ) ;
#11393 = CARTESIAN_POINT ( 'NONE',  ( -56.98255259209989276, -274.9983418301884512, -199.5877651041261345 ) ) ;
#11394 = CARTESIAN_POINT ( 'NONE',  ( -97.31204832372311841, -276.3170232525630468, -317.3717312079050430 ) ) ;
#11395 = CARTESIAN_POINT ( 'NONE',  ( 198.5086862847058171, 68.69963673589226971, 12.80442219776277213 ) ) ;
#11396 = CARTESIAN_POINT ( 'NONE',  ( -81.13870037973701699, -274.0908838076598499, -211.7679830997394959 ) ) ;
#11397 = DIRECTION ( 'NONE',  ( 0.000000000000000000, 1.000000000000000000, -1.224646799147353207E-16 ) ) ;
#11399 = CARTESIAN_POINT ( 'NONE',  ( -11.48823446740222032, -274.2317006526435534, -202.0384963232974940 ) ) ;
#11398 = CARTESIAN_POINT ( 'NONE',  ( -64.87016117494248135, -287.4298902250495189, -340.5631881141715667 ) ) ;
#11400 = CARTESIAN_POINT ( 'NONE',  ( 36.78441279345251758, -287.8138627200721089, -291.2498027762903234 ) ) ;
#11401 = CARTESIAN_POINT ( 'NONE',  ( -69.35238401008209053, -289.1286462285888206, -340.3831119873746047 ) ) ;
#11402 = CARTESIAN_POINT ( 'NONE',  ( -40.39932015838823531, -299.9939157610626239, -195.0169606266555036 ) ) ;
#11403 = CARTESIAN_POINT ( 'NONE',  ( 28.76599078492039396, -292.0193218058253137, -305.5403066563320635 ) ) ;
#11404 = CARTESIAN_POINT ( 'NONE',  ( 37.52249607088534589, -280.5317742177047649, -252.9968900744329972 ) ) ;
#11405 = CARTESIAN_POINT ( 'NONE',  ( 22.68542923180448057, -296.3033736090878278, -195.3865787154307441 ) ) ;
#11406 = CARTESIAN_POINT ( 'NONE',  ( -93.73448883533198739, -277.2394758535182291, -220.8395359513654057 ) ) ;
#11407 = DIRECTION ( 'NONE',  ( 1.000000000000000000, 2.720159063138535749E-15, 0.000000000000000000 ) ) ;
#11408 = CARTESIAN_POINT ( 'NONE',  ( 19.81307960487046316, -286.9946250090910667, -316.4095887485784147 ) ) ;
#11409 = CARTESIAN_POINT ( 'NONE',  ( 196.7383257810085979, 42.27872732282705925, 11.00000000000000000 ) ) ;
#11410 = CARTESIAN_POINT ( 'NONE',  ( 156.4851178187871312, 1.000000000000000000, 10.00000000000000000 ) ) ;
#11411 = CARTESIAN_POINT ( 'NONE',  ( -58.18703868680834290, -289.7827586610171693, -198.2618640257711604 ) ) ;
#11412 = CARTESIAN_POINT ( 'NONE',  ( 22.83592406990304013, -276.4838422028288960, -227.8026935853109762 ) ) ;
#11413 = CARTESIAN_POINT ( 'NONE',  ( 38.94217531313751834, -283.0434760568230104, -275.6022591515587692 ) ) ;
#11415 = CARTESIAN_POINT ( 'NONE',  ( -110.3187896272780932, -284.5089228646999118, -273.6381354138727033 ) ) ;
#11414 = CARTESIAN_POINT ( 'NONE',  ( -36.18977776368984678, -296.0866170971119686, -195.0062959027168006 ) ) ;
#11416 = CARTESIAN_POINT ( 'NONE',  ( 21.94520876119978681, -276.3714986951895867, -226.7671120568137439 ) ) ;
#11417 = CARTESIAN_POINT ( 'NONE',  ( 34.27732038458702135, -276.1574838319912146, -255.3561829670659620 ) ) ;
#11418 = CARTESIAN_POINT ( 'NONE',  ( -57.91307169582564285, -285.3178921301194464, -342.5388085858872387 ) ) ;
#11419 = CARTESIAN_POINT ( 'NONE',  ( -74.41789684930030546, -272.4672874572282240, -207.0600733800549165 ) ) ;
#11420 = ORIENTED_EDGE ( 'NONE', *, *, #11662, .T. ) ;
#11421 = CARTESIAN_POINT ( 'NONE',  ( 202.9738562182569694, 291.9636489450776367, -53.99999999998589573 ) ) ;
#11422 = CARTESIAN_POINT ( 'NONE',  ( -24.90990485622979023, -294.7312330327834502, -346.4049884760342479 ) ) ;
#11423 = CARTESIAN_POINT ( 'NONE',  ( -110.3230030974495719, -286.3290913668477629, -286.0926037668029380 ) ) ;
#11424 = PLANE ( 'NONE',  #65478 ) ;
#11425 = CARTESIAN_POINT ( 'NONE',  ( 99.50465036329318025, -297.2649936051624309, -195.4191791630918829 ) ) ;
#11426 = CARTESIAN_POINT ( 'NONE',  ( -80.14473762126785061, -276.8124489957585865, -334.2378595661368195 ) ) ;
#11427 = CARTESIAN_POINT ( 'NONE',  ( -113.3165986411326571, -288.8698335051075219, -276.8648168246490968 ) ) ;
#11428 = CARTESIAN_POINT ( 'NONE',  ( -8.202442798970212223, -284.1835824435787572, -338.0487197718591688 ) ) ;
#11429 = AXIS2_PLACEMENT_3D ( 'NONE', #55746, #13141, #93571 ) ;
#11430 = CARTESIAN_POINT ( 'NONE',  ( -69.67412546411621577, -279.2438419996188941, -336.9528315824991864 ) ) ;
#11431 = CARTESIAN_POINT ( 'NONE',  ( -107.3932622177593004, -286.3709757065608414, -239.7101484561688949 ) ) ;
#11432 = CARTESIAN_POINT ( 'NONE',  ( 19.46310423882188445, -282.8732092315353839, -221.3698402362720117 ) ) ;
#11433 = CARTESIAN_POINT ( 'NONE',  ( 29.94649989121425193, -275.2323519110170764, -232.8175652762110985 ) ) ;
#11434 = CARTESIAN_POINT ( 'NONE',  ( -96.15056425276520713, -277.7156232632123647, -320.0857701678258991 ) ) ;
#11435 = ADVANCED_FACE ( 'NONE', ( #71766 ), #41903, .F. ) ;
#11436 = CARTESIAN_POINT ( 'NONE',  ( -108.2332687382704819, -298.1750230079541666, -293.2368349063028177 ) ) ;
#11437 = CARTESIAN_POINT ( 'NONE',  ( 175.2296996224750103, 275.0000000000000568, 0.000000000000000000 ) ) ;
#11438 = CARTESIAN_POINT ( 'NONE',  ( 139.6925840978351516, -0.9999999999999991118, 21.50000000000000000 ) ) ;
#11439 = CARTESIAN_POINT ( 'NONE',  ( 51.79982928851320878, -297.2963346967968619, -194.6241899864013192 ) ) ;
#11440 = CARTESIAN_POINT ( 'NONE',  ( 29.20774096101851924, -275.4658549147889062, -300.5134036702175990 ) ) ;
#11441 = CARTESIAN_POINT ( 'NONE',  ( -34.07718661552963368, -299.1717895042510236, -193.6696448167754454 ) ) ;
#11442 = CARTESIAN_POINT ( 'NONE',  ( -4.160082858052456700, -288.2559950131039841, -204.2025638000948504 ) ) ;
#11443 = CARTESIAN_POINT ( 'NONE',  ( -36.26464106556716160, -296.5590312381929721, -346.6731709522434812 ) ) ;
#11444 = CARTESIAN_POINT ( 'NONE',  ( -111.5800121149757160, -297.5190723850998324, -289.3000501851827835 ) ) ;
#11445 = CARTESIAN_POINT ( 'NONE',  ( -109.4866115917095897, -292.2938767789697749, -290.4299665183043544 ) ) ;
#11446 = CARTESIAN_POINT ( 'NONE',  ( -62.91204080322021497, -277.7184462700200243, -199.9773019534132743 ) ) ;
#11447 = CARTESIAN_POINT ( 'NONE',  ( -110.3034457167512414, -280.6640958970323254, -255.5356416199172145 ) ) ;
#11448 = CARTESIAN_POINT ( 'NONE',  ( -47.44444569349431617, -296.0027431062397341, -196.5576365706783406 ) ) ;
#11449 = CARTESIAN_POINT ( 'NONE',  ( -30.30563378287073562, -284.8244523437048201, -345.7985042736161745 ) ) ;
#11450 = CARTESIAN_POINT ( 'NONE',  ( 34.30100721949369813, -286.2683203468890838, -254.8192854472428053 ) ) ;
#11451 = CARTESIAN_POINT ( 'NONE',  ( -29.52244597877754373, -125.2720606855327645, -363.9572059679637164 ) ) ;
#11452 = EDGE_LOOP ( 'NONE', ( #70609, #72394, #40072, #5192 ) ) ;
#11453 = CARTESIAN_POINT ( 'NONE',  ( -39.97043042295008064, -285.6849327779158898, -197.3873058039590092 ) ) ;
#11454 = ORIENTED_EDGE ( 'NONE', *, *, #89540, .F. ) ;
#11455 = CARTESIAN_POINT ( 'NONE',  ( -58.38866193284027872, -284.3975512039889963, -344.1626984338965372 ) ) ;
#11456 = CARTESIAN_POINT ( 'NONE',  ( -74.28774443070166456, -273.8800120937729616, -207.3178043428175386 ) ) ;
#11457 = CARTESIAN_POINT ( 'NONE',  ( 37.63803112149120267, -286.1490916994732743, -254.6116087331639619 ) ) ;
#11458 = CARTESIAN_POINT ( 'NONE',  ( -19.82160859362019067, -281.2131800830991324, -195.5678616846588227 ) ) ;
#11459 = EDGE_CURVE ( 'NONE', #56922, #42812, #78843, .T. ) ;
#11460 = CARTESIAN_POINT ( 'NONE',  ( 186.6539576904058890, 293.9636489450775230, -11.60392986742922261 ) ) ;
#11461 = CARTESIAN_POINT ( 'NONE',  ( -95.39107686109805684, -280.7465174123743736, -220.8134983719806144 ) ) ;
#11462 = CARTESIAN_POINT ( 'NONE',  ( 12.97514498431736030, -281.0660220433105110, -212.1034198699930755 ) ) ;
#11463 = CARTESIAN_POINT ( 'NONE',  ( -6.941161984400256557, -283.9809262143061233, -207.3071070584150277 ) ) ;
#11464 = CARTESIAN_POINT ( 'NONE',  ( 85.12579728816612601, 83.07458439776537773, -302.4277712846086388 ) ) ;
#11465 = ORIENTED_EDGE ( 'NONE', *, *, #84689, .F. ) ;
#11466 = CARTESIAN_POINT ( 'NONE',  ( -27.06294769334709471, -276.1831539464841399, -196.1848865931888497 ) ) ;
#11467 = CARTESIAN_POINT ( 'NONE',  ( -84.62815394613997455, -219.0928880101756704, -352.2053832115043974 ) ) ;
#11468 = CARTESIAN_POINT ( 'NONE',  ( 20.97651499013447207, -278.9285694221537142, -223.7689234350514766 ) ) ;
#11469 = CARTESIAN_POINT ( 'NONE',  ( 35.72353641092399101, -295.0466737807587947, -249.4464324571203235 ) ) ;
#11470 = CARTESIAN_POINT ( 'NONE',  ( -107.7031715467910260, -295.6389931028600131, -290.1892799794342750 ) ) ;
#11471 = CARTESIAN_POINT ( 'NONE',  ( -4.624614936613887117, -291.9793798705346717, -200.7255003711733821 ) ) ;
#11472 = CARTESIAN_POINT ( 'NONE',  ( -104.9195836729377191, -260.6502345264863720, -315.6181490027343557 ) ) ;
#11474 = CARTESIAN_POINT ( 'NONE',  ( 36.07227124826489018, -285.8536498959455798, -262.8226021462563722 ) ) ;
#11473 = CARTESIAN_POINT ( 'NONE',  ( -111.0488184132014311, -295.3833861899994417, -250.0196381538110018 ) ) ;
#11475 = CARTESIAN_POINT ( 'NONE',  ( 18.01723649435033181, -296.1084460155602187, -319.8399065829707979 ) ) ;
#11476 = CARTESIAN_POINT ( 'NONE',  ( 32.74892890134105272, -285.9454472552562265, -248.2158515072573266 ) ) ;
#11477 = CARTESIAN_POINT ( 'NONE',  ( -90.02799977710412804, -286.6039323911152792, -219.0494396915206039 ) ) ;
#11478 = ORIENTED_EDGE ( 'NONE', *, *, #29868, .T. ) ;
#11479 = CARTESIAN_POINT ( 'NONE',  ( 38.58559150408168392, -294.6352542864493671, -281.6689293700790699 ) ) ;
#11480 = CARTESIAN_POINT ( 'NONE',  ( -1.216129416510071115, -283.0512547400093695, -333.8664845470268006 ) ) ;
#11481 = CARTESIAN_POINT ( 'NONE',  ( -92.42221285259176966, -294.6140288385988697, -323.5978143141338137 ) ) ;
#11482 = CARTESIAN_POINT ( 'NONE',  ( -106.3639559085468704, -290.9191095673795076, -304.2472036212384410 ) ) ;
#11483 = CARTESIAN_POINT ( 'NONE',  ( -4.636001466699962492, -292.9639148862775073, -200.7201517441747001 ) ) ;
#11484 = CARTESIAN_POINT ( 'NONE',  ( -39.95589968992072016, -289.2524614877446538, -343.3638723023991588 ) ) ;
#11485 = ORIENTED_EDGE ( 'NONE', *, *, #60783, .T. ) ;
#11486 = DIRECTION ( 'NONE',  ( -1.000000000000000000, 0.000000000000000000, 0.000000000000000000 ) ) ;
#11487 = CARTESIAN_POINT ( 'NONE',  ( -103.5123887959996409, -297.9251030542459375, -307.3701453069767808 ) ) ;
#11488 = CARTESIAN_POINT ( 'NONE',  ( 98.11687111328420485, -298.3994096029719003, -193.8837290502138160 ) ) ;
#11489 = ADVANCED_FACE ( 'NONE', ( #92096 ), #85229, .F. ) ;
#11490 = CARTESIAN_POINT ( 'NONE',  ( -5.445217454625628228, -279.5411907961400289, -204.4367458427530266 ) ) ;
#11491 = CARTESIAN_POINT ( 'NONE',  ( -5.134309819086812610, -273.9724995160595427, -200.4882984245600994 ) ) ;
#11492 = CARTESIAN_POINT ( 'NONE',  ( -69.54318831975241721, -296.1002413525507677, -204.0755847722494423 ) ) ;
#11493 = CARTESIAN_POINT ( 'NONE',  ( -81.53605894583266434, -279.5212305605182337, -330.0077786293063582 ) ) ;
#11494 = CARTESIAN_POINT ( 'NONE',  ( 36.83490362576873167, -273.7441626959432597, -274.4031117153029413 ) ) ;
#11495 = CARTESIAN_POINT ( 'NONE',  ( -6.584612420995379800, -295.8440838470920653, -337.0029371490374501 ) ) ;
#11496 = CARTESIAN_POINT ( 'NONE',  ( -105.0529562735668208, -298.0070062402089093, -242.2646437551103702 ) ) ;
#11497 = DIRECTION ( 'NONE',  ( 0.5729786897769424403, -5.686911123206802946E-15, -0.8195702660916258653 ) ) ;
#11498 = CARTESIAN_POINT ( 'NONE',  ( -113.3248288483426762, -298.2331975103411992, -263.9581772851617529 ) ) ;
#11499 = CARTESIAN_POINT ( 'NONE',  ( -36.53874163567517996, -296.0620253656962291, -195.1947156145810425 ) ) ;
#11500 = CARTESIAN_POINT ( 'NONE',  ( 14.39427520030632657, -294.9526403546959159, -322.0780313726114628 ) ) ;
#11501 = CARTESIAN_POINT ( 'NONE',  ( -104.0831550980230418, -289.5419824366031207, -239.3618743800400637 ) ) ;
#11502 = CARTESIAN_POINT ( 'NONE',  ( 140.6539576904058606, 276.0000000000000568, -12.00000000000000178 ) ) ;
#11503 = CARTESIAN_POINT ( 'NONE',  ( -3.858559478608783788, -274.9743928494764873, -201.0760927360696257 ) ) ;
#11504 = CARTESIAN_POINT ( 'NONE',  ( -35.15122092426700817, -298.4135995138944395, -197.3398456385576765 ) ) ;
#11505 = CARTESIAN_POINT ( 'NONE',  ( -6.113629538847954237, -284.6237049131701156, -338.9411035002154335 ) ) ;
#11506 = AXIS2_PLACEMENT_3D ( 'NONE', #48238, #84693, #79014 ) ;
#11507 = CARTESIAN_POINT ( 'NONE',  ( -35.92522793467507114, -281.7196016093114395, -346.8678886647937816 ) ) ;
#11508 = EDGE_CURVE ( 'NONE', #84479, #75355, #20146, .T. ) ;
#11509 = CARTESIAN_POINT ( 'NONE',  ( -41.38738884441230681, -276.4503954261335821, -347.1658790889136412 ) ) ;
#11510 = CARTESIAN_POINT ( 'NONE',  ( -67.86102795488912420, -282.6604924618716268, -336.8530149059919268 ) ) ;
#11511 = CARTESIAN_POINT ( 'NONE',  ( -14.01563164195555977, -280.7500629060195934, -341.8168592057301112 ) ) ;
#11512 = CARTESIAN_POINT ( 'NONE',  ( 33.43168896984582972, -273.8602827569240503, -250.0169715893742364 ) ) ;
#11513 = CARTESIAN_POINT ( 'NONE',  ( -59.57981250831698361, -279.3401748849400406, -342.0421395490499776 ) ) ;
#11514 = DIRECTION ( 'NONE',  ( 0.2456588035076310295, -0.9693563597868428694, 0.000000000000000000 ) ) ;
#11515 = FACE_OUTER_BOUND ( 'NONE', #28357, .T. ) ;
#11516 = CARTESIAN_POINT ( 'NONE',  ( -36.88163231859655156, -296.2977026140270596, -194.3745803279026916 ) ) ;
#11517 = CARTESIAN_POINT ( 'NONE',  ( -106.8278119566251831, -280.9255136185743709, -241.6956564145168329 ) ) ;
#11518 = DIRECTION ( 'NONE',  ( 0.4999999999999967248, 0.8660254037844404840, 0.000000000000000000 ) ) ;
#11519 = CARTESIAN_POINT ( 'NONE',  ( -112.9138559037067182, -286.4408799082561359, -272.8270985848679402 ) ) ;
#11520 = ORIENTED_EDGE ( 'NONE', *, *, #65065, .T. ) ;
#11521 = CARTESIAN_POINT ( 'NONE',  ( 158.6539576904058606, 293.9636489450775230, 0.000000000000000000 ) ) ;
#11522 = CARTESIAN_POINT ( 'NONE',  ( 12.56710903178727534, -286.3568403398864461, -326.4130420163684221 ) ) ;
#11523 = DIRECTION ( 'NONE',  ( 0.000000000000000000, 0.000000000000000000, 1.000000000000000000 ) ) ;
#11524 = CARTESIAN_POINT ( 'NONE',  ( -95.59490051737277838, -295.9720864045256121, -225.6898309268584626 ) ) ;
#11525 = CARTESIAN_POINT ( 'NONE',  ( -53.70344102723436208, -287.4039243361898457, -342.7707783337318119 ) ) ;
#11526 = CARTESIAN_POINT ( 'NONE',  ( -53.17117378510891967, -153.5335516589311737, -364.2630158522994179 ) ) ;
#11527 = CARTESIAN_POINT ( 'NONE',  ( -110.5494919696190408, -294.3427326947924030, -286.6589665262314952 ) ) ;
#11528 = CARTESIAN_POINT ( 'NONE',  ( -98.77442992329163474, -283.6398623706434137, -225.0113347756494022 ) ) ;
#11529 = CARTESIAN_POINT ( 'NONE',  ( 15.82168780366188088, -282.4204734350224157, -219.1012770998071346 ) ) ;
#11530 = CARTESIAN_POINT ( 'NONE',  ( -33.13751901158030222, -281.2397787458382936, -346.2443568781510521 ) ) ;
#11531 = CARTESIAN_POINT ( 'NONE',  ( -72.35886167263529956, -289.5293361712776914, -334.4142084416675402 ) ) ;
#11532 = CARTESIAN_POINT ( 'NONE',  ( -94.40887490260023185, -280.6297944397164770, -223.8991713785771651 ) ) ;
#11533 = CARTESIAN_POINT ( 'NONE',  ( -66.14266353455525405, -280.4681358479791129, -203.0934053111797937 ) ) ;
#11534 = CARTESIAN_POINT ( 'NONE',  ( 36.40842415022844847, -289.3335443232876401, -254.8285740615326915 ) ) ;
#11535 = ORIENTED_EDGE ( 'NONE', *, *, #36693, .F. ) ;
#11536 = CARTESIAN_POINT ( 'NONE',  ( -110.1018633137572920, -272.8698358982286436, -245.1627320581836500 ) ) ;
#11537 = CARTESIAN_POINT ( 'NONE',  ( -110.5469674573932366, -292.3429909457438498, -285.0152747344441764 ) ) ;
#11538 = DIRECTION ( 'NONE',  ( 0.000000000000000000, 0.000000000000000000, 1.000000000000000000 ) ) ;
#11539 = CARTESIAN_POINT ( 'NONE',  ( 25.22466315766300227, -290.6948066931273047, -320.2154176792147382 ) ) ;
#11540 = ORIENTED_EDGE ( 'NONE', *, *, #43526, .F. ) ;
#11541 = CARTESIAN_POINT ( 'NONE',  ( 0.1109106937538962556, -274.5550432051274470, -335.5916923982401840 ) ) ;
#11542 = CARTESIAN_POINT ( 'NONE',  ( 194.7510731661265595, 15.36528803885690664, 22.50000000000000000 ) ) ;
#11543 = CARTESIAN_POINT ( 'NONE',  ( -14.04619081289553506, -293.1547460610950111, -342.9128902544452444 ) ) ;
#11544 = CARTESIAN_POINT ( 'NONE',  ( -44.56893824619808697, -297.4660286304355736, -197.6074923732301443 ) ) ;
#11545 = CARTESIAN_POINT ( 'NONE',  ( -50.85983175033088344, -290.7479861537665329, -342.8561444416225186 ) ) ;
#11546 = CARTESIAN_POINT ( 'NONE',  ( -36.15511286537676483, -284.7972155504232887, -344.3649423895672612 ) ) ;
#11547 = CARTESIAN_POINT ( 'NONE',  ( -101.2015815193663144, -292.5343043824975666, -228.3075643155002581 ) ) ;
#11548 = CARTESIAN_POINT ( 'NONE',  ( -40.62810733174035249, -293.3268314184469432, -193.9117867469470582 ) ) ;
#11549 = CARTESIAN_POINT ( 'NONE',  ( -10.04516407786696952, -288.4086670894283770, -200.4909443072115494 ) ) ;
#11550 = CARTESIAN_POINT ( 'NONE',  ( 1.372136844239459919, -280.7207461174638183, -203.7403742711566395 ) ) ;
#11551 = CARTESIAN_POINT ( 'NONE',  ( -98.85080414034196394, -294.0386249543082613, -314.3348645217753869 ) ) ;
#11552 = CARTESIAN_POINT ( 'NONE',  ( 17.82479500166395781, -282.1226721011521477, -324.1556216165811861 ) ) ;
#11553 = CARTESIAN_POINT ( 'NONE',  ( 5.876947330639362477, -276.5050727388298810, -209.9402126790755290 ) ) ;
#11554 = CARTESIAN_POINT ( 'NONE',  ( -21.33282851196159058, -279.3376638359844719, -340.3538533559490702 ) ) ;
#11555 = CARTESIAN_POINT ( 'NONE',  ( -45.53989364634736603, -275.2944363086901376, -345.7332774168204423 ) ) ;
#11556 = CARTESIAN_POINT ( 'NONE',  ( 180.7149167944524493, 8.542400036368780647, -9.000000000000001776 ) ) ;
#11557 = CARTESIAN_POINT ( 'NONE',  ( 9.943755245608874915, -281.8879246674198384, -326.1239116657922636 ) ) ;
#11558 = CARTESIAN_POINT ( 'NONE',  ( -31.46533377740031412, -278.1847185798686155, -346.7906720702263215 ) ) ;
#11559 = CARTESIAN_POINT ( 'NONE',  ( -2.319525372208536496, -285.5628516571409818, -202.0363260972031867 ) ) ;
#11560 = CARTESIAN_POINT ( 'NONE',  ( 23.40701951457631935, -294.7307829323729038, -228.0591670476086108 ) ) ;
#11561 = CARTESIAN_POINT ( 'NONE',  ( 28.41597052308757299, -277.6586671755612770, -308.8626655423060470 ) ) ;
#11562 = CARTESIAN_POINT ( 'NONE',  ( 4.578856692953886309, -275.9199632546058183, -206.2985416266020025 ) ) ;
#11563 = CARTESIAN_POINT ( 'NONE',  ( 0.8696174200904051022, -276.3605945279220464, -332.6209571198442063 ) ) ;
#11564 = CARTESIAN_POINT ( 'NONE',  ( -74.18334530882417255, -297.5432225595473028, -335.4972953945558629 ) ) ;
#11565 = CARTESIAN_POINT ( 'NONE',  ( -24.81035568559763504, -284.2120783810746047, -196.5318811778817576 ) ) ;
#11566 = CARTESIAN_POINT ( 'NONE',  ( 32.16869925652592599, -292.7933900766773831, -237.1608193483886851 ) ) ;
#11567 = CARTESIAN_POINT ( 'NONE',  ( -8.516674468338223392, -290.2812446754635403, -340.9128753623573402 ) ) ;
#11568 = CARTESIAN_POINT ( 'NONE',  ( 26.51052486730400659, -291.9803529021078816, -234.2418894663271089 ) ) ;
#11569 = ORIENTED_EDGE ( 'NONE', *, *, #27631, .F. ) ;
#11570 = CARTESIAN_POINT ( 'NONE',  ( -90.36389935942597162, -289.8944950071613675, -215.2672263030509328 ) ) ;
#11571 = CARTESIAN_POINT ( 'NONE',  ( -1.242531588920580132, -292.2119008737589638, -206.8727260103918013 ) ) ;
#11572 = ORIENTED_EDGE ( 'NONE', *, *, #57340, .F. ) ;
#11573 = CARTESIAN_POINT ( 'NONE',  ( -98.77324533424825859, -291.0183084803539373, -316.2920635262997280 ) ) ;
#11574 = CARTESIAN_POINT ( 'NONE',  ( -109.0632492248754914, -278.7036895740114346, -284.1423713981456558 ) ) ;
#11575 = CARTESIAN_POINT ( 'NONE',  ( -112.2954467929809255, -295.6770092014780289, -254.0693990215986844 ) ) ;
#11576 = CARTESIAN_POINT ( 'NONE',  ( -49.33702200896129852, -286.5546397482127077, -194.3507213057398815 ) ) ;
#11577 = EDGE_CURVE ( 'NONE', #40890, #70302, #44390, .T. ) ;
#11578 = CARTESIAN_POINT ( 'NONE',  ( 38.26861755794667630, -287.7046555250698248, -255.9103688320375909 ) ) ;
#11579 = CARTESIAN_POINT ( 'NONE',  ( -101.0118354170628834, -285.3757170552138973, -234.5055412121603240 ) ) ;
#11580 = CARTESIAN_POINT ( 'NONE',  ( -64.04501568489942542, -182.5871740903956209, -362.3045948285029567 ) ) ;
#11581 = CARTESIAN_POINT ( 'NONE',  ( -113.0704522964411183, -269.5540774813418921, -295.9878753163457077 ) ) ;
#11582 = CARTESIAN_POINT ( 'NONE',  ( 195.7885930606527438, 282.2018346885278106, -110.2488485752002418 ) ) ;
#11583 = CIRCLE ( 'NONE', #55461, 0.5000000000000004441 ) ;
#11584 = CARTESIAN_POINT ( 'NONE',  ( 32.24862845876810979, -275.0482150385315663, -292.9396009730232890 ) ) ;
#11585 = CARTESIAN_POINT ( 'NONE',  ( 7.759790988737595541, -275.3402858988699791, -328.2192316810764510 ) ) ;
#11586 = CARTESIAN_POINT ( 'NONE',  ( -75.74374658687683848, -297.0619129554684150, -203.6305705875854528 ) ) ;
#11587 = CARTESIAN_POINT ( 'NONE',  ( 203.7386562182570060, 292.1033822784109475, -53.99999999998943423 ) ) ;
#11588 = CARTESIAN_POINT ( 'NONE',  ( 37.46674707484939404, -274.0344211875304268, -254.2680747095361653 ) ) ;
#11589 = CARTESIAN_POINT ( 'NONE',  ( 97.19193867083082239, -301.6141606055674060, -196.0827732276452480 ) ) ;
#11590 = CARTESIAN_POINT ( 'NONE',  ( -33.36172283956069862, -299.0420852247531798, -193.5957918784854712 ) ) ;
#11591 = CARTESIAN_POINT ( 'NONE',  ( -13.26168312770531088, -289.2230987187677442, -339.3403990955671361 ) ) ;
#11592 = CARTESIAN_POINT ( 'NONE',  ( -64.20014745993481142, -296.1966677711534999, -342.3526635091344019 ) ) ;
#11593 = CARTESIAN_POINT ( 'NONE',  ( -46.12907256121117427, -298.4358671745771971, -193.9261195272139844 ) ) ;
#11594 = CARTESIAN_POINT ( 'NONE',  ( -5.539589312092116025, -294.7884655921533863, -336.0835717210860025 ) ) ;
#11595 = ORIENTED_EDGE ( 'NONE', *, *, #61799, .F. ) ;
#11596 = CARTESIAN_POINT ( 'NONE',  ( 34.35566330565874438, -277.1644542615528053, -246.3467742006522769 ) ) ;
#11597 = ADVANCED_FACE ( 'NONE', ( #34821 ), #92559, .F. ) ;
#11598 = EDGE_CURVE ( 'NONE', #2535, #307, #76171, .T. ) ;
#11599 = ORIENTED_EDGE ( 'NONE', *, *, #15267, .F. ) ;
#11600 = CARTESIAN_POINT ( 'NONE',  ( -59.27859297360825508, -279.2832248190913447, -196.6162901275342278 ) ) ;
#11601 = UNCERTAINTY_MEASURE_WITH_UNIT (LENGTH_MEASURE( 1.000000000000000082E-05 ), #72501, 'distance_accuracy_value', 'NONE');
#11602 = CARTESIAN_POINT ( 'NONE',  ( -51.31407577090775618, -278.1764662041657630, -342.2511810393753535 ) ) ;
#11603 = CARTESIAN_POINT ( 'NONE',  ( -3.160588105494891664, -278.3671081626870887, -338.2403641731778521 ) ) ;
#11604 = CARTESIAN_POINT ( 'NONE',  ( -102.2031762563668309, -276.0604935216273361, -308.8222777740136280 ) ) ;
#11605 = CARTESIAN_POINT ( 'NONE',  ( -96.33476895739782719, -273.6485508082550382, -227.1747776428907173 ) ) ;
#11606 = CARTESIAN_POINT ( 'NONE',  ( -44.60935979190379896, -296.5332539400791347, -197.0808543419433647 ) ) ;
#11607 = CARTESIAN_POINT ( 'NONE',  ( 153.4245301327638344, 19.61868323046913432, -10.85241966621300591 ) ) ;
#11608 = CARTESIAN_POINT ( 'NONE',  ( -106.2635040667686610, -278.3969885493340826, -294.5723588836564772 ) ) ;
#11609 = CARTESIAN_POINT ( 'NONE',  ( -12.40042463954857332, -287.4193648854037519, -342.7438763495526928 ) ) ;
#11610 = CARTESIAN_POINT ( 'NONE',  ( -36.97575334906754563, -276.0569231635925576, -195.3492938116267226 ) ) ;
#11611 = DIRECTION ( 'NONE',  ( 0.8348322475753292560, 0.5505044217881672752, -0.000000000000000000 ) ) ;
#11612 = CARTESIAN_POINT ( 'NONE',  ( -75.96263931986773343, -288.7796748299530236, -332.4982629346425824 ) ) ;
#11613 = CARTESIAN_POINT ( 'NONE',  ( -94.32919781409560755, -283.1982718715816532, -322.0114345590041580 ) ) ;
#11614 = CARTESIAN_POINT ( 'NONE',  ( 6.169978848331856724, -280.6922266477875496, -330.2335473955945417 ) ) ;
#11616 = CARTESIAN_POINT ( 'NONE',  ( -109.4169125134991134, -282.8729681504414657, -251.7471995278742156 ) ) ;
#11615 = CARTESIAN_POINT ( 'NONE',  ( 35.15064247038245071, -279.9612275208723418, -257.7027143469986754 ) ) ;
#11617 = CARTESIAN_POINT ( 'NONE',  ( -25.03178290578624399, -288.2091696749959624, -196.3264024738879243 ) ) ;
#11618 = CARTESIAN_POINT ( 'NONE',  ( -102.2006786956894757, -279.2917446365155456, -304.7186994294927445 ) ) ;
#11619 = DIRECTION ( 'NONE',  ( 0.000000000000000000, 0.000000000000000000, 1.000000000000000000 ) ) ;
#11620 = CARTESIAN_POINT ( 'NONE',  ( -80.79295932109633327, -293.4626542217836800, -209.2302033757691788 ) ) ;
#11621 = CARTESIAN_POINT ( 'NONE',  ( -96.28278228896346036, -276.1397277320244825, -318.3390113488942461 ) ) ;
#11622 = CARTESIAN_POINT ( 'NONE',  ( 25.46738383376368020, -276.7170583646852151, -307.7631451985898821 ) ) ;
#11623 = CARTESIAN_POINT ( 'NONE',  ( -108.9314939596393543, -286.2567375103013774, -293.3148658332976311 ) ) ;
#11624 = CARTESIAN_POINT ( 'NONE',  ( 196.0143093133015384, 73.40565171261611965, 12.00000000000000711 ) ) ;
#11625 = CARTESIAN_POINT ( 'NONE',  ( -106.4050623250753915, -292.0721932180657632, -301.1420541801509216 ) ) ;
#11626 = CARTESIAN_POINT ( 'NONE',  ( -111.4131706052021826, -294.3998911031088710, -282.2070421955319830 ) ) ;
#11627 = CARTESIAN_POINT ( 'NONE',  ( -12.74570201443743223, -285.5611213048340460, -197.5655432750447744 ) ) ;
#11628 = CARTESIAN_POINT ( 'NONE',  ( -110.0615381874820429, -289.1199781494431704, -257.4894350983458366 ) ) ;
#11629 = CARTESIAN_POINT ( 'NONE',  ( 82.64890176555634582, -299.5541904835127980, -202.0153591320744226 ) ) ;
#11630 = CARTESIAN_POINT ( 'NONE',  ( 29.59658498552832029, -274.6431605175964705, -300.7010168396257086 ) ) ;
#11631 = CARTESIAN_POINT ( 'NONE',  ( 17.04827757031210211, -292.4058820509746397, -320.8843384530421758 ) ) ;
#11632 = CARTESIAN_POINT ( 'NONE',  ( 113.5000000000000568, -192.7866584945343504, -490.8867980474134356 ) ) ;
#11633 = CARTESIAN_POINT ( 'NONE',  ( 144.2857639756989272, -299.5541904835127980, -195.3611179825600175 ) ) ;
#11634 = CARTESIAN_POINT ( 'NONE',  ( -64.12712969097799487, -290.1889964378135573, -198.8544353375396838 ) ) ;
#11635 = CARTESIAN_POINT ( 'NONE',  ( -98.78428046866444845, -286.7136077545509352, -229.4801965607597367 ) ) ;
#11636 = CARTESIAN_POINT ( 'NONE',  ( 29.46100516558870908, -286.2679947538612737, -306.6839816260460339 ) ) ;
#11637 = CARTESIAN_POINT ( 'NONE',  ( -105.1474911294664878, -286.3597133522752074, -241.6337416539681726 ) ) ;
#11638 = DIRECTION ( 'NONE',  ( 1.000000000000000000, -0.000000000000000000, 0.000000000000000000 ) ) ;
#11639 = CARTESIAN_POINT ( 'NONE',  ( -60.03840806735935587, -286.5531606275172862, -200.8092583711334100 ) ) ;
#11640 = CARTESIAN_POINT ( 'NONE',  ( 32.91987177790567642, -295.1778266320673083, -242.9825372491910969 ) ) ;
#11641 = CARTESIAN_POINT ( 'NONE',  ( -88.26010818284377990, -275.8386055020574759, -326.1879029240238310 ) ) ;
#11642 = CARTESIAN_POINT ( 'NONE',  ( -5.289708302656784156, -276.9750615321442524, -340.3497892919464221 ) ) ;
#11643 = CARTESIAN_POINT ( 'NONE',  ( 16.48136691980723256, -290.8891718643524200, -217.2554290598356488 ) ) ;
#11644 = CARTESIAN_POINT ( 'NONE',  ( -111.3372469311076856, -278.8191976690511638, -249.0618444428088765 ) ) ;
#11645 = CARTESIAN_POINT ( 'NONE',  ( -74.09069615543015175, -297.5229575377426841, -335.3330972860230759 ) ) ;
#11646 = FACE_BOUND ( 'NONE', #799, .T. ) ;
#11647 = DIRECTION ( 'NONE',  ( -0.000000000000000000, -1.000000000000000000, -0.000000000000000000 ) ) ;
#11648 = CARTESIAN_POINT ( 'NONE',  ( 32.31329700962663054, -285.9276872772892375, -246.9213045967846654 ) ) ;
#11649 = CARTESIAN_POINT ( 'NONE',  ( -108.3042741779299689, -276.4057819892398129, -292.3320249914052056 ) ) ;
#11650 = CARTESIAN_POINT ( 'NONE',  ( 25.04376588432860018, -280.1146008827191167, -311.9910865051884912 ) ) ;
#11651 = DIRECTION ( 'NONE',  ( 0.000000000000000000, 0.000000000000000000, 1.000000000000000000 ) ) ;
#11652 = CARTESIAN_POINT ( 'NONE',  ( -29.88718316410720632, -272.6247755084341406, -194.4194434616762237 ) ) ;
#11653 = CARTESIAN_POINT ( 'NONE',  ( 36.33594807749791755, -295.1132910682781585, -273.4993714367753910 ) ) ;
#11654 = CARTESIAN_POINT ( 'NONE',  ( 23.51046387246500302, -279.8471644805388223, -223.6651848667837044 ) ) ;
#11655 = CARTESIAN_POINT ( 'NONE',  ( -3.022918825840486434, -295.5281451286790002, -335.0575606866904650 ) ) ;
#11656 = CARTESIAN_POINT ( 'NONE',  ( -111.4865478233219278, -297.6291528604314749, -289.2776772275749977 ) ) ;
#11657 = CARTESIAN_POINT ( 'NONE',  ( -41.86622181449494207, -297.8268698960334859, -197.5014672283679715 ) ) ;
#11658 = CARTESIAN_POINT ( 'NONE',  ( -94.99312199470141138, -293.2149144762724973, -222.3690452327836056 ) ) ;
#11659 = CARTESIAN_POINT ( 'NONE',  ( -73.61489112234414733, -285.7513802489950763, -202.3811118123230699 ) ) ;
#11660 = CARTESIAN_POINT ( 'NONE',  ( 36.03645121284596087, -273.9317012814196346, -289.2278185178793706 ) ) ;
#11661 = CARTESIAN_POINT ( 'NONE',  ( 18.64335908102332695, -288.1074178690261078, -323.2257862389564025 ) ) ;
#11662 = EDGE_CURVE ( 'NONE', #4210, #49577, #1017, .T. ) ;
#11663 = CARTESIAN_POINT ( 'NONE',  ( 34.22849508360164350, -286.4067173510317730, -254.8332203058909045 ) ) ;
#11664 = CARTESIAN_POINT ( 'NONE',  ( -66.22116472758847294, -289.6739569152180707, -201.1442329411145238 ) ) ;
#11665 = ORIENTED_EDGE ( 'NONE', *, *, #83215, .T. ) ;
#11666 = CARTESIAN_POINT ( 'NONE',  ( -75.10193482699480683, -210.9688814900462432, -359.8487438039043127 ) ) ;
#11667 = CARTESIAN_POINT ( 'NONE',  ( -70.00559712005777158, -289.0021050615021068, -335.7283235549663232 ) ) ;
#11668 = DIRECTION ( 'NONE',  ( -1.000000000000000000, 0.000000000000000000, 0.000000000000000000 ) ) ;
#11669 = CARTESIAN_POINT ( 'NONE',  ( -102.7114169038248264, -284.9657750020126059, -310.6056249522939083 ) ) ;
#11670 = CARTESIAN_POINT ( 'NONE',  ( 37.55171220868359683, -292.8229808298123658, -287.2666842175201509 ) ) ;
#11671 = CARTESIAN_POINT ( 'NONE',  ( 37.88141747907987167, -283.3070123656646047, -282.6051177324919195 ) ) ;
#11672 = CARTESIAN_POINT ( 'NONE',  ( 24.18511593081843358, -282.2590850588985631, -224.8886078306695708 ) ) ;
#11673 = CARTESIAN_POINT ( 'NONE',  ( -10.97775055176488834, -282.5321013339286651, -338.4877626633717682 ) ) ;
#11674 = CARTESIAN_POINT ( 'NONE',  ( -24.27228820052091507, -276.2190463883545704, -196.4556234875636278 ) ) ;
#11675 = CARTESIAN_POINT ( 'NONE',  ( -100.0085033970901378, -295.9584688961542156, -315.1932064507313953 ) ) ;
#11676 = CARTESIAN_POINT ( 'NONE',  ( -111.9515173681788838, -288.5257767519766503, -273.9637530710510873 ) ) ;
#11677 = CARTESIAN_POINT ( 'NONE',  ( -72.98519972288366375, -296.4882235488046263, -206.3004669503997945 ) ) ;
#11678 = ORIENTED_EDGE ( 'NONE', *, *, #14901, .F. ) ;
#11679 = ORIENTED_EDGE ( 'NONE', *, *, #33815, .F. ) ;
#11680 = CARTESIAN_POINT ( 'NONE',  ( 222.4306832106270804, -135.2391364535880882, 22.50000000000000000 ) ) ;
#11681 = CARTESIAN_POINT ( 'NONE',  ( -107.5233276065386150, -286.1466326648921950, -295.3308615078214530 ) ) ;
#11682 = CARTESIAN_POINT ( 'NONE',  ( -33.43677011586752457, -296.0837740014431461, -346.9655942397035915 ) ) ;
#11683 = CARTESIAN_POINT ( 'NONE',  ( -42.93244548060171439, -283.7758508834265285, -343.2991078337446424 ) ) ;
#11684 = CARTESIAN_POINT ( 'NONE',  ( -34.31241549124833767, -276.0736885875668349, -347.0660307852529058 ) ) ;
#11685 = CARTESIAN_POINT ( 'NONE',  ( -69.58799349518503163, -292.2901725061936418, -200.5364135441451481 ) ) ;
#11686 = CARTESIAN_POINT ( 'NONE',  ( -57.40565113898599492, -283.9356145187182392, -197.2467975960159094 ) ) ;
#11687 = CARTESIAN_POINT ( 'NONE',  ( -86.50279144521452679, -291.7243194107862791, -211.0556685650587383 ) ) ;
#11688 = CARTESIAN_POINT ( 'NONE',  ( -109.7216608513759581, -291.0177183754245220, -260.3304151526854753 ) ) ;
#11689 = FACE_OUTER_BOUND ( 'NONE', #19985, .T. ) ;
#11690 = LINE ( 'NONE', #31611, #47780 ) ;
#11691 = CARTESIAN_POINT ( 'NONE',  ( 26.11126514475094140, -24.39807644324349667, -341.5406973817991343 ) ) ;
#11692 = CARTESIAN_POINT ( 'NONE',  ( -34.48536626912725467, -284.5369755402188048, -346.6143088077583343 ) ) ;
#11693 = CARTESIAN_POINT ( 'NONE',  ( -95.99890600148557951, -287.4094976428776249, -317.0979686699210447 ) ) ;
#11694 = ORIENTED_EDGE ( 'NONE', *, *, #80334, .F. ) ;
#11695 = CARTESIAN_POINT ( 'NONE',  ( -1.111146971636954639, -281.4794899202430543, -334.0915902221684632 ) ) ;
#11696 = CARTESIAN_POINT ( 'NONE',  ( 37.57030876805323771, -275.4411775086145440, -288.1360987535976506 ) ) ;
#11697 = CARTESIAN_POINT ( 'NONE',  ( -90.80066947534646715, -281.2923472873845867, -217.9219484851064976 ) ) ;
#11698 = CARTESIAN_POINT ( 'NONE',  ( -68.68430080596803577, -197.1092947213748801, -358.3343516210577491 ) ) ;
#11699 = CARTESIAN_POINT ( 'NONE',  ( 31.85105581707266253, -280.5466157161601473, -302.9043616880563263 ) ) ;
#11700 = CARTESIAN_POINT ( 'NONE',  ( -77.92258379212319142, -283.5245112615154994, -207.6496734141182117 ) ) ;
#11701 = CARTESIAN_POINT ( 'NONE',  ( -34.12330758321979118, -299.8520531893593102, -194.3734957074033787 ) ) ;
#11702 = CARTESIAN_POINT ( 'NONE',  ( -10.46153253366171754, -295.1840593404305082, -338.2981846826284027 ) ) ;
#11703 = ORIENTED_EDGE ( 'NONE', *, *, #42165, .F. ) ;
#11704 = CARTESIAN_POINT ( 'NONE',  ( -109.9086964929104084, -289.0835355329542153, -282.0711414671125112 ) ) ;
#11705 = CARTESIAN_POINT ( 'NONE',  ( 8.187397591614196557, -277.0993197920200259, -332.3981239670805508 ) ) ;
#11706 = CARTESIAN_POINT ( 'NONE',  ( -19.27162332516118681, -274.2910648713669275, -199.5805329121355953 ) ) ;
#11707 = CARTESIAN_POINT ( 'NONE',  ( 36.19314342898342574, -274.7472866812546499, -292.1817026711595418 ) ) ;
#11708 = CARTESIAN_POINT ( 'NONE',  ( 133.0380396672494783, -299.5541904835127980, -195.3611179825600175 ) ) ;
#11709 = CARTESIAN_POINT ( 'NONE',  ( -106.3021228730598295, -270.9389989292703831, -240.7440863109640077 ) ) ;
#11710 = DIRECTION ( 'NONE',  ( 0.000000000000000000, 0.000000000000000000, 1.000000000000000000 ) ) ;
#11711 = CARTESIAN_POINT ( 'NONE',  ( 199.2296996224750103, 68.12454877784578855, 2.107038703926640721 ) ) ;
#11712 = CARTESIAN_POINT ( 'NONE',  ( -16.02956128768343547, -283.8496364557395282, -340.5039637401467871 ) ) ;
#11713 = CARTESIAN_POINT ( 'NONE',  ( -0.8422296462996153865, -284.3345153356459605, -337.0224127571835311 ) ) ;
#11714 = CARTESIAN_POINT ( 'NONE',  ( -99.12161761480486177, -283.3603405406467459, -309.5344671044090887 ) ) ;
#11715 = CARTESIAN_POINT ( 'NONE',  ( -56.83084584935117789, -275.7074002510711921, -341.5943448547106982 ) ) ;
#11716 = CARTESIAN_POINT ( 'NONE',  ( -7.984325615633683704, -284.5238214239820991, -338.5447673707404874 ) ) ;
#11717 = CARTESIAN_POINT ( 'NONE',  ( -37.83363503378704706, -275.5382638401135296, -344.0653827548361505 ) ) ;
#11718 = CARTESIAN_POINT ( 'NONE',  ( 195.7510731661265595, -141.7221692137691775, -22.50000000000000000 ) ) ;
#11719 = CARTESIAN_POINT ( 'NONE',  ( 195.9136854370872811, 42.35701288050587721, 12.17428566605772922 ) ) ;
#11720 = CARTESIAN_POINT ( 'NONE',  ( -69.90327055032263104, -280.4370216824067370, -200.7486047600565087 ) ) ;
#11721 = ADVANCED_FACE ( 'NONE', ( #12583, #14467 ), #20624, .T. ) ;
#11722 = VERTEX_POINT ( 'NONE', #77439 ) ;
#11723 = EDGE_LOOP ( 'NONE', ( #3891, #57612, #83619, #43939 ) ) ;
#11724 = DIRECTION ( 'NONE',  ( -0.000000000000000000, -1.000000000000000000, -0.000000000000000000 ) ) ;
#11725 = CARTESIAN_POINT ( 'NONE',  ( -91.04444654790594882, -287.1595835766373170, -216.9165625403198021 ) ) ;
#11726 = CARTESIAN_POINT ( 'NONE',  ( -47.82626200431142394, -294.3859196442186317, -342.8188357746217889 ) ) ;
#11727 = EDGE_CURVE ( 'NONE', #49577, #610, #40228, .T. ) ;
#11728 = CARTESIAN_POINT ( 'NONE',  ( -98.95245104799202807, -289.2875037354023675, -316.3984167867946553 ) ) ;
#11729 = CARTESIAN_POINT ( 'NONE',  ( 16.72988289493238057, -285.0747629120200486, -219.8029399253381371 ) ) ;
#11731 = CARTESIAN_POINT ( 'NONE',  ( -109.3413263621045672, -288.5688874194672167, -287.5083579527609459 ) ) ;
#11730 = CARTESIAN_POINT ( 'NONE',  ( -5.527607383993497159, -285.0537078233779766, -203.9903196028090804 ) ) ;
#11732 = CARTESIAN_POINT ( 'NONE',  ( -107.3600760673499366, -285.4670424617925164, -292.3737856042744170 ) ) ;
#11733 = CARTESIAN_POINT ( 'NONE',  ( 9.262817734426024074, -274.4122399569943695, -329.1898158302455499 ) ) ;
#11734 = CARTESIAN_POINT ( 'NONE',  ( -23.90671828721737668, -284.6207606491204842, -195.3011844166014725 ) ) ;
#11735 = CARTESIAN_POINT ( 'NONE',  ( -48.69310354446782441, -299.9079007241820705, -196.1728451924504952 ) ) ;
#11736 = CARTESIAN_POINT ( 'NONE',  ( 17.29431629925166547, -286.2742332370357303, -321.9841180463167234 ) ) ;
#11737 = CARTESIAN_POINT ( 'NONE',  ( -9.167869994485087659, -281.3710761509059353, -202.7619778689879979 ) ) ;
#11738 = CARTESIAN_POINT ( 'NONE',  ( -56.79135804319869152, -291.3023910024834322, -343.0216492172917242 ) ) ;
#11739 = CARTESIAN_POINT ( 'NONE',  ( 209.2599468862078140, 293.9636489450776367, 3.999999999999991562 ) ) ;
#11740 = DIRECTION ( 'NONE',  ( 0.000000000000000000, 1.000000000000000000, 0.000000000000000000 ) ) ;
#11741 = CARTESIAN_POINT ( 'NONE',  ( -27.90300671838431157, -296.8534991211220699, -345.3815764387252898 ) ) ;
#11742 = CARTESIAN_POINT ( 'NONE',  ( -80.17683077337308362, -277.4719795954232495, -208.7969057410843163 ) ) ;
#11743 = CARTESIAN_POINT ( 'NONE',  ( -72.09007957810054279, -290.8016131279472916, -201.8140108161004207 ) ) ;
#11744 = CARTESIAN_POINT ( 'NONE',  ( -96.73212947363174408, -295.5596340879585568, -226.5309178835082378 ) ) ;
#11745 = CARTESIAN_POINT ( 'NONE',  ( 16.17354225024463688, -280.9580061116063234, -320.8067575354481846 ) ) ;
#11746 = CARTESIAN_POINT ( 'NONE',  ( -21.60625329655805871, -272.3352913046833805, -197.6032324449385271 ) ) ;
#11747 = CARTESIAN_POINT ( 'NONE',  ( 17.45939652356535987, -295.5632921491301204, -319.3503253922410181 ) ) ;
#11748 = CARTESIAN_POINT ( 'NONE',  ( 31.98288692825981272, -290.4805209788416391, -303.7098442033570223 ) ) ;
#11749 = CARTESIAN_POINT ( 'NONE',  ( -62.59715637206504368, -296.2092224565062679, -198.3550787787695526 ) ) ;
#11750 = CARTESIAN_POINT ( 'NONE',  ( 37.85251465581007579, -291.6488165154114540, -259.0618612532959446 ) ) ;
#11751 = CARTESIAN_POINT ( 'NONE',  ( -102.1535652485686256, -291.5046454847147857, -305.3230467993019488 ) ) ;
#11752 = CARTESIAN_POINT ( 'NONE',  ( -22.78264641048746597, -118.9815703160634541, -22.50000000000000000 ) ) ;
#11753 = CARTESIAN_POINT ( 'NONE',  ( -65.39831883214733921, -292.4786069832919679, -202.7796229373281562 ) ) ;
#11754 = DIRECTION ( 'NONE',  ( 0.000000000000000000, 0.000000000000000000, 1.000000000000000000 ) ) ;
#11756 = CARTESIAN_POINT ( 'NONE',  ( -34.85728298530064251, -292.0842281890849677, -197.4034064541639566 ) ) ;
#11755 = CARTESIAN_POINT ( 'NONE',  ( -30.39222680375099372, -280.9847636096063184, -345.3951877304016875 ) ) ;
#11757 = CARTESIAN_POINT ( 'NONE',  ( 39.27810925450119584, -281.6541718384929140, -278.5185280903869511 ) ) ;
#11758 = CARTESIAN_POINT ( 'NONE',  ( -65.24848116184352875, -283.0737654950311253, -342.1176060608789271 ) ) ;
#11759 = CARTESIAN_POINT ( 'NONE',  ( -26.22713541370747592, -286.9103189059982810, -344.4167914571044662 ) ) ;
#11760 = CARTESIAN_POINT ( 'NONE',  ( -48.53796866150762668, -281.3357794512028249, -343.7471455981579425 ) ) ;
#11761 = CARTESIAN_POINT ( 'NONE',  ( -48.00259242569042328, -278.3989126251840958, -194.7494835698466602 ) ) ;
#11762 = CARTESIAN_POINT ( 'NONE',  ( 30.08434164730011062, -286.9483550530452476, -307.0128268430932508 ) ) ;
#11763 = CARTESIAN_POINT ( 'NONE',  ( 195.4093337208560399, 40.63452519861395729, 14.75905111207264220 ) ) ;
#11764 = CARTESIAN_POINT ( 'NONE',  ( 23.23304758720301422, -294.5707959261951601, -228.1827175810766732 ) ) ;
#11765 = CARTESIAN_POINT ( 'NONE',  ( -31.47723787421008979, -278.4048796134323993, -346.5987331437362968 ) ) ;
#11766 = CARTESIAN_POINT ( 'NONE',  ( -71.66787631362498701, -277.1855977076144200, -334.8252113265434105 ) ) ;
#11767 = CARTESIAN_POINT ( 'NONE',  ( -27.85119685655844535, -292.3360322400757809, -193.8945498252629420 ) ) ;
#11768 = CARTESIAN_POINT ( 'NONE',  ( -80.75458304236330775, -281.7155013947428870, -332.2684242999184221 ) ) ;
#11769 = CARTESIAN_POINT ( 'NONE',  ( 33.53894712342368223, -292.3684801669259059, -251.9398722610837069 ) ) ;
#11770 = CARTESIAN_POINT ( 'NONE',  ( -100.6150815138749977, -295.0938930828261277, -230.0935149264976758 ) ) ;
#11771 = ORIENTED_EDGE ( 'NONE', *, *, #49238, .T. ) ;
#11772 = CARTESIAN_POINT ( 'NONE',  ( 184.7149167944524493, 8.542400036368780647, -9.000000000000001776 ) ) ;
#11773 = CARTESIAN_POINT ( 'NONE',  ( 10.32693495289770702, -293.8807372098407313, -325.7297884649692605 ) ) ;
#11774 = FACE_BOUND ( 'NONE', #56566, .T. ) ;
#11775 = CARTESIAN_POINT ( 'NONE',  ( -92.05005921254146983, -288.6952119285918457, -226.6919474004047572 ) ) ;
#11776 = CARTESIAN_POINT ( 'NONE',  ( -36.88651872117245034, -297.1164735630179621, -193.5964809375084030 ) ) ;
#11777 = CARTESIAN_POINT ( 'NONE',  ( 35.99021109349600067, -279.9340052404979247, -289.4067547463413916 ) ) ;
#11778 = EDGE_CURVE ( 'NONE', #1585, #19733, #52981, .T. ) ;
#11779 = EDGE_CURVE ( 'NONE', #24854, #25416, #65594, .T. ) ;
#11780 = CARTESIAN_POINT ( 'NONE',  ( 15.94364210691151484, -288.1037122962427475, -215.4614770469405300 ) ) ;
#11781 = CARTESIAN_POINT ( 'NONE',  ( -84.68664261970612017, -289.5590650814730793, -325.9927252284525139 ) ) ;
#11782 = CARTESIAN_POINT ( 'NONE',  ( -108.8400967152963403, -279.8382973938271334, -288.2648901868055873 ) ) ;
#11783 = CARTESIAN_POINT ( 'NONE',  ( -78.88563823001278763, -293.6348069637433014, -332.4392710130770752 ) ) ;
#11784 = CARTESIAN_POINT ( 'NONE',  ( -41.95356932101942959, -299.7533800294712591, -196.4916068367509183 ) ) ;
#11785 = CARTESIAN_POINT ( 'NONE',  ( -110.7893362632360805, -277.3436170816679578, -270.6242444570373209 ) ) ;
#11786 = ORIENTED_EDGE ( 'NONE', *, *, #16494, .F. ) ;
#11787 = CARTESIAN_POINT ( 'NONE',  ( -113.8624312931764138, -272.4927491730388738, -261.7833731474086676 ) ) ;
#11788 = CARTESIAN_POINT ( 'NONE',  ( -48.24827296263730148, -291.1120298774809498, -344.0498264543599021 ) ) ;
#11789 = CARTESIAN_POINT ( 'NONE',  ( 38.05723960318069743, -295.0085439118863064, -258.9877242958766033 ) ) ;
#11790 = CARTESIAN_POINT ( 'NONE',  ( 201.6516428717762608, 292.4574023500951512, -53.99999999997706368 ) ) ;
#11791 = CARTESIAN_POINT ( 'NONE',  ( -108.7605268715318374, -290.9974035083213835, -286.0155553866644027 ) ) ;
#11792 = CARTESIAN_POINT ( 'NONE',  ( -48.18343439339133027, -248.3668650810685676, -465.6442049081568371 ) ) ;
#11793 = VERTEX_POINT ( 'NONE', #9174 ) ;
#11794 = CARTESIAN_POINT ( 'NONE',  ( -91.56952993098747129, -297.9554750583028522, -215.8390558306278706 ) ) ;
#11795 = CARTESIAN_POINT ( 'NONE',  ( -110.4347962095075104, -288.9461554691451397, -250.3694094784423214 ) ) ;
#11796 = CARTESIAN_POINT ( 'NONE',  ( -89.59706575995504352, -297.6729351026829704, -213.7635042708118931 ) ) ;
#11797 = DIRECTION ( 'NONE',  ( -0.8457827187922973833, -0.5335274993777826547, -0.000000000000000000 ) ) ;
#11798 = FACE_OUTER_BOUND ( 'NONE', #16591, .T. ) ;
#11799 = CARTESIAN_POINT ( 'NONE',  ( 5.187096875363059745, -290.0083104836809866, -333.7173266510132521 ) ) ;
#11800 = CARTESIAN_POINT ( 'NONE',  ( -2.659677404128715672, -282.9805209788415823, -198.2697987213421698 ) ) ;
#11801 = CARTESIAN_POINT ( 'NONE',  ( -111.4308302195787661, -286.6877879847500026, -259.8335717846267130 ) ) ;
#11802 = CARTESIAN_POINT ( 'NONE',  ( 33.32150121606481008, -285.7530049581886260, -241.1484515462541367 ) ) ;
#11803 = CARTESIAN_POINT ( 'NONE',  ( -18.79317459280651548, -272.2912262461288719, -197.8092274115205953 ) ) ;
#11804 = CARTESIAN_POINT ( 'NONE',  ( -93.11293265455064727, -275.1630468386803159, -221.0571240069463101 ) ) ;
#11805 = CARTESIAN_POINT ( 'NONE',  ( -110.6003346563089877, -288.4611142822752186, -283.5704581172514054 ) ) ;
#11806 = CARTESIAN_POINT ( 'NONE',  ( -34.31631551368566591, -278.8749037063864762, -346.0654938829343905 ) ) ;
#11807 = ORIENTED_EDGE ( 'NONE', *, *, #80555, .F. ) ;
#11809 = CARTESIAN_POINT ( 'NONE',  ( 33.55647239966744166, -280.6653617867252137, -252.4961469644773047 ) ) ;
#11808 = CARTESIAN_POINT ( 'NONE',  ( -41.05118505629953773, -280.0041679465415996, -197.4554273845873524 ) ) ;
#11810 = CARTESIAN_POINT ( 'NONE',  ( 25.82015139036784745, -277.2094185429656363, -313.9510211707606118 ) ) ;
#11811 = CARTESIAN_POINT ( 'NONE',  ( 22.57439089600631021, -279.7045637080174174, -222.6111188941444539 ) ) ;
#11812 = CARTESIAN_POINT ( 'NONE',  ( -107.3525364133518849, -259.7561089835505186, -315.8720887335824727 ) ) ;
#11813 = CARTESIAN_POINT ( 'NONE',  ( -5.223660991503157547, -275.4058667572645049, -200.6384403523648530 ) ) ;
#11814 = PRODUCT_CONTEXT ( 'NONE', #58995, 'mechanical' ) ;
#11815 = CARTESIAN_POINT ( 'NONE',  ( -100.6443058047159553, -274.6397606081572462, -227.6584728236507829 ) ) ;
#11816 = CARTESIAN_POINT ( 'NONE',  ( -37.37352853689063892, -294.5519495502701943, -195.3611179825600175 ) ) ;
#11817 = VERTEX_POINT ( 'NONE', #87782 ) ;
#11818 = VECTOR ( 'NONE', #27744, 999.9999999999998863 ) ;
#11819 = CARTESIAN_POINT ( 'NONE',  ( 165.2688068684385883, 275.0000000000000568, 21.83530662808711398 ) ) ;
#11820 = CARTESIAN_POINT ( 'NONE',  ( 25.96991669313003825, -289.1381429757798855, -307.4191197812877476 ) ) ;
#11821 = CARTESIAN_POINT ( 'NONE',  ( 31.95012996263987759, -289.7159460382678731, -301.5479147726393307 ) ) ;
#11822 = CARTESIAN_POINT ( 'NONE',  ( -95.85489269177629978, -289.2862853594372723, -314.2009448446495981 ) ) ;
#11823 = CARTESIAN_POINT ( 'NONE',  ( -65.84872774809066698, -285.1967355518366389, -198.8845636537164410 ) ) ;
#11824 = CARTESIAN_POINT ( 'NONE',  ( 197.4878715644970555, 25.93102243561467546, 11.99999999999999112 ) ) ;
#11825 = CARTESIAN_POINT ( 'NONE',  ( 32.98754730838870586, -280.2473129105107432, -292.8933919597594695 ) ) ;
#11826 = CARTESIAN_POINT ( 'NONE',  ( -31.75514733084627039, -290.8414603354181054, -344.4372960680524329 ) ) ;
#11827 = CARTESIAN_POINT ( 'NONE',  ( -33.47906054805210374, -281.4825587910334548, -343.9658460776556126 ) ) ;
#11828 = CARTESIAN_POINT ( 'NONE',  ( -108.2920067222448921, -279.6158749119506410, -289.5261244584051497 ) ) ;
#11829 = CARTESIAN_POINT ( 'NONE',  ( -80.85100677912684830, -278.1533820175014853, -329.0546327539217373 ) ) ;
#11830 = CARTESIAN_POINT ( 'NONE',  ( -112.7783104193172363, -289.5144841047574005, -257.0447165564938246 ) ) ;
#11831 = CARTESIAN_POINT ( 'NONE',  ( -112.9761822890654912, -285.1815137696266902, -284.2023576766145538 ) ) ;
#11832 = CARTESIAN_POINT ( 'NONE',  ( 27.08280086380950991, -287.4914927807429876, -228.3015105766904469 ) ) ;
#11833 = CARTESIAN_POINT ( 'NONE',  ( 20.18228246193993414, -282.3523327063134616, -315.3054327678537447 ) ) ;
#11834 = ORIENTED_EDGE ( 'NONE', *, *, #67723, .F. ) ;
#11835 = CARTESIAN_POINT ( 'NONE',  ( 73.43068321062709458, -134.2391364535880598, 0.000000000000000000 ) ) ;
#11836 = CARTESIAN_POINT ( 'NONE',  ( -83.53236201604286748, -293.2871538132972660, -210.2389378926997665 ) ) ;
#11837 = CARTESIAN_POINT ( 'NONE',  ( -79.30981323136398942, -290.1836321062335742, -206.3292459575291957 ) ) ;
#11838 = CARTESIAN_POINT ( 'NONE',  ( 5.323522573438709493, -273.7038557481634484, -210.7745949941079573 ) ) ;
#11839 = CARTESIAN_POINT ( 'NONE',  ( -34.86624419779202810, -294.3704082286992048, -347.2193309779238461 ) ) ;
#11840 = CARTESIAN_POINT ( 'NONE',  ( -41.61385774977839702, -290.4773847918907563, -196.7413988045967699 ) ) ;
#11841 = CARTESIAN_POINT ( 'NONE',  ( -93.87066067648564172, -294.1221814493834472, -318.1557593804848807 ) ) ;
#11842 = B_SPLINE_CURVE_WITH_KNOTS ( 'NONE', 3,
 ( #49946, #37144, #86865, #58473, #22019, #65596, #1164, #64211, #30047, #87317, #14913, #22465, #85473, #20620, #21075, #42846, #49491, #71762, #8713, #10576, #81155, #2565, #81611, #30503, #51798, #66501, #59874, #74051 ),
 .UNSPECIFIED., .F., .F.,
 ( 4, 2, 2, 2, 2, 2, 2, 2, 2, 2, 2, 2, 2, 4 ),
 ( 0.006505935382142305663, 0.006896669962658084560, 0.007287404543173863457, 0.007678139123689642354, 0.008068873704205420383, 0.008459608284721200147, 0.008850342865236978177, 0.009241077445752757941, 0.009631812026268535970, 0.01041328118730009203, 0.01119475034833164982, 0.01158548492884745734, 0.01197621950936326660, 0.01275768867039482266 ),
 .UNSPECIFIED. ) ;
#11843 = CARTESIAN_POINT ( 'NONE',  ( -63.95061020473567481, -290.6120151509840639, -338.8195136740945941 ) ) ;
#11844 = CARTESIAN_POINT ( 'NONE',  ( 219.8344101925596021, 0.000000000000000000, 9.000000000000001776 ) ) ;
#11845 = CARTESIAN_POINT ( 'NONE',  ( -111.1601629958731507, -292.3811216796044050, -283.6938090988346062 ) ) ;
#11846 = CARTESIAN_POINT ( 'NONE',  ( -1.651351009163778416, -290.5239215389173637, -204.2080575212583256 ) ) ;
#11847 = CARTESIAN_POINT ( 'NONE',  ( 34.93054123707709380, -295.8122833016357163, -290.5912999540839792 ) ) ;
#11848 = CARTESIAN_POINT ( 'NONE',  ( -17.11836718601185936, -287.2608417565090804, -199.9204242047243554 ) ) ;
#11849 = CARTESIAN_POINT ( 'NONE',  ( -9.053773662506463538, -296.6833939349633624, -340.0569250178330094 ) ) ;
#11850 = CARTESIAN_POINT ( 'NONE',  ( 37.11466220994713439, -277.6845312497366649, -282.2934803350398170 ) ) ;
#11851 = CARTESIAN_POINT ( 'NONE',  ( 21.41613360024045321, -275.0119424398041019, -319.5091158610763955 ) ) ;
#11852 = EDGE_CURVE ( 'NONE', #49537, #37280, #91679, .T. ) ;
#11853 = CARTESIAN_POINT ( 'NONE',  ( -98.95681923200736207, -296.3614924859028861, -224.4290767416403583 ) ) ;
#11854 = CARTESIAN_POINT ( 'NONE',  ( -48.78634528543979343, -275.4396036881377086, -343.5363659927569415 ) ) ;
#11855 = CARTESIAN_POINT ( 'NONE',  ( -71.58269891887039194, -277.6760637381186143, -204.2493401320581654 ) ) ;
#11856 = CARTESIAN_POINT ( 'NONE',  ( -106.6865357460839334, -274.0753466474948254, -246.3106652291610033 ) ) ;
#11857 = CARTESIAN_POINT ( 'NONE',  ( -21.45941477323787794, -272.8267042362189727, -195.6191665549959566 ) ) ;
#11858 = CARTESIAN_POINT ( 'NONE',  ( -101.9762590594997675, -297.5010479940899017, -305.5427709767504325 ) ) ;
#11859 = CARTESIAN_POINT ( 'NONE',  ( 198.5394373320682746, 68.65923120349998499, 9.381478303810135699 ) ) ;
#11860 = CARTESIAN_POINT ( 'NONE',  ( -66.89392010452345971, -298.4575382553139775, -203.4200729694276504 ) ) ;
#11861 = FACE_OUTER_BOUND ( 'NONE', #15049, .T. ) ;
#11863 = CARTESIAN_POINT ( 'NONE',  ( -74.27155067695211699, -273.3801315311856115, -207.3328386040565761 ) ) ;
#11862 = CARTESIAN_POINT ( 'NONE',  ( -74.86696263462846446, -287.5693706703454495, -335.7083556989466615 ) ) ;
#11864 = CARTESIAN_POINT ( 'NONE',  ( 22.09017432804451531, -286.8943748884699971, -221.4034597600582401 ) ) ;
#11865 = CARTESIAN_POINT ( 'NONE',  ( -4.345976336065635159, -288.2958086325601812, -339.9243277616816385 ) ) ;
#11866 = CARTESIAN_POINT ( 'NONE',  ( -109.2513031221235451, -298.8232467559110432, -247.6620655784195435 ) ) ;
#11867 = CARTESIAN_POINT ( 'NONE',  ( -38.39297099805281022, -293.0652040566474739, -345.1870711011701474 ) ) ;
#11868 = CARTESIAN_POINT ( 'NONE',  ( 22.39126835378041847, -281.3990173969403941, -318.7154159960040829 ) ) ;
#11869 = EDGE_CURVE ( 'NONE', #70, #69962, #18718, .T. ) ;
#11870 = LINE ( 'NONE', #18501, #10854 ) ;
#11871 = CARTESIAN_POINT ( 'NONE',  ( -111.5124260985978992, -276.6958976484647224, -259.1533272852826713 ) ) ;
#11872 = FACE_OUTER_BOUND ( 'NONE', #64731, .T. ) ;
#11873 = CARTESIAN_POINT ( 'NONE',  ( -66.50082156175574255, -288.2375346325468968, -337.7717712545001518 ) ) ;
#11874 = CARTESIAN_POINT ( 'NONE',  ( 159.4851178187871312, 3.000000000000000000, -9.000000000000001776 ) ) ;
#11875 = DIRECTION ( 'NONE',  ( 0.9531768234071978929, -0.3024135303179465439, -0.000000000000000000 ) ) ;
#11876 = CARTESIAN_POINT ( 'NONE',  ( -75.76173359790544737, -287.5647585581627936, -334.7881783211586253 ) ) ;
#11877 = CARTESIAN_POINT ( 'NONE',  ( -52.82257436235986603, -299.4507331487625379, -198.1506198083567654 ) ) ;
#11878 = CARTESIAN_POINT ( 'NONE',  ( 37.84903145169399608, -283.1497351497974932, -284.0338941800599173 ) ) ;
#11880 = CARTESIAN_POINT ( 'NONE',  ( -106.1737312355437126, -284.2267880142716763, -294.8252525044101731 ) ) ;
#11879 = CARTESIAN_POINT ( 'NONE',  ( -36.88335263032297462, -296.0779758395780163, -195.0060632432097236 ) ) ;
#11881 = CARTESIAN_POINT ( 'NONE',  ( -62.24603790994116537, -275.1470580657255596, -201.1141044985861015 ) ) ;
#11882 = CARTESIAN_POINT ( 'NONE',  ( -36.79343992032838884, -282.0592019801688366, -195.3504113958989876 ) ) ;
#11884 = CARTESIAN_POINT ( 'NONE',  ( -55.33992824315551928, -296.8737459230746367, -199.3194009591837528 ) ) ;
#11883 = CIRCLE ( 'NONE', #88986, 8.222204860432944074 ) ;
#11885 = ORIENTED_EDGE ( 'NONE', *, *, #2379, .T. ) ;
#11886 = FACE_OUTER_BOUND ( 'NONE', #77346, .T. ) ;
#11887 = CARTESIAN_POINT ( 'NONE',  ( -13.78406194055809664, -294.5879634934768774, -343.6689462652067846 ) ) ;
#11888 = CARTESIAN_POINT ( 'NONE',  ( -109.6276565220233579, -286.7723836883359354, -251.7442623429170681 ) ) ;
#11889 = LINE ( 'NONE', #33666, #51849 ) ;
#11890 = CARTESIAN_POINT ( 'NONE',  ( -2.659677404128736544, -280.1237833571632336, -342.4524372437778652 ) ) ;
#11891 = CARTESIAN_POINT ( 'NONE',  ( -41.38619084396332681, -276.2990005151955302, -347.1063061983342095 ) ) ;
#11892 = EDGE_CURVE ( 'NONE', #56772, #70448, #23866, .T. ) ;
#11893 = CARTESIAN_POINT ( 'NONE',  ( -110.7765126455665978, -288.6945117161553753, -290.7024239173342721 ) ) ;
#11894 = CARTESIAN_POINT ( 'NONE',  ( 12.39879054353536958, -283.8642601007659323, -324.7356647737787512 ) ) ;
#11895 = CARTESIAN_POINT ( 'NONE',  ( -13.43720181756111565, -278.4977468912605900, -340.4617628390448658 ) ) ;
#11896 = CARTESIAN_POINT ( 'NONE',  ( -31.66183847170702492, -284.4070772694444145, -346.5736641192407888 ) ) ;
#11897 = CARTESIAN_POINT ( 'NONE',  ( -104.4826819890446075, -282.9501992718563770, -300.0127462419482640 ) ) ;
#11898 = CARTESIAN_POINT ( 'NONE',  ( -80.21855741976330023, -281.4716564336793567, -208.8259592917643204 ) ) ;
#11899 = CARTESIAN_POINT ( 'NONE',  ( -15.77939409296619289, -274.4901564271136749, -196.3864521335050313 ) ) ;
#11900 = CARTESIAN_POINT ( 'NONE',  ( -69.01731485000155430, -277.2906191478002143, -340.5585366834978345 ) ) ;
#11901 = CARTESIAN_POINT ( 'NONE',  ( -66.59698157317149025, -297.3585213228496968, -338.8114116806738707 ) ) ;
#11902 = PLANE ( 'NONE',  #52058 ) ;
#11903 = CARTESIAN_POINT ( 'NONE',  ( 153.1590225954906543, 19.71789692321348397, -10.20076944887112269 ) ) ;
#11904 = CARTESIAN_POINT ( 'NONE',  ( -92.80172060689096725, -293.9765023789503289, -321.9989462706197969 ) ) ;
#11905 = CARTESIAN_POINT ( 'NONE',  ( -1.445459428485909248, -276.0704572094677474, -334.0536412462648741 ) ) ;
#11906 = CARTESIAN_POINT ( 'NONE',  ( -36.55841889359908237, -299.1414084624087195, -193.6700876241062872 ) ) ;
#11907 = CARTESIAN_POINT ( 'NONE',  ( -7.871784015579938121, -288.2038361082733786, -202.4678336343174578 ) ) ;
#11908 = CARTESIAN_POINT ( 'NONE',  ( 37.08075170875183346, -294.8589223784181286, -253.4501109912460493 ) ) ;
#11909 = CARTESIAN_POINT ( 'NONE',  ( 31.87783838519173685, -295.1812889064271417, -303.2973836299144637 ) ) ;
#11910 = CARTESIAN_POINT ( 'NONE',  ( -105.7126183004163664, -292.1513018800488908, -300.9101353951804754 ) ) ;
#11911 = CARTESIAN_POINT ( 'NONE',  ( -46.66011258465849210, -277.9335628587383553, -196.0578377145540969 ) ) ;
#11912 = CARTESIAN_POINT ( 'NONE',  ( -97.58519442977799940, -281.0723888527524537, -226.6342887573707969 ) ) ;
#11913 = CARTESIAN_POINT ( 'NONE',  ( -101.4182199183619133, -294.1202938809319676, -308.3508446733941923 ) ) ;
#11914 = CARTESIAN_POINT ( 'NONE',  ( 6.234265778095955390, -284.3283624284052280, -332.4046432469247065 ) ) ;
#11915 = CARTESIAN_POINT ( 'NONE',  ( -8.119147141539352575, -285.3644825102141453, -203.1281761218491511 ) ) ;
#11916 = CARTESIAN_POINT ( 'NONE',  ( -75.84180017535200591, -209.4652300186797049, -356.3057796646524480 ) ) ;
#11917 = VERTEX_POINT ( 'NONE', #16764 ) ;
#11918 = CARTESIAN_POINT ( 'NONE',  ( -97.37090427723909158, -284.7982187592184005, -228.7627968174912496 ) ) ;
#11919 = ORIENTED_EDGE ( 'NONE', *, *, #62384, .F. ) ;
#11920 = CARTESIAN_POINT ( 'NONE',  ( 4.389075172492190369, -283.5835164434987519, -334.7669925542786018 ) ) ;
#11921 = CARTESIAN_POINT ( 'NONE',  ( -59.48609328469245838, -274.0907847944768037, -200.7257587572469788 ) ) ;
#11922 = CARTESIAN_POINT ( 'NONE',  ( -63.05363600282146308, -284.5195216888135405, -198.2022302990849880 ) ) ;
#11923 = CARTESIAN_POINT ( 'NONE',  ( 29.07698386091632514, -281.9913298667300978, -231.8724361448573745 ) ) ;
#11924 = CARTESIAN_POINT ( 'NONE',  ( 195.4663476211042052, 20.04167166511072651, -14.69138476959436623 ) ) ;
#11925 = CARTESIAN_POINT ( 'NONE',  ( -31.14950356325812564, -281.6490172806020382, -194.2538922277914537 ) ) ;
#11926 = CARTESIAN_POINT ( 'NONE',  ( -1.190700509482957470, -281.1704389952192287, -202.4905204206547751 ) ) ;
#11927 = CARTESIAN_POINT ( 'NONE',  ( -37.37352853689063181, -286.5523547857346784, -340.3611179825599606 ) ) ;
#11928 = CARTESIAN_POINT ( 'NONE',  ( -38.73072492404651257, -140.1446639439760702, -364.8181740665336292 ) ) ;
#11929 = ORIENTED_EDGE ( 'NONE', *, *, #46756, .F. ) ;
#11930 = CARTESIAN_POINT ( 'NONE',  ( -67.82711616010269040, -275.6512994770065461, -202.0047941750336520 ) ) ;
#11931 = CARTESIAN_POINT ( 'NONE',  ( -31.67332922037059006, -124.0639957142015533, -364.0958594919561051 ) ) ;
#11932 = CARTESIAN_POINT ( 'NONE',  ( -105.9440327837278915, -276.9587884342035977, -240.9406021121017147 ) ) ;
#11933 = CARTESIAN_POINT ( 'NONE',  ( -37.81155663608277706, -293.8064773571610999, -194.3759006540348935 ) ) ;
#11934 = CARTESIAN_POINT ( 'NONE',  ( -97.27169148441737434, -295.3178765231755278, -312.2214668146835379 ) ) ;
#11935 = CARTESIAN_POINT ( 'NONE',  ( -90.73871056436745164, -290.8272698274044501, -214.8950699995339733 ) ) ;
#11936 = DIRECTION ( 'NONE',  ( 0.000000000000000000, 0.000000000000000000, 1.000000000000000000 ) ) ;
#11938 = CARTESIAN_POINT ( 'NONE',  ( 32.60525647443726882, -285.6427788552146581, -246.8268094768048115 ) ) ;
#11937 = CARTESIAN_POINT ( 'NONE',  ( -106.6396837845702237, -294.7116974572602430, -302.5542189893770342 ) ) ;
#11939 = CARTESIAN_POINT ( 'NONE',  ( 22.79158483978172356, -294.8134448020422269, -226.8095953903694806 ) ) ;
#11940 = CARTESIAN_POINT ( 'NONE',  ( 33.55319126898695714, -286.4933798103258482, -289.9187965230924533 ) ) ;
#11941 = CARTESIAN_POINT ( 'NONE',  ( -92.92116950648502893, -285.1865728186486990, -318.4652515098845811 ) ) ;
#11942 = ORIENTED_EDGE ( 'NONE', *, *, #22600, .T. ) ;
#11943 = CARTESIAN_POINT ( 'NONE',  ( -50.53772762970902477, -292.8288226814275390, -194.7391299729637808 ) ) ;
#11944 = CARTESIAN_POINT ( 'NONE',  ( 13.97236240340401814, -282.8008410370684942, -322.4405811189353130 ) ) ;
#11945 = CARTESIAN_POINT ( 'NONE',  ( -102.7843733399455743, -294.8245010074130619, -310.1765074795446822 ) ) ;
#11946 = CARTESIAN_POINT ( 'NONE',  ( -82.74897544549313011, -290.4583979378410845, -332.3477146650190548 ) ) ;
#11947 = CARTESIAN_POINT ( 'NONE',  ( -11.18007883237300604, -292.8763495210278052, -197.9511605447531508 ) ) ;
#11948 = CARTESIAN_POINT ( 'NONE',  ( 33.38803480352928688, -287.4797993331431485, -252.2467664456233933 ) ) ;
#11949 = ORIENTED_EDGE ( 'NONE', *, *, #24378, .T. ) ;
#11950 = CARTESIAN_POINT ( 'NONE',  ( 223.4306832106270804, -141.7221692137691775, -21.50000000000000000 ) ) ;
#11951 = CARTESIAN_POINT ( 'NONE',  ( -96.42900093387635252, -297.7665343754947003, -317.8052274613804684 ) ) ;
#11952 = CARTESIAN_POINT ( 'NONE',  ( -84.89671618182417490, -296.0964742166052588, -210.4293340983272742 ) ) ;
#11953 = CARTESIAN_POINT ( 'NONE',  ( 27.99671797459161482, -280.1618587805434117, -237.1684379888619674 ) ) ;
#11954 = ORIENTED_EDGE ( 'NONE', *, *, #41498, .T. ) ;
#11955 = CARTESIAN_POINT ( 'NONE',  ( 35.14088228149329041, -275.3874989983887076, -296.3212588594157637 ) ) ;
#11956 = VECTOR ( 'NONE', #88714, 1000.000000000000000 ) ;
#11957 = CARTESIAN_POINT ( 'NONE',  ( -110.9032408041161091, -295.0895906233503183, -265.9557253485581327 ) ) ;
#11958 = CARTESIAN_POINT ( 'NONE',  ( -51.49354218856608156, -279.0954822059095477, -343.2349187883628474 ) ) ;
#11959 = CARTESIAN_POINT ( 'NONE',  ( -27.09665949279046160, -272.3231992950544509, -196.7844998258825342 ) ) ;
#11960 = CARTESIAN_POINT ( 'NONE',  ( -18.10171823212836273, -296.0036361283404176, -341.1915747111040673 ) ) ;
#11961 = CARTESIAN_POINT ( 'NONE',  ( -63.20132276407057503, -298.7870346821795238, -201.7107164865911102 ) ) ;
#11962 = LINE ( 'NONE', #19997, #14298 ) ;
#11963 = CARTESIAN_POINT ( 'NONE',  ( -48.86929473770263144, -299.5079330296687203, -194.9850034571304320 ) ) ;
#11964 = CARTESIAN_POINT ( 'NONE',  ( -56.88783298730761118, -295.8006349718829142, -197.7263289338401933 ) ) ;
#11965 = CARTESIAN_POINT ( 'NONE',  ( -28.10167507329012437, -292.8238083442508355, -197.7946828861999791 ) ) ;
#11966 = CARTESIAN_POINT ( 'NONE',  ( -94.73917262081765500, -289.7727667268370624, -224.2878146096032594 ) ) ;
#11967 = CARTESIAN_POINT ( 'NONE',  ( 209.0355956570440412, 30.15830632019625313, 14.26380412825890787 ) ) ;
#11968 = CARTESIAN_POINT ( 'NONE',  ( -0.08074427398172294434, -275.0265562188263289, -203.0323343567650909 ) ) ;
#11969 = CARTESIAN_POINT ( 'NONE',  ( -103.2059893864593931, -273.1445513411402430, -238.8826268342931201 ) ) ;
#11970 = CARTESIAN_POINT ( 'NONE',  ( 9.774517450236274385, -282.6765479314079812, -211.4855070770204577 ) ) ;
#11971 = CARTESIAN_POINT ( 'NONE',  ( -52.83422942530944511, -281.9313824124492385, -345.3370881873298686 ) ) ;
#11972 = CARTESIAN_POINT ( 'NONE',  ( -2.778368391850212671, -275.9559438820924129, -339.0684893653298104 ) ) ;
#11973 = CARTESIAN_POINT ( 'NONE',  ( -103.1623985106912613, -283.3164742530137232, -302.4186551696149081 ) ) ;
#11974 = CARTESIAN_POINT ( 'NONE',  ( 37.58628065862232148, -279.4753064740824016, -264.3756255478745061 ) ) ;
#11975 = CARTESIAN_POINT ( 'NONE',  ( -93.35054011315504852, -271.8005968509393711, -222.6092437142021367 ) ) ;
#11976 = CARTESIAN_POINT ( 'NONE',  ( -112.2711749018781546, -280.6072150155323470, -266.0855091339631144 ) ) ;
#11977 = DIRECTION ( 'NONE',  ( 1.000000000000000000, 0.000000000000000000, 0.000000000000000000 ) ) ;
#11978 = DIRECTION ( 'NONE',  ( -0.2456588035076248677, 0.9693563597868444237, 0.000000000000000000 ) ) ;
#11979 = CARTESIAN_POINT ( 'NONE',  ( -67.75106180120246790, -295.8985455865802123, -200.6685581360634103 ) ) ;
#11980 = CARTESIAN_POINT ( 'NONE',  ( 30.21892019334217849, -277.9870224707883040, -303.4280633812549581 ) ) ;
#11981 = CARTESIAN_POINT ( 'NONE',  ( 20.55867556936468077, -272.8944578681928874, -222.6898777343884888 ) ) ;
#11982 = CARTESIAN_POINT ( 'NONE',  ( 140.6539576904058606, 275.0000000000000568, 12.50000000000000000 ) ) ;
#11983 = CARTESIAN_POINT ( 'NONE',  ( -110.8131001222128162, -286.2467500528933897, -288.0585939169493486 ) ) ;
#11984 = ORIENTED_EDGE ( 'NONE', *, *, #67622, .F. ) ;
#11985 = FACE_OUTER_BOUND ( 'NONE', #85658, .T. ) ;
#11986 = CARTESIAN_POINT ( 'NONE',  ( 6.047021010661475238, -286.4638105083834034, -331.5991299858230263 ) ) ;
#11987 = CARTESIAN_POINT ( 'NONE',  ( 156.4947056272797852, 21.00000000000000000, 15.00000000000000000 ) ) ;
#11988 = CARTESIAN_POINT ( 'NONE',  ( -0.5722527155605370286, -293.3471525912123639, -333.9418572773470260 ) ) ;
#11989 = CARTESIAN_POINT ( 'NONE',  ( 22.95130391865977515, -286.2871191324499591, -313.6695368501304984 ) ) ;
#11990 = CARTESIAN_POINT ( 'NONE',  ( -82.08396892746139883, -205.6231916066184624, -355.0661004095303497 ) ) ;
#11991 = CARTESIAN_POINT ( 'NONE',  ( -96.36268795855517055, -293.9168872256790905, -316.6377173474196525 ) ) ;
#11992 = CARTESIAN_POINT ( 'NONE',  ( -97.02588882726561792, -283.6743962815139071, -222.8163456593140666 ) ) ;
#11993 = CARTESIAN_POINT ( 'NONE',  ( 9.771765009306662364, -282.3131028808741121, -213.4899239032754394 ) ) ;
#11994 = CARTESIAN_POINT ( 'NONE',  ( -3.677768561452260165, -287.6915676875727286, -201.5371584017965461 ) ) ;
#11995 = CARTESIAN_POINT ( 'NONE',  ( 37.42443782884210890, -279.9648363296811340, -283.9978842131654915 ) ) ;
#11996 = CARTESIAN_POINT ( 'NONE',  ( -34.57800184039527380, -289.0166003900959026, -343.3583656645191695 ) ) ;
#11997 = CARTESIAN_POINT ( 'NONE',  ( -22.08986493811561047, -281.6765148138701989, -198.3174808447351722 ) ) ;
#11998 = CARTESIAN_POINT ( 'NONE',  ( -3.082510429314294420, -281.3197669460260499, -205.7024231446197859 ) ) ;
#11999 = EDGE_CURVE ( 'NONE', #51424, #33982, #28195, .T. ) ;
#12000 = CARTESIAN_POINT ( 'NONE',  ( 35.10280011080594420, -289.2642166040210441, -249.4347683480205831 ) ) ;
#12001 = ORIENTED_EDGE ( 'NONE', *, *, #33757, .T. ) ;
#12002 = CARTESIAN_POINT ( 'NONE',  ( -113.8626674886053678, -272.6594023460276617, -261.7854807345403856 ) ) ;
#12003 = CARTESIAN_POINT ( 'NONE',  ( -74.33876776348557769, -291.5264750778824805, -335.2068920707291113 ) ) ;
#12004 = CARTESIAN_POINT ( 'NONE',  ( 169.7306087885279453, 275.5000000000000568, -24.89999999999999147 ) ) ;
#12005 = CARTESIAN_POINT ( 'NONE',  ( -69.91165696735023971, -276.1233781216988064, -202.8022627189028810 ) ) ;
#12006 = ORIENTED_EDGE ( 'NONE', *, *, #51325, .T. ) ;
#12007 = CARTESIAN_POINT ( 'NONE',  ( -20.56077931937331726, -274.8371346808540352, -343.6840942699477637 ) ) ;
#12008 = CARTESIAN_POINT ( 'NONE',  ( 198.5113747970946179, 66.01554725018998226, 10.78125329330598348 ) ) ;
#12009 = CARTESIAN_POINT ( 'NONE',  ( -61.35894570803728243, -293.7587048365227247, -342.7323422057019116 ) ) ;
#12010 = CARTESIAN_POINT ( 'NONE',  ( -93.65699342930312810, -296.7193012729372867, -223.7951624828971546 ) ) ;
#12011 = CARTESIAN_POINT ( 'NONE',  ( -39.96340923975267856, -290.6056837565198521, -344.0578511618480206 ) ) ;
#12012 = CARTESIAN_POINT ( 'NONE',  ( 8.438090839920427300, -284.1760635549513836, -328.5831412016553372 ) ) ;
#12013 = CARTESIAN_POINT ( 'NONE',  ( -108.2449011334998090, -291.6131318147539560, -298.8451903521631721 ) ) ;
#12014 = CARTESIAN_POINT ( 'NONE',  ( -111.0622698857904993, -291.6093430813161262, -290.8202447521590557 ) ) ;
#12015 = CARTESIAN_POINT ( 'NONE',  ( -3.720211904967436922, -288.4959754508652736, -203.3193684354497748 ) ) ;
#12016 = CARTESIAN_POINT ( 'NONE',  ( -73.76751629861605863, -279.7489066921709195, -202.5069459657786695 ) ) ;
#12017 = CARTESIAN_POINT ( 'NONE',  ( -109.4333787901076533, -294.3417296020811023, -293.0341870494128216 ) ) ;
#12018 = CARTESIAN_POINT ( 'NONE',  ( -52.91968858602928805, -283.0796915706076788, -345.8233438824149175 ) ) ;
#12019 = CARTESIAN_POINT ( 'NONE',  ( 33.70532038733049518, -277.6933128490790068, -291.9269958120816568 ) ) ;
#12020 = EDGE_CURVE ( 'NONE', #10127, #44168, #24728, .T. ) ;
#12021 = CARTESIAN_POINT ( 'NONE',  ( -107.3452863284742449, -275.1604526064901393, -262.5058405983616012 ) ) ;
#12022 = AXIS2_PLACEMENT_3D ( 'NONE', #16185, #65944, #52612 ) ;
#12023 = CARTESIAN_POINT ( 'NONE',  ( 29.07289954989624192, -273.3058408325565551, -233.3330177788781725 ) ) ;
#12024 = CARTESIAN_POINT ( 'NONE',  ( 194.7510731661265595, -143.7221692137691775, -21.50000000000000000 ) ) ;
#12025 = CARTESIAN_POINT ( 'NONE',  ( -5.526034681492270728, -279.9900228883731756, -204.5906696483962151 ) ) ;
#12026 = CARTESIAN_POINT ( 'NONE',  ( -97.60697025100625979, -279.1217732958113515, -317.6485998084235689 ) ) ;
#12027 = AXIS2_PLACEMENT_3D ( 'NONE', #47486, #46093, #82550 ) ;
#12028 = CARTESIAN_POINT ( 'NONE',  ( -54.89911711056387134, -284.8904909920424302, -195.6312222166651509 ) ) ;
#12029 = CARTESIAN_POINT ( 'NONE',  ( -17.17776363783582738, -294.0760283630731351, -199.0941106353228065 ) ) ;
#12030 = CARTESIAN_POINT ( 'NONE',  ( 22.12114468027513681, -276.5070288106356884, -222.6895104939444252 ) ) ;
#12031 = CARTESIAN_POINT ( 'NONE',  ( -24.26050937830338938, -275.5308541059839627, -194.9270596098099020 ) ) ;
#12032 = DIRECTION ( 'NONE',  ( -0.000000000000000000, 0.000000000000000000, -1.000000000000000000 ) ) ;
#12033 = CARTESIAN_POINT ( 'NONE',  ( 23.98323269371284638, -275.9348189188465312, -310.0554889903755225 ) ) ;
#12034 = CARTESIAN_POINT ( 'NONE',  ( -110.6763679830202989, -298.3597315934669609, -285.3263355785745716 ) ) ;
#12035 = CARTESIAN_POINT ( 'NONE',  ( -37.25377280838804239, -284.0530614498246109, -195.5150814858104980 ) ) ;
#12036 = CARTESIAN_POINT ( 'NONE',  ( 1.693041237821428568, -292.2255401779535191, -203.9523791118493534 ) ) ;
#12037 = CARTESIAN_POINT ( 'NONE',  ( 22.13250329715412335, -274.1922227026672090, -315.4683893789126614 ) ) ;
#12038 = CARTESIAN_POINT ( 'NONE',  ( -7.217242680788439557, -290.2637008478211555, -340.3677651890384936 ) ) ;
#12039 = CARTESIAN_POINT ( 'NONE',  ( -28.05361346976921411, -291.0930025974869864, -197.5918104978125882 ) ) ;
#12040 = ORIENTED_EDGE ( 'NONE', *, *, #6789, .F. ) ;
#12041 = CARTESIAN_POINT ( 'NONE',  ( 24.34954572478147128, -291.5237045862518812, -225.2745736584487872 ) ) ;
#12042 = CARTESIAN_POINT ( 'NONE',  ( -102.4264875098985783, -290.6697245900886060, -237.1424351068653209 ) ) ;
#12043 = EDGE_LOOP ( 'NONE', ( #77514, #31253 ) ) ;
#12044 = CARTESIAN_POINT ( 'NONE',  ( 32.42508598765144257, -288.2216390095728684, -238.3885792133189909 ) ) ;
#12045 = CARTESIAN_POINT ( 'NONE',  ( -64.82800983640910886, -280.0162774585989496, -202.7106171313166953 ) ) ;
#12046 = CARTESIAN_POINT ( 'NONE',  ( 4.048852894904261923, -293.4292338567008755, -334.9861218836370540 ) ) ;
#12047 = CARTESIAN_POINT ( 'NONE',  ( -83.22171987203101651, -286.0938626919149783, -208.5829895882328913 ) ) ;
#12048 = CARTESIAN_POINT ( 'NONE',  ( 35.82760768382338057, -287.5825273056528317, -246.2742231218383893 ) ) ;
#12049 = CARTESIAN_POINT ( 'NONE',  ( 18.51327032795031258, -282.5535809824711464, -317.4157264960379621 ) ) ;
#12050 = CARTESIAN_POINT ( 'NONE',  ( 5.697525119581973385, -58.35050878906803007, -354.7899736438976106 ) ) ;
#12051 = CARTESIAN_POINT ( 'NONE',  ( -91.01950653586207807, -229.5109285105102117, -346.8848101179228252 ) ) ;
#12052 = CARTESIAN_POINT ( 'NONE',  ( 187.9541643320069113, 268.7763698351266157, -137.5712847132034540 ) ) ;
#12053 = CARTESIAN_POINT ( 'NONE',  ( 7.437794970279090201, -273.8781792905782595, -212.5044109801810919 ) ) ;
#12054 = CARTESIAN_POINT ( 'NONE',  ( -40.53292591936764211, -276.0135128299020266, -343.6132564228390152 ) ) ;
#12055 = CARTESIAN_POINT ( 'NONE',  ( -99.03933312968028702, -296.6719276773890783, -224.3725246228790127 ) ) ;
#12056 = CARTESIAN_POINT ( 'NONE',  ( 180.7906440682407663, 251.0613717956916560, -164.6901867084850437 ) ) ;
#12057 = CARTESIAN_POINT ( 'NONE',  ( 36.40575605637703660, -274.4942664410054363, -290.7719250130335809 ) ) ;
#12058 = CARTESIAN_POINT ( 'NONE',  ( -68.73247420903742011, -275.3939662924613003, -203.3204180578236162 ) ) ;
#12059 = EDGE_LOOP ( 'NONE', ( #52244, #91910 ) ) ;
#12060 = CARTESIAN_POINT ( 'NONE',  ( -14.90765706747966490, -299.2678316286620657, -193.5929225309962476 ) ) ;
#12061 = CARTESIAN_POINT ( 'NONE',  ( 28.28578510267488610, -288.4790709341182264, -302.4706434188188950 ) ) ;
#12062 = CARTESIAN_POINT ( 'NONE',  ( -56.02111412153313807, -296.0896449586250583, -344.8945890734977979 ) ) ;
#12063 = CARTESIAN_POINT ( 'NONE',  ( -114.3044827737108875, -297.0180482407640170, -272.4743640083499940 ) ) ;
#12064 = CARTESIAN_POINT ( 'NONE',  ( 31.54075996821940109, -294.0422162593171151, -294.6828556138995054 ) ) ;
#12065 = VERTEX_POINT ( 'NONE', #81159 ) ;
#12066 = CARTESIAN_POINT ( 'NONE',  ( 21.53464059610251624, -278.1192746915972407, -317.7407597516067312 ) ) ;
#12067 = EDGE_LOOP ( 'NONE', ( #24580, #17667, #8430, #49991 ) ) ;
#12068 = CARTESIAN_POINT ( 'NONE',  ( -48.10396624039731961, -279.4265218701735307, -194.1252946922032834 ) ) ;
#12069 = CARTESIAN_POINT ( 'NONE',  ( -78.75521430402318401, -278.5663156721249720, -330.8242638033912613 ) ) ;
#12070 = CARTESIAN_POINT ( 'NONE',  ( 14.21235068436446625, -278.1002765565810364, -326.2552728451562984 ) ) ;
#12071 = CARTESIAN_POINT ( 'NONE',  ( -111.6807755903653998, -276.4146507069258973, -282.6943520841978739 ) ) ;
#12072 = CARTESIAN_POINT ( 'NONE',  ( -96.18730163186943116, -297.8108117375129495, -226.9684720651976306 ) ) ;
#12073 = CARTESIAN_POINT ( 'NONE',  ( -75.98278277568226713, -294.1536051859461622, -333.0483368961862425 ) ) ;
#12074 = DIRECTION ( 'NONE',  ( -0.9693563597868444237, -0.2456588035076248677, 0.000000000000000000 ) ) ;
#12075 = CARTESIAN_POINT ( 'NONE',  ( -6.260979659944867493, -280.9419849285802115, -199.9656407025799467 ) ) ;
#12076 = CARTESIAN_POINT ( 'NONE',  ( -93.09157462559910812, -279.3887618167108258, -223.2149169268290620 ) ) ;
#12077 = CARTESIAN_POINT ( 'NONE',  ( 23.73832545172015784, -286.8544458745618044, -316.4320279948617554 ) ) ;
#12078 = CARTESIAN_POINT ( 'NONE',  ( -35.89847248428284843, -300.0703343395864522, -195.1939519473317262 ) ) ;
#12079 = FACE_OUTER_BOUND ( 'NONE', #536, .T. ) ;
#12080 = CARTESIAN_POINT ( 'NONE',  ( -78.27320510520871721, -288.8152378342200564, -331.0621457637079175 ) ) ;
#12081 = CARTESIAN_POINT ( 'NONE',  ( -11.36680714482212551, -278.6349657166464908, -201.0012190010811253 ) ) ;
#12083 = CARTESIAN_POINT ( 'NONE',  ( -15.73748276506246846, -280.8502940522446352, -341.5971481064415229 ) ) ;
#12082 = CARTESIAN_POINT ( 'NONE',  ( -39.70209396986417261, -278.5966893481790976, -196.7971308432429680 ) ) ;
#12085 = CARTESIAN_POINT ( 'NONE',  ( 14.10028829397946737, -288.7740956177092357, -215.7133758892978790 ) ) ;
#12084 = AXIS2_PLACEMENT_3D ( 'NONE', #75709, #89904, #25513 ) ;
#12086 = CARTESIAN_POINT ( 'NONE',  ( -92.51702009879923594, -280.4445017572029428, -221.9393641559117896 ) ) ;
#12087 = CARTESIAN_POINT ( 'NONE',  ( 153.3642062430809858, 20.33187285098938091, -12.12209853637909696 ) ) ;
#12088 = CARTESIAN_POINT ( 'NONE',  ( -7.996835274825064843, -294.4366931725923564, -201.3263074816831306 ) ) ;
#12089 = CARTESIAN_POINT ( 'NONE',  ( -45.56256277481169548, -275.3946948587646943, -345.9541394910341978 ) ) ;
#12090 = CIRCLE ( 'NONE', #10592, 2.939656322713313230 ) ;
#12091 = CARTESIAN_POINT ( 'NONE',  ( 3.197517151241683564, -277.1428203115000883, -331.1925615817715425 ) ) ;
#12092 = CARTESIAN_POINT ( 'NONE',  ( -49.76481145806104678, -285.2102801587333829, -344.5466612843584358 ) ) ;
#12093 = CARTESIAN_POINT ( 'NONE',  ( 157.7374095173865385, 14.19731191252289015, 13.00000000000000178 ) ) ;
#12094 = CARTESIAN_POINT ( 'NONE',  ( -88.49825579899042793, -291.6830222655178773, -325.9697594667278508 ) ) ;
#12095 = CARTESIAN_POINT ( 'NONE',  ( -111.9921130698222669, -294.4525742150585188, -278.1037617474970034 ) ) ;
#12096 = CARTESIAN_POINT ( 'NONE',  ( 38.62747359294239402, -286.6037749383541495, -258.7476642976691323 ) ) ;
#12097 = CARTESIAN_POINT ( 'NONE',  ( 180.0056393205866812, 275.0000000000000568, -23.52000000000002800 ) ) ;
#12098 = CARTESIAN_POINT ( 'NONE',  ( -24.49386947443048967, -272.9042454923451260, -197.9477477540017105 ) ) ;
#12099 = CARTESIAN_POINT ( 'NONE',  ( 34.30267206218994147, -291.9448418601630806, -289.8503127165409410 ) ) ;
#12100 = PRESENTATION_STYLE_ASSIGNMENT (( #90668 ) ) ;
#12101 = DIRECTION ( 'NONE',  ( 0.000000000000000000, 0.000000000000000000, 1.000000000000000000 ) ) ;
#12102 = CARTESIAN_POINT ( 'NONE',  ( -88.17308651892729188, -289.8354375658416870, -213.4499775204312186 ) ) ;
#12103 = CARTESIAN_POINT ( 'NONE',  ( -65.41622508650461043, -287.2791818744134957, -202.0552552028171078 ) ) ;
#12104 = CARTESIAN_POINT ( 'NONE',  ( 36.39894947718684648, -285.5595333313642641, -252.0228898107602618 ) ) ;
#12105 = CARTESIAN_POINT ( 'NONE',  ( -107.9522164552924721, -285.7048899173073551, -291.1311737325640934 ) ) ;
#12106 = CARTESIAN_POINT ( 'NONE',  ( 123.4306832106270946, -178.2391364535880882, -4.999999999999990230 ) ) ;
#12107 = CARTESIAN_POINT ( 'NONE',  ( -96.71183582797749523, -285.9517544706959029, -227.5870964547588642 ) ) ;
#12108 = EDGE_CURVE ( 'NONE', #2466, #78327, #51341, .T. ) ;
#12109 = CARTESIAN_POINT ( 'NONE',  ( -5.326349165420787735, -294.4512190947503996, -202.1451073256325230 ) ) ;
#12110 = CARTESIAN_POINT ( 'NONE',  ( 22.36485730461436816, -274.2623918198684692, -316.6902055586546680 ) ) ;
#12111 = CARTESIAN_POINT ( 'NONE',  ( 39.29583067753333836, -275.7880703290786073, -262.5782603437717739 ) ) ;
#12112 = CARTESIAN_POINT ( 'NONE',  ( 3.386338600675487420, -290.6744581830073457, -206.6552262671307574 ) ) ;
#12113 = CARTESIAN_POINT ( 'NONE',  ( -59.30214201170247890, -279.7754927335259367, -196.5590923174327429 ) ) ;
#12114 = CARTESIAN_POINT ( 'NONE',  ( -53.48097994725340243, -297.2399588052111881, -343.2934199162808113 ) ) ;
#12115 = CARTESIAN_POINT ( 'NONE',  ( -43.53450001092989652, -248.8289484981847863, -480.0790493083237607 ) ) ;
#12116 = CARTESIAN_POINT ( 'NONE',  ( 208.0457363859825932, 36.70443730966733398, 13.54762445178161556 ) ) ;
#12117 = CARTESIAN_POINT ( 'NONE',  ( -67.73646410636035853, -284.3295090226798720, -203.4477276778946759 ) ) ;
#12118 = CARTESIAN_POINT ( 'NONE',  ( 18.65292621928355743, -278.8573599138828740, -220.4458830727914176 ) ) ;
#12119 = DIRECTION ( 'NONE',  ( 0.000000000000000000, 0.000000000000000000, 1.000000000000000000 ) ) ;
#12120 = CARTESIAN_POINT ( 'NONE',  ( 13.51692020822867590, -273.2285297687224670, -213.4036866298212658 ) ) ;
#12121 = CARTESIAN_POINT ( 'NONE',  ( -32.42197374866186976, -276.3372129110847482, -343.3473521264460828 ) ) ;
#12122 = CARTESIAN_POINT ( 'NONE',  ( -47.87316328768768869, -296.7085001218731577, -343.3498152119228166 ) ) ;
#12123 = CARTESIAN_POINT ( 'NONE',  ( 1.230447900359898927, -279.4745957653457822, -204.0157968305569796 ) ) ;
#12124 = CARTESIAN_POINT ( 'NONE',  ( -18.14732858763413503, -295.7398548508115823, -341.0363226063383308 ) ) ;
#12125 = CARTESIAN_POINT ( 'NONE',  ( -107.9136246579931964, -297.4875592714385562, -300.0430711448337320 ) ) ;
#12126 = CARTESIAN_POINT ( 'NONE',  ( -104.3974404178966608, -272.6087385816778692, -241.3259865658003207 ) ) ;
#12127 = CARTESIAN_POINT ( 'NONE',  ( -76.03261901806769174, -293.5358917652077366, -206.0508561117189288 ) ) ;
#12128 = CARTESIAN_POINT ( 'NONE',  ( -29.46504789154979420, -286.3159943636675848, -193.7650452761536712 ) ) ;
#12129 = CARTESIAN_POINT ( 'NONE',  ( 36.38432931418959271, -273.9142899411396002, -287.8748182233948114 ) ) ;
#12130 = CARTESIAN_POINT ( 'NONE',  ( 35.94710223975818053, -287.6824663743896053, -293.9778800805364085 ) ) ;
#12131 = CARTESIAN_POINT ( 'NONE',  ( -111.6051648534035792, -280.6356769159129954, -262.3285223940375772 ) ) ;
#12132 = ADVANCED_FACE ( 'NONE', ( #44233 ), #68540, .F. ) ;
#12133 = CARTESIAN_POINT ( 'NONE',  ( 35.86463821520069217, -286.6558863060381555, -273.7827368651386450 ) ) ;
#12134 = CARTESIAN_POINT ( 'NONE',  ( -96.74805393107904194, -289.1794479906947117, -224.5595020958670602 ) ) ;
#12135 = CARTESIAN_POINT ( 'NONE',  ( 192.3098639061998369, 281.3337059592261085, -109.1536320133224081 ) ) ;
#12136 = CARTESIAN_POINT ( 'NONE',  ( 34.62912086282523916, -286.8902635349357979, -257.4982663267292651 ) ) ;
#12137 = DIRECTION ( 'NONE',  ( 0.000000000000000000, 0.000000000000000000, -1.000000000000000000 ) ) ;
#12138 = CARTESIAN_POINT ( 'NONE',  ( 21.43760079848006939, -283.1602244131310044, -319.7353419897778508 ) ) ;
#12139 = CARTESIAN_POINT ( 'NONE',  ( -113.5813438005440901, -289.4929522382327036, -279.7635207484131570 ) ) ;
#12140 = CARTESIAN_POINT ( 'NONE',  ( -36.77913987123995554, -281.6592347143105144, -194.1502822681547968 ) ) ;
#12141 = CARTESIAN_POINT ( 'NONE',  ( 1.111525613179245697, -281.8690547907502264, -204.1596884215062460 ) ) ;
#12142 = CARTESIAN_POINT ( 'NONE',  ( 0.4017681391234181332, -280.4031858349217146, -207.8171592341532516 ) ) ;
#12143 = CARTESIAN_POINT ( 'NONE',  ( 20.52618475422655919, -276.8941315245025976, -222.6504425319625682 ) ) ;
#12144 = CARTESIAN_POINT ( 'NONE',  ( -74.60636176672315401, -295.5334945952799330, -337.8029128380182442 ) ) ;
#12145 = CARTESIAN_POINT ( 'NONE',  ( -89.05226049374094544, -289.3414026917805018, -216.4578912480474742 ) ) ;
#12146 = CARTESIAN_POINT ( 'NONE',  ( 95.12591598188809883, -298.6689901460368333, -197.0771287801524352 ) ) ;
#12147 = EDGE_LOOP ( 'NONE', ( #10058, #18795, #73951, #70782 ) ) ;
#12148 = ORIENTED_EDGE ( 'NONE', *, *, #17507, .F. ) ;
#12149 = CARTESIAN_POINT ( 'NONE',  ( -85.78064239524103129, -285.6491776325273690, -326.8852992426071751 ) ) ;
#12150 = CARTESIAN_POINT ( 'NONE',  ( -34.98374721744943372, -293.1607495128159826, -193.6933888333213361 ) ) ;
#12151 = CARTESIAN_POINT ( 'NONE',  ( -32.13016675250568710, -283.6360914014192076, -343.2770462023576670 ) ) ;
#12152 = CARTESIAN_POINT ( 'NONE',  ( -49.66960162630130782, -272.9574977029046181, -194.5391266561833561 ) ) ;
#12153 = CARTESIAN_POINT ( 'NONE',  ( -113.7113057255853192, -291.0853606803837579, -279.8000047734951750 ) ) ;
#12154 = CARTESIAN_POINT ( 'NONE',  ( -86.92342681083555078, -283.5107149691977497, -213.0033068358802666 ) ) ;
#12155 = VECTOR ( 'NONE', #33086, 1000.000000000000000 ) ;
#12156 = CARTESIAN_POINT ( 'NONE',  ( 23.08883111274378308, -293.2472353785645396, -222.6546788394745988 ) ) ;
#12157 = CARTESIAN_POINT ( 'NONE',  ( 29.44611453984981964, -288.2840993630251205, -300.0073463656589183 ) ) ;
#12158 = DIRECTION ( 'NONE',  ( 0.000000000000000000, 0.000000000000000000, 1.000000000000000000 ) ) ;
#12159 = CARTESIAN_POINT ( 'NONE',  ( 165.2494399300530290, -11.64849832608277325, 13.00000000000000178 ) ) ;
#12160 = CARTESIAN_POINT ( 'NONE',  ( -105.2969866710188853, -260.2444925846916703, -315.5001506840901015 ) ) ;
#12161 = AXIS2_PLACEMENT_3D ( 'NONE', #47973, #91532, #54614 ) ;
#12162 = CARTESIAN_POINT ( 'NONE',  ( -44.33620535657472317, -284.6590824827696338, -346.3994182778305344 ) ) ;
#12163 = CARTESIAN_POINT ( 'NONE',  ( -20.19161114001082069, -289.7666405000204009, -195.3683826091709363 ) ) ;
#12164 = ORIENTED_EDGE ( 'NONE', *, *, #57750, .F. ) ;
#12165 = CARTESIAN_POINT ( 'NONE',  ( 29.59109355022479804, -280.8749501981781691, -300.3893375235729764 ) ) ;
#12166 = CARTESIAN_POINT ( 'NONE',  ( -14.59999215182917531, -276.4321008013143341, -343.9598331176591159 ) ) ;
#12167 = CARTESIAN_POINT ( 'NONE',  ( -92.66902528389553595, -281.2570878000263974, -219.9734655407550008 ) ) ;
#12168 = CARTESIAN_POINT ( 'NONE',  ( 86.42939490984008444, 81.28859003109494097, -300.3317345712586075 ) ) ;
#12169 = CARTESIAN_POINT ( 'NONE',  ( 23.29091717055268873, -279.5016194973937331, -223.8392852947689846 ) ) ;
#12170 = CARTESIAN_POINT ( 'NONE',  ( -100.9991269917803720, -283.0987470634276519, -231.2809142228382200 ) ) ;
#12171 = CARTESIAN_POINT ( 'NONE',  ( -20.80751537109819083, -300.0165860262275714, -194.3695687811124913 ) ) ;
#12172 = CARTESIAN_POINT ( 'NONE',  ( 32.68626100221049313, -293.7669239865959412, -249.3524132035507819 ) ) ;
#12173 = VERTEX_POINT ( 'NONE', #65456 ) ;
#12174 = CARTESIAN_POINT ( 'NONE',  ( -65.50052449426593171, -290.3609424753026929, -202.4628760507472123 ) ) ;
#12175 = CARTESIAN_POINT ( 'NONE',  ( -7.915958199600482637, -277.3280347832439929, -341.4207115390197487 ) ) ;
#12176 = CARTESIAN_POINT ( 'NONE',  ( -8.970830099267709912, -274.4337146183043501, -203.0458227968066751 ) ) ;
#12177 = CARTESIAN_POINT ( 'NONE',  ( -112.1387490793718769, -271.6851727742526919, -253.4231730181333830 ) ) ;
#12178 = CARTESIAN_POINT ( 'NONE',  ( -112.3417001281054723, -270.5523139186827279, -270.3356821209761165 ) ) ;
#12179 = B_SPLINE_CURVE_WITH_KNOTS ( 'NONE', 3,
 ( #19649, #71267, #78367, #57529, #13506, #49929, #48518, #64194, #86374, #77418, #5930, #21525, #43307, #93026, #85910, #12557, #21062, #78826, #13971, #84972, #93487, #71745, #41407, #6873, #50403, #92076, #35745, #20121, #64659, #79309, #26765, #27230 ),
 .UNSPECIFIED., .F., .F.,
 ( 4, 2, 2, 2, 2, 2, 2, 2, 2, 2, 2, 2, 2, 2, 2, 4 ),
 ( 5.029510472558947976E-05, 0.0005389448914400213776, 0.001027594678154453330, 0.001516244464868885498, 0.002004894251583317234, 0.002982193825012181138, 0.003470843611726534810, 0.003959493398440889350, 0.004448143185155244324, 0.004936792971869597563, 0.005425442758583952536, 0.005914092545298305775, 0.006402742332012659882, 0.006891392118727013121, 0.007380041905441368094, 0.007868691692155720466 ),
 .UNSPECIFIED. ) ;
#12180 = CARTESIAN_POINT ( 'NONE',  ( -43.49890293645135841, -252.7466870590830865, -490.1793782242883708 ) ) ;
#12181 = CARTESIAN_POINT ( 'NONE',  ( 34.36468109498141388, -282.4308064254109354, -255.0560012621517103 ) ) ;
#12182 = CARTESIAN_POINT ( 'NONE',  ( 36.34306245447238126, -283.0769474221561381, -251.7996045828177500 ) ) ;
#12183 = CARTESIAN_POINT ( 'NONE',  ( -95.84253576604854175, -284.5152067011182453, -226.5256882694470448 ) ) ;
#12184 = CARTESIAN_POINT ( 'NONE',  ( 10.01386047972154358, -273.1169381897151425, -213.6912549244103161 ) ) ;
#12185 = CARTESIAN_POINT ( 'NONE',  ( -3.810487204755621971, -282.3597111919590361, -204.1161606322495743 ) ) ;
#12186 = CARTESIAN_POINT ( 'NONE',  ( 30.82345145232138250, -273.6586523184039379, -242.2231109509739611 ) ) ;
#12187 = CARTESIAN_POINT ( 'NONE',  ( 160.5350683151633291, 250.0000000000000568, 20.22542485937379908 ) ) ;
#12188 = CARTESIAN_POINT ( 'NONE',  ( -29.97240801541454402, -275.2272902793549179, -197.4233389703065882 ) ) ;
#12189 = CARTESIAN_POINT ( 'NONE',  ( 199.0061125298537377, 275.5000000000000568, -7.725424859374024678 ) ) ;
#12190 = CARTESIAN_POINT ( 'NONE',  ( -109.4581908558036076, -279.6926047155141646, -243.6863145223899778 ) ) ;
#12191 = ORIENTED_EDGE ( 'NONE', *, *, #80971, .F. ) ;
#12192 = ORIENTED_EDGE ( 'NONE', *, *, #34350, .F. ) ;
#12193 = LINE ( 'NONE', #62886, #47404 ) ;
#12194 = CARTESIAN_POINT ( 'NONE',  ( -107.8871901145954268, -286.7701849255651041, -242.5842992570482011 ) ) ;
#12195 = EDGE_CURVE ( 'NONE', #52563, #1567, #45873, .T. ) ;
#12196 = CARTESIAN_POINT ( 'NONE',  ( -20.82163094983162210, -294.0319387170497407, -341.6852733604249011 ) ) ;
#12197 = CARTESIAN_POINT ( 'NONE',  ( -114.2882219228515623, -289.8899927519804010, -271.2193291012045506 ) ) ;
#12198 = CARTESIAN_POINT ( 'NONE',  ( 7.559225863779852617, -284.9137802728170072, -211.4585983066750146 ) ) ;
#12200 = CARTESIAN_POINT ( 'NONE',  ( -74.06698991887705574, -287.7870453570566838, -334.6347940558463847 ) ) ;
#12199 = CARTESIAN_POINT ( 'NONE',  ( -46.78262172876914349, -284.5048047828813083, -197.3288132142241977 ) ) ;
#12201 = CARTESIAN_POINT ( 'NONE',  ( -109.5865826433986996, -285.9281213835758422, -257.3362805320824123 ) ) ;
#12202 = CARTESIAN_POINT ( 'NONE',  ( 32.31697798636230345, -273.9156722045734114, -298.2979450863081752 ) ) ;
#12203 = CARTESIAN_POINT ( 'NONE',  ( 37.99772346691247549, -285.8066078133404062, -258.8542976975157330 ) ) ;
#12204 = CARTESIAN_POINT ( 'NONE',  ( -45.92689010823990969, -299.9434374331393087, -195.8541038121131521 ) ) ;
#12205 = CARTESIAN_POINT ( 'NONE',  ( 1.808399266338743372, -284.5744438434254562, -206.1949419754272128 ) ) ;
#12206 = CARTESIAN_POINT ( 'NONE',  ( -6.681819521282037044, -281.4060838330309480, -203.8389321843791606 ) ) ;
#12207 = CARTESIAN_POINT ( 'NONE',  ( -94.96872272678864135, -291.8867198598726986, -318.6423902799984376 ) ) ;
#12208 = CARTESIAN_POINT ( 'NONE',  ( 193.2782779784440379, 275.9651295423822717, 16.89756555088499113 ) ) ;
#12209 = CARTESIAN_POINT ( 'NONE',  ( 153.9133111279456045, 20.47222690886501439, -13.06183683676588991 ) ) ;
#12210 = CARTESIAN_POINT ( 'NONE',  ( -107.0371653761872039, -298.0924419484564396, -299.6830084152645099 ) ) ;
#12211 = CARTESIAN_POINT ( 'NONE',  ( -106.2704250900716403, -276.9385234075442099, -240.8004765643772487 ) ) ;
#12212 = CARTESIAN_POINT ( 'NONE',  ( 1.627045640737986965, -291.7560645211557926, -204.0764779830154225 ) ) ;
#12213 = CARTESIAN_POINT ( 'NONE',  ( -111.0416378147748588, -294.9018857734444055, -274.2029402473264668 ) ) ;
#12214 = CARTESIAN_POINT ( 'NONE',  ( 15.62635212349230684, -279.5056411373265632, -219.3410838375655203 ) ) ;
#12215 = CARTESIAN_POINT ( 'NONE',  ( -46.32885511714368221, -272.0170786454707468, -196.4656158069768424 ) ) ;
#12216 = CARTESIAN_POINT ( 'NONE',  ( 33.92837093508556023, -295.1024964109620328, -288.3004727649005190 ) ) ;
#12217 = CARTESIAN_POINT ( 'NONE',  ( -110.4683760289727132, -299.2662352645559167, -253.7030783399848985 ) ) ;
#12218 = CARTESIAN_POINT ( 'NONE',  ( -65.27004920581832437, -296.1737045843922829, -199.2925713611411140 ) ) ;
#12219 = CARTESIAN_POINT ( 'NONE',  ( 34.52066476800799677, -292.1092301560768192, -295.2158334448697588 ) ) ;
#12220 = CARTESIAN_POINT ( 'NONE',  ( -110.9260335088017513, -291.9663220036208031, -271.2101152383597764 ) ) ;
#12221 = CARTESIAN_POINT ( 'NONE',  ( 175.2296996224750103, 249.5000000000000568, 0.000000000000000000 ) ) ;
#12222 = CARTESIAN_POINT ( 'NONE',  ( -107.9103373006685302, -291.6094750962571993, -251.0564767033813780 ) ) ;
#12223 = DIRECTION ( 'NONE',  ( 0.000000000000000000, 1.000000000000000000, 0.000000000000000000 ) ) ;
#12224 = CARTESIAN_POINT ( 'NONE',  ( -111.6133822124661634, -291.9936991492689344, -251.5538813231878521 ) ) ;
#12226 = CARTESIAN_POINT ( 'NONE',  ( 6.676241738921436131, -292.6700126829893520, -212.1252115863068184 ) ) ;
#12225 = CARTESIAN_POINT ( 'NONE',  ( 7.586536656508338083, -278.6814628473795210, -209.7994598067362233 ) ) ;
#12227 = CARTESIAN_POINT ( 'NONE',  ( -31.07375881513053884, -280.1291405431306885, -193.5639622451460014 ) ) ;
#12228 = CIRCLE ( 'NONE', #65192, 1.499999999999992673 ) ;
#12229 = CARTESIAN_POINT ( 'NONE',  ( -113.8832898643969145, -284.1163759313272976, -278.5543671618648887 ) ) ;
#12230 = CARTESIAN_POINT ( 'NONE',  ( 25.77120952216590766, -286.0943649801365041, -310.5704335842223145 ) ) ;
#12231 = CARTESIAN_POINT ( 'NONE',  ( -33.45484955168409158, -281.1423197847879578, -344.5072823240979005 ) ) ;
#12232 = CARTESIAN_POINT ( 'NONE',  ( -74.65187693594110385, -278.0447971328082417, -203.7979265044083093 ) ) ;
#12233 = CARTESIAN_POINT ( 'NONE',  ( -52.10027496992502449, -284.7879543168428427, -195.0495433521734867 ) ) ;
#12234 = CARTESIAN_POINT ( 'NONE',  ( 195.4675039778850874, 40.79415162994154542, 14.67933883143855844 ) ) ;
#12235 = CARTESIAN_POINT ( 'NONE',  ( 36.08918958322248471, -295.0496659380318647, -262.4966309275322374 ) ) ;
#12236 = CARTESIAN_POINT ( 'NONE',  ( -64.86575049154239991, -278.8298329513968383, -341.6983316994605389 ) ) ;
#12237 = CARTESIAN_POINT ( 'NONE',  ( -110.3721857433128832, -278.2512818505545624, -267.9033186655663030 ) ) ;
#12238 = CARTESIAN_POINT ( 'NONE',  ( -112.2621967214914207, -290.4958358142283146, -288.1916435425410441 ) ) ;
#12239 = CARTESIAN_POINT ( 'NONE',  ( -47.09516221221688426, -281.2549789651542369, -345.2889777796481781 ) ) ;
#12240 = CARTESIAN_POINT ( 'NONE',  ( 33.34065423091620772, -292.8638572597541270, -289.5767956944072807 ) ) ;
#12241 = CARTESIAN_POINT ( 'NONE',  ( -97.47326855502184628, -295.1643581684585911, -225.5156464618005430 ) ) ;
#12242 = ORIENTED_EDGE ( 'NONE', *, *, #46507, .F. ) ;
#12243 = CARTESIAN_POINT ( 'NONE',  ( -23.68628624284178130, -55.96374926131388605, -21.50000000000000000 ) ) ;
#12244 = CARTESIAN_POINT ( 'NONE',  ( 33.83394867336524214, -293.2778457244722290, -286.9091041001183271 ) ) ;
#12245 = CARTESIAN_POINT ( 'NONE',  ( 129.8483263487583201, -299.5541904835127980, -195.3611179825600175 ) ) ;
#12246 = CARTESIAN_POINT ( 'NONE',  ( 17.40634833298269157, -290.4094976428775112, -226.7417163044926838 ) ) ;
#12247 = CARTESIAN_POINT ( 'NONE',  ( -112.0426122002401144, -295.8327135549497484, -252.6807913541129835 ) ) ;
#12248 = CARTESIAN_POINT ( 'NONE',  ( 35.42021604417455904, -279.4220560292304185, -249.1956301611389506 ) ) ;
#12249 = CARTESIAN_POINT ( 'NONE',  ( -75.87293286456544195, -286.8644720892505120, -204.2043977389613758 ) ) ;
#12250 = CARTESIAN_POINT ( 'NONE',  ( 23.53523806185751610, -286.8254345529110196, -229.9831410774160645 ) ) ;
#12251 = CARTESIAN_POINT ( 'NONE',  ( -95.81142191041391243, -279.4471145343522380, -315.2164341560484786 ) ) ;
#12252 = CARTESIAN_POINT ( 'NONE',  ( -111.8526729088855234, -294.6298944311196237, -265.8932621870417279 ) ) ;
#12253 = CARTESIAN_POINT ( 'NONE',  ( -61.32056243981657673, -297.1278680915882546, -340.4367708109081718 ) ) ;
#12254 = EDGE_CURVE ( 'NONE', #79037, #42785, #56532, .T. ) ;
#12255 = CARTESIAN_POINT ( 'NONE',  ( -93.03791353753595672, -276.6702134207022254, -318.1634434236502216 ) ) ;
#12256 = EDGE_LOOP ( 'NONE', ( #34034, #70174, #3561, #19174 ) ) ;
#12257 = DIRECTION ( 'NONE',  ( -0.000000000000000000, -1.000000000000000000, -0.000000000000000000 ) ) ;
#12258 = CARTESIAN_POINT ( 'NONE',  ( -110.7916707995137244, -296.5104465501717641, -247.1443520679468691 ) ) ;
#12259 = CARTESIAN_POINT ( 'NONE',  ( -83.41882080653705600, -291.6096319183529317, -328.8266047662896767 ) ) ;
#12260 = CARTESIAN_POINT ( 'NONE',  ( 23.40369620696903397, -295.7715792783166648, -316.3658703643342847 ) ) ;
#12261 = CARTESIAN_POINT ( 'NONE',  ( 201.0264371890905295, 293.4388253988550446, -53.99999999998393463 ) ) ;
#12262 = EDGE_CURVE ( 'NONE', #9702, #46866, #996, .T. ) ;
#12263 = CARTESIAN_POINT ( 'NONE',  ( 32.41338023834404680, -288.4949644403909588, -292.3956429355217779 ) ) ;
#12264 = CARTESIAN_POINT ( 'NONE',  ( -43.52658375460264750, -249.7100083083012692, -454.9363245936367548 ) ) ;
#12265 = ORIENTED_EDGE ( 'NONE', *, *, #53102, .F. ) ;
#12266 = CARTESIAN_POINT ( 'NONE',  ( 35.95462134410069410, -280.3234292536554904, -247.5473179570181230 ) ) ;
#12267 = CARTESIAN_POINT ( 'NONE',  ( -112.5026404498714641, -297.4078133366812722, -254.0470624620327271 ) ) ;
#12268 = CARTESIAN_POINT ( 'NONE',  ( -66.51754283989180294, -289.8136788822043854, -200.4391923523176615 ) ) ;
#12269 = CARTESIAN_POINT ( 'NONE',  ( -98.21986154133084312, -297.5147828649090229, -223.2272780580528320 ) ) ;
#12270 = CARTESIAN_POINT ( 'NONE',  ( 196.8803347170859865, 250.0000000000000568, 12.49999999999999289 ) ) ;
#12271 = CARTESIAN_POINT ( 'NONE',  ( 175.2296996224750103, 247.0000000000001137, 8.550761578869359170 ) ) ;
#12272 = DIRECTION ( 'NONE',  ( 0.000000000000000000, 0.000000000000000000, 1.000000000000000000 ) ) ;
#12273 = CARTESIAN_POINT ( 'NONE',  ( 9.814813650075565832, -289.9367044543358247, -330.4197763981928233 ) ) ;
#12274 = CARTESIAN_POINT ( 'NONE',  ( -99.86837403722181250, -294.6952119285919025, -220.4570493818173702 ) ) ;
#12275 = CARTESIAN_POINT ( 'NONE',  ( 34.48932993219253973, -281.2487535259369906, -297.8131836031942044 ) ) ;
#12276 = CARTESIAN_POINT ( 'NONE',  ( -82.60727683114484421, -287.4321626107948191, -210.7703805379511550 ) ) ;
#12277 = CARTESIAN_POINT ( 'NONE',  ( -46.41737087459109290, -284.5138541181401024, -194.4912392918764397 ) ) ;
#12278 = CARTESIAN_POINT ( 'NONE',  ( 3.962559356409089961, -272.6092366696081513, -207.8973601537884122 ) ) ;
#12279 = CARTESIAN_POINT ( 'NONE',  ( -106.7679418898665773, -274.8258885968784853, -243.3615688579964456 ) ) ;
#12280 = CARTESIAN_POINT ( 'NONE',  ( -93.62964140134269542, -289.3127449480446103, -221.6478562641615042 ) ) ;
#12281 = CARTESIAN_POINT ( 'NONE',  ( -61.98152825431640167, -279.2293862984769248, -342.0627609226370964 ) ) ;
#12282 = PRODUCT_DEFINITION ( 'UNKNOWN', '', #55311, #56106 ) ;
#12284 = CARTESIAN_POINT ( 'NONE',  ( 32.83476664340047080, -280.6302785096988828, -249.8878139061026786 ) ) ;
#12283 = CARTESIAN_POINT ( 'NONE',  ( -66.06970082331426397, -279.6654330015371102, -203.2378524186758568 ) ) ;
#12285 = CARTESIAN_POINT ( 'NONE',  ( 36.59131022884746898, -276.8887249210343953, -290.7915417684785098 ) ) ;
#12286 = CARTESIAN_POINT ( 'NONE',  ( 20.77492727107647852, -279.6698321323710843, -220.4365949994931100 ) ) ;
#12287 = CARTESIAN_POINT ( 'NONE',  ( 195.1743528851788199, 283.2594845134466368, -110.5268553716196749 ) ) ;
#12288 = CARTESIAN_POINT ( 'NONE',  ( -83.44836953659944356, -274.3789098938663074, -208.9187287201598622 ) ) ;
#12289 = CARTESIAN_POINT ( 'NONE',  ( -43.26235011396510544, -299.4041787160501826, -194.1272658402198203 ) ) ;
#12290 = CARTESIAN_POINT ( 'NONE',  ( 31.95455697924148097, -289.6233781216988064, -236.9535640164627637 ) ) ;
#12291 = VERTEX_POINT ( 'NONE', #86254 ) ;
#12292 = AXIS2_PLACEMENT_3D ( 'NONE', #39594, #90715, #47174 ) ;
#12293 = CARTESIAN_POINT ( 'NONE',  ( -0.8255832566043728171, -289.6350506796578088, -333.9868366128078492 ) ) ;
#12294 = CARTESIAN_POINT ( 'NONE',  ( 35.71071140791632104, -289.0445011284853081, -249.2623049460595723 ) ) ;
#12295 = CARTESIAN_POINT ( 'NONE',  ( -56.09973924764294395, -288.6486645537076470, -341.0680395405777858 ) ) ;
#12296 = CARTESIAN_POINT ( 'NONE',  ( -111.0508255130668118, -283.7822792773383753, -292.4634374057991408 ) ) ;
#12297 = CARTESIAN_POINT ( 'NONE',  ( -11.74252710806512567, -92.25804922821241405, -360.0298267093687059 ) ) ;
#12298 = CARTESIAN_POINT ( 'NONE',  ( 24.36249257634518628, -279.3957484082234259, -229.7839498355443482 ) ) ;
#12299 = CARTESIAN_POINT ( 'NONE',  ( -60.38415036879518283, -287.6105736046046673, -199.7926337589588286 ) ) ;
#12300 = CARTESIAN_POINT ( 'NONE',  ( 26.14661009765528377, -280.5423287361759890, -307.8777115820259382 ) ) ;
#12301 = CARTESIAN_POINT ( 'NONE',  ( -96.81456792384837229, -280.4675065571523191, -227.1844868604487715 ) ) ;
#12302 = CARTESIAN_POINT ( 'NONE',  ( -40.50215777285083618, -277.5852773837323753, -343.3667429060195673 ) ) ;
#12303 = CARTESIAN_POINT ( 'NONE',  ( -106.8934364363057625, -289.7613145279184437, -238.1323836803984477 ) ) ;
#12304 = CARTESIAN_POINT ( 'NONE',  ( -108.0744848543433960, -284.9705600630828712, -300.5143860453322873 ) ) ;
#12305 = CARTESIAN_POINT ( 'NONE',  ( -99.73488931745403363, -284.4460960140673933, -315.4681035871540189 ) ) ;
#12306 = CARTESIAN_POINT ( 'NONE',  ( -18.73358778480818643, -282.9725910021337540, -341.0020354171684858 ) ) ;
#12307 = ORIENTED_EDGE ( 'NONE', *, *, #907, .F. ) ;
#12308 = CARTESIAN_POINT ( 'NONE',  ( 206.8799559751410584, 30.07585723490866059, 15.00000000000000178 ) ) ;
#12309 = CARTESIAN_POINT ( 'NONE',  ( -112.7793822618751278, -292.5088696306393672, -262.7844240488696528 ) ) ;
#12310 = CARTESIAN_POINT ( 'NONE',  ( 12.96686980223632979, -291.4225696925302032, -212.7213221546050761 ) ) ;
#12311 = CARTESIAN_POINT ( 'NONE',  ( 11.71299313959655386, -273.8116788298353868, -215.9141006872862931 ) ) ;
#12312 = CARTESIAN_POINT ( 'NONE',  ( -99.93037944374245285, -295.3071608886352806, -315.1270986449532643 ) ) ;
#12313 = CARTESIAN_POINT ( 'NONE',  ( -100.2939329859144948, -289.5547202451573980, -232.0502301077711138 ) ) ;
#12314 = CARTESIAN_POINT ( 'NONE',  ( -41.11296538479525964, -293.3400869444051295, -344.2910536434748110 ) ) ;
#12315 = CARTESIAN_POINT ( 'NONE',  ( -109.1020049645889003, -291.9594656185281565, -254.9471906481589087 ) ) ;
#12316 = DIRECTION ( 'NONE',  ( 0.000000000000000000, 0.000000000000000000, -1.000000000000000000 ) ) ;
#12317 = CARTESIAN_POINT ( 'NONE',  ( -51.28777609540209426, -291.2306304234671188, -344.0530959106517344 ) ) ;
#12318 = CARTESIAN_POINT ( 'NONE',  ( 35.98959470203071476, -291.7642438109647287, -286.9282053159424208 ) ) ;
#12319 = CARTESIAN_POINT ( 'NONE',  ( -73.85753729900216058, -297.5371780412540943, -335.8858413564130956 ) ) ;
#12320 = CARTESIAN_POINT ( 'NONE',  ( -30.52126939088868696, -287.0816260456099940, -197.3931473229183950 ) ) ;
#12321 = CARTESIAN_POINT ( 'NONE',  ( 27.99403419739965670, -296.0479111324673909, -307.6317697364838750 ) ) ;
#12322 = CARTESIAN_POINT ( 'NONE',  ( 12.84974033404173710, -276.7279805236878474, -214.0844165269328983 ) ) ;
#12323 = CARTESIAN_POINT ( 'NONE',  ( -54.54904394307327919, -297.0336317297703204, -195.4740954831521833 ) ) ;
#12324 = CARTESIAN_POINT ( 'NONE',  ( -24.17099700790322103, -275.1216660739979716, -343.2453244915890309 ) ) ;
#12325 = CARTESIAN_POINT ( 'NONE',  ( -57.47973599684804213, -277.8700182071046356, -198.6968053393258913 ) ) ;
#12326 = CARTESIAN_POINT ( 'NONE',  ( -98.18088628750028590, -274.3258788034443683, -229.2128516132085565 ) ) ;
#12327 = CARTESIAN_POINT ( 'NONE',  ( 24.85790375305440136, -273.5342227035681617, -225.9561232890435747 ) ) ;
#12328 = CARTESIAN_POINT ( 'NONE',  ( -108.8674592320696632, -297.7502853114162349, -287.7185590533965751 ) ) ;
#12329 = DIRECTION ( 'NONE',  ( 0.000000000000000000, 0.000000000000000000, 1.000000000000000000 ) ) ;
#12330 = CARTESIAN_POINT ( 'NONE',  ( -109.5205565110302359, -297.1976890153803197, -282.3116166514656129 ) ) ;
#12331 = DIRECTION ( 'NONE',  ( 1.000000000000000000, -0.000000000000000000, -0.000000000000000000 ) ) ;
#12333 = CARTESIAN_POINT ( 'NONE',  ( -85.30856530277549155, -273.2010595982754353, -215.2648465032376635 ) ) ;
#12332 = CARTESIAN_POINT ( 'NONE',  ( 30.20170578519502769, -286.0123585095279850, -303.8897227860072690 ) ) ;
#12334 = CARTESIAN_POINT ( 'NONE',  ( -37.98244548293538259, -286.0443322566591746, -193.3637839677369072 ) ) ;
#12335 = CARTESIAN_POINT ( 'NONE',  ( -105.1393533608000439, -289.7473706317709912, -306.8196218956072698 ) ) ;
#12336 = CARTESIAN_POINT ( 'NONE',  ( -107.3696304866851676, -298.8943726077774841, -242.3910098301828384 ) ) ;
#12337 = CARTESIAN_POINT ( 'NONE',  ( -31.48362787898167880, -292.9779849416254933, -345.0161856952290691 ) ) ;
#12338 = CARTESIAN_POINT ( 'NONE',  ( 25.79180670193011693, -281.3294068004708492, -314.1828745627234412 ) ) ;
#12339 = CARTESIAN_POINT ( 'NONE',  ( -4.771743288812454686, -289.9809262143061801, -202.8022627189028810 ) ) ;
#12340 = CARTESIAN_POINT ( 'NONE',  ( 13.01691457970142984, -278.7548853946701115, -214.7132872792192302 ) ) ;
#12341 = CARTESIAN_POINT ( 'NONE',  ( 202.9270896288134907, 287.6726455163375249, -4.941865385500935126 ) ) ;
#12342 = CARTESIAN_POINT ( 'NONE',  ( -5.634717298421447751, -287.4204732917380625, -336.5562669444793755 ) ) ;
#12343 = DIRECTION ( 'NONE',  ( 0.9951408606192336803, 1.205805641958489930E-17, 0.09846150276128748380 ) ) ;
#12344 = CARTESIAN_POINT ( 'NONE',  ( -102.0418455001494067, -288.0438598972423279, -308.3961917731384119 ) ) ;
#12345 = CARTESIAN_POINT ( 'NONE',  ( -93.36486008588094876, -298.8288843281441132, -222.3016279232871568 ) ) ;
#12346 = CARTESIAN_POINT ( 'NONE',  ( -8.246308434866241655, -284.1039444616968126, -341.0717746061306457 ) ) ;
#12348 = CARTESIAN_POINT ( 'NONE',  ( 28.97268187461106947, -281.1389756182431370, -239.7210847254205532 ) ) ;
#12347 = CARTESIAN_POINT ( 'NONE',  ( -84.17406545711961030, -295.4318630093549132, -211.3260745132724026 ) ) ;
#12349 = CARTESIAN_POINT ( 'NONE',  ( -89.60986098759802587, -297.5063607904565970, -213.7465203535422802 ) ) ;
#12350 = CARTESIAN_POINT ( 'NONE',  ( -74.58715180564381342, -274.9718270474398878, -206.8343631794590181 ) ) ;
#12351 = CARTESIAN_POINT ( 'NONE',  ( -8.334658402542197919, -282.4320570626722429, -201.1836710167748379 ) ) ;
#12352 = B_SPLINE_CURVE_WITH_KNOTS ( 'NONE', 3,
 ( #59600, #7981, #23117, #80413, #45817, #15097, #8447, #43957, #45342, #52465, #72855, #66687, #88901, #52000, #87053, #36875, #16034, #51525, #65790, #29782, #44430, #58661, #81339, #67162 ),
 .UNSPECIFIED., .F., .F.,
 ( 4, 2, 2, 2, 2, 2, 2, 2, 2, 2, 2, 4 ),
 ( 0.000000000000000000, 0.06250000000000000000, 0.1250000000000000000, 0.2500000000000000000, 0.3750000000000000000, 0.5000000000000000000, 0.6250000000000000000, 0.7500000000000000000, 0.8125000000000000000, 0.8750000000000000000, 0.9375000000000000000, 1.000000000000000000 ),
 .UNSPECIFIED. ) ;
#12353 = CARTESIAN_POINT ( 'NONE',  ( -109.8866175390029412, -271.6157113375448944, -259.4571357085231966 ) ) ;
#12354 = AXIS2_PLACEMENT_3D ( 'NONE', #82747, #48156, #48626 ) ;
#12355 = VERTEX_POINT ( 'NONE', #38848 ) ;
#12356 = DIRECTION ( 'NONE',  ( 1.000000000000000000, 0.000000000000000000, 0.000000000000000000 ) ) ;
#12357 = CARTESIAN_POINT ( 'NONE',  ( -110.5468839981672460, -286.7202603077519143, -255.7718116152337018 ) ) ;
#12358 = CARTESIAN_POINT ( 'NONE',  ( 142.6449502718966755, -0.9999999999999991118, 22.50000000000000000 ) ) ;
#12359 = CARTESIAN_POINT ( 'NONE',  ( 40.65961533371913106, -278.8380690714489560, -252.5904736702033802 ) ) ;
#12360 = CARTESIAN_POINT ( 'NONE',  ( -100.3389879459672898, -277.1665491118436080, -314.3554420278452994 ) ) ;
#12361 = CARTESIAN_POINT ( 'NONE',  ( -97.54026788375671231, -288.3216059542572793, -317.0791322641306351 ) ) ;
#12362 = AXIS2_PLACEMENT_3D ( 'NONE', #79885, #29710, #58592 ) ;
#12363 = CARTESIAN_POINT ( 'NONE',  ( -42.96670276048308779, -284.6444194685781213, -343.8900249105404896 ) ) ;
#12364 = CARTESIAN_POINT ( 'NONE',  ( 30.90695707659207514, -276.7784004215046139, -242.1456897177627070 ) ) ;
#12365 = CARTESIAN_POINT ( 'NONE',  ( -113.7649760321169339, -285.9460777749832801, -272.8483026054009315 ) ) ;
#12366 = CARTESIAN_POINT ( 'NONE',  ( -80.87391478423749902, -282.4525475443406890, -329.5181572540485035 ) ) ;
#12367 = CARTESIAN_POINT ( 'NONE',  ( -32.86849959756012396, -282.1086894136328738, -195.4946293040974012 ) ) ;
#12368 = CARTESIAN_POINT ( 'NONE',  ( -34.10531919109820365, -274.2584813910368098, -193.4291620542774695 ) ) ;
#12369 = CARTESIAN_POINT ( 'NONE',  ( -111.8279815417099314, -278.1406233807484796, -289.9268728162484194 ) ) ;
#12370 = CARTESIAN_POINT ( 'NONE',  ( -73.99047156523944579, -297.4632290545595197, -335.1544953516561804 ) ) ;
#12371 = DIRECTION ( 'NONE',  ( 0.7484200282493165268, 0.000000000000000000, -0.6632250457539224930 ) ) ;
#12372 = EDGE_CURVE ( 'NONE', #25769, #34721, #20961, .T. ) ;
#12373 = LINE ( 'NONE', #70158, #1221 ) ;
#12374 = CARTESIAN_POINT ( 'NONE',  ( -111.6721816342009248, -294.8790802923677461, -255.6219096070480532 ) ) ;
#12375 = CARTESIAN_POINT ( 'NONE',  ( -3.844833691172875767, -276.1053555423025614, -335.2914528095027435 ) ) ;
#12376 = CARTESIAN_POINT ( 'NONE',  ( -65.44160412548666272, -298.7730784402122026, -198.9468872621766025 ) ) ;
#12377 = CARTESIAN_POINT ( 'NONE',  ( -44.13945563225464497, -287.7251643746256491, -196.6606123302011895 ) ) ;
#12378 = CARTESIAN_POINT ( 'NONE',  ( -6.064032080916389233, -296.1686117307091308, -339.9629515513158253 ) ) ;
#12379 = CARTESIAN_POINT ( 'NONE',  ( -11.17832639995599209, -295.9238376586882282, -342.4138347899152564 ) ) ;
#12380 = CARTESIAN_POINT ( 'NONE',  ( -112.0781864990786971, -292.6130086766314093, -265.6448368251349734 ) ) ;
#12381 =( REPRESENTATION_RELATIONSHIP ('NONE','NONE', #78428, #30030 ) REPRESENTATION_RELATIONSHIP_WITH_TRANSFORMATION ( #11353 )SHAPE_REPRESENTATION_RELATIONSHIP( ) );
#12382 = CARTESIAN_POINT ( 'NONE',  ( 14.62613770033450855, -278.7850881638697160, -216.4430617230063376 ) ) ;
#12383 = CARTESIAN_POINT ( 'NONE',  ( -62.82443310092831723, -281.6381287760690952, -200.3642630252234085 ) ) ;
#12384 = CARTESIAN_POINT ( 'NONE',  ( -41.13661430115381279, -293.1800999510632550, -344.7171427419654606 ) ) ;
#12385 = CARTESIAN_POINT ( 'NONE',  ( -85.30188125907153562, -285.5672148244704545, -329.0137096019414571 ) ) ;
#12386 = CARTESIAN_POINT ( 'NONE',  ( -91.74140396466356151, -284.1740150678466534, -221.1449300419688484 ) ) ;
#12387 = CARTESIAN_POINT ( 'NONE',  ( 204.9738562182569979, 293.6303156117443223, -54.00000000000747491 ) ) ;
#12388 = EDGE_LOOP ( 'NONE', ( #84486, #669, #4733, #84122 ) ) ;
#12389 = CARTESIAN_POINT ( 'NONE',  ( -110.2490565082685663, -284.2835098783307330, -265.4595574974268857 ) ) ;
#12390 = ORIENTED_EDGE ( 'NONE', *, *, #79580, .F. ) ;
#12391 = CARTESIAN_POINT ( 'NONE',  ( 35.03138931000073342, -282.3087423848197659, -244.8327572750843615 ) ) ;
#12392 = CARTESIAN_POINT ( 'NONE',  ( -78.87058298120439304, -273.8087513320262474, -210.2377325723746537 ) ) ;
#12393 = CARTESIAN_POINT ( 'NONE',  ( 36.31371157666659144, -286.0797629835053044, -249.1277041300705548 ) ) ;
#12394 = CARTESIAN_POINT ( 'NONE',  ( 39.04524470153614857, -282.5952721576835529, -278.4816875874217885 ) ) ;
#12395 = CARTESIAN_POINT ( 'NONE',  ( -111.1518169033748933, -279.8271526880959641, -289.7715003554112627 ) ) ;
#12396 = CARTESIAN_POINT ( 'NONE',  ( -67.33036735255592475, -280.3204651058207446, -199.5515661913208021 ) ) ;
#12397 = CARTESIAN_POINT ( 'NONE',  ( -21.39648532958014826, -274.3380690714489560, -340.3683826091709079 ) ) ;
#12398 = CARTESIAN_POINT ( 'NONE',  ( 203.3400678907170231, 292.9455748915181061, -83.20730514549673273 ) ) ;
#12399 = ORIENTED_EDGE ( 'NONE', *, *, #51127, .T. ) ;
#12400 = CARTESIAN_POINT ( 'NONE',  ( -92.49043599584310016, -275.2606048649046784, -219.7590873547483170 ) ) ;
#12401 = CARTESIAN_POINT ( 'NONE',  ( -112.9615723932939062, -270.7119090785686240, -296.2735061844161351 ) ) ;
#12402 = CARTESIAN_POINT ( 'NONE',  ( -43.87037679853860084, -277.9894685846156790, -195.9510056702047507 ) ) ;
#12403 = CARTESIAN_POINT ( 'NONE',  ( 38.21597287674843813, -295.2040146367762645, -261.8172931764508462 ) ) ;
#12404 = CARTESIAN_POINT ( 'NONE',  ( -47.81583098944544474, -294.5373146293514424, -342.7601395228516026 ) ) ;
#12405 = CARTESIAN_POINT ( 'NONE',  ( -109.4139899671798446, -290.4023521162516204, -243.2814220093720792 ) ) ;
#12406 = CARTESIAN_POINT ( 'NONE',  ( 208.6208076322478746, 32.98517505407394168, 12.09245862095555601 ) ) ;
#12408 = CARTESIAN_POINT ( 'NONE',  ( 28.37974902053175441, -285.4995115546490752, -236.6756032379166470 ) ) ;
#12407 = CARTESIAN_POINT ( 'NONE',  ( -74.33711193959376828, -294.1084524502449540, -337.2780333952446199 ) ) ;
#12409 = CARTESIAN_POINT ( 'NONE',  ( 35.42259604894641001, -295.2218198698093943, -255.6566055860660640 ) ) ;
#12410 = CARTESIAN_POINT ( 'NONE',  ( 29.86931596887154683, -286.6359094285825222, -300.2181546650601831 ) ) ;
#12411 = CARTESIAN_POINT ( 'NONE',  ( -108.5670512060605404, -285.6298209544997917, -288.4772114669492566 ) ) ;
#12412 = EDGE_LOOP ( 'NONE', ( #49233, #85830, #50103, #92985, #51621, #43910 ) ) ;
#12413 = CARTESIAN_POINT ( 'NONE',  ( -112.4124034799732925, -291.6953305836013328, -254.2612952486399536 ) ) ;
#12414 = CARTESIAN_POINT ( 'NONE',  ( 28.20905029452487156, -282.4827303476370730, -302.7418395665159210 ) ) ;
#12415 = CARTESIAN_POINT ( 'NONE',  ( -113.2063622782859227, -295.4816453028025762, -259.6568538004638071 ) ) ;
#12416 = CARTESIAN_POINT ( 'NONE',  ( -74.34057437189321149, -290.3340253990980955, -337.7203453135224436 ) ) ;
#12417 = CARTESIAN_POINT ( 'NONE',  ( -74.39217739053599132, -290.0235901612713292, -337.8060412764365879 ) ) ;
#12418 = CARTESIAN_POINT ( 'NONE',  ( 11.13247268856299321, -286.9121436349000760, -215.7106547222429072 ) ) ;
#12419 = VERTEX_POINT ( 'NONE', #17103 ) ;
#12420 = DIRECTION ( 'NONE',  ( -1.000000000000000000, 0.000000000000000000, 0.000000000000000000 ) ) ;
#12421 = CARTESIAN_POINT ( 'NONE',  ( -113.1030561598872879, -298.4217558035367688, -269.6383386235157218 ) ) ;
#12422 = CARTESIAN_POINT ( 'NONE',  ( -113.1110118654578258, -295.3715647831007232, -259.6688718474485427 ) ) ;
#12423 = CARTESIAN_POINT ( 'NONE',  ( -64.89355741687893442, -278.7419500879294105, -202.5060989468545358 ) ) ;
#12424 = EDGE_LOOP ( 'NONE', ( #66019, #79941, #54756, #43116, #88073, #25649 ) ) ;
#12425 = CARTESIAN_POINT ( 'NONE',  ( -0.06976037480313371231, -274.0420208480372821, -203.0384144344906190 ) ) ;
#12426 = CARTESIAN_POINT ( 'NONE',  ( -110.4951657120618052, -294.9103219988043634, -279.6744437218180792 ) ) ;
#12427 = CARTESIAN_POINT ( 'NONE',  ( -70.99188594780189021, -279.3615203784351024, -336.5315832779912171 ) ) ;
#12428 = CARTESIAN_POINT ( 'NONE',  ( 14.37384996976745022, -272.9283413867563581, -217.1035611763335851 ) ) ;
#12429 = CIRCLE ( 'NONE', #65386, 3.491568894204821749 ) ;
#12430 = CARTESIAN_POINT ( 'NONE',  ( -42.40186366650118543, -296.3224685553829545, -343.5835547771696383 ) ) ;
#12431 = CARTESIAN_POINT ( 'NONE',  ( -82.14384936096338663, -298.5046164229716510, -212.2709720357035792 ) ) ;
#12432 = DIRECTION ( 'NONE',  ( 0.000000000000000000, 0.000000000000000000, -1.000000000000000000 ) ) ;
#12433 = CARTESIAN_POINT ( 'NONE',  ( -66.59824771527503628, -297.0291252575901808, -340.7349231682601953 ) ) ;
#12434 = CIRCLE ( 'NONE', #17020, 1.000000000000000888 ) ;
#12435 = CARTESIAN_POINT ( 'NONE',  ( -34.81022065091374174, -296.0836149370950352, -195.1953032834341286 ) ) ;
#12436 = CARTESIAN_POINT ( 'NONE',  ( -44.31818114722263857, -292.6131409919578346, -197.5419570256928239 ) ) ;
#12437 = CARTESIAN_POINT ( 'NONE',  ( -97.04722166087842083, -288.5301040387733451, -313.3800163479940579 ) ) ;
#12438 = DIRECTION ( 'NONE',  ( -1.000000000000000000, 0.000000000000000000, 0.000000000000000000 ) ) ;
#12439 = CARTESIAN_POINT ( 'NONE',  ( 19.98582186219895718, -275.3472909304086897, -218.9692655756464035 ) ) ;
#12440 = EDGE_CURVE ( 'NONE', #64930, #48357, #47411, .T. ) ;
#12441 = CARTESIAN_POINT ( 'NONE',  ( -69.27061200015319287, -297.9533443617694388, -204.6904847166565844 ) ) ;
#12442 = ADVANCED_FACE ( 'NONE', ( #73480 ), #8592, .T. ) ;
#12443 = CIRCLE ( 'NONE', #35218, 9.103929867429224387 ) ;
#12444 = CARTESIAN_POINT ( 'NONE',  ( -79.02245826540124085, -281.4734479977473711, -207.5201611191039603 ) ) ;
#12445 = CARTESIAN_POINT ( 'NONE',  ( 20.70296369716275109, -279.5597516472616348, -220.5002922571243573 ) ) ;
#12446 = CARTESIAN_POINT ( 'NONE',  ( -34.30343725528067722, -276.3634805228944629, -347.1991407678876271 ) ) ;
#12447 = CARTESIAN_POINT ( 'NONE',  ( -22.69972827092026435, -278.6362677321605474, -195.5273926378769431 ) ) ;
#12448 = CARTESIAN_POINT ( 'NONE',  ( 32.62743136519172538, -279.1936863063045848, -242.7535163127353997 ) ) ;
#12449 = CARTESIAN_POINT ( 'NONE',  ( -36.71294846266656720, -272.6349288561673347, -196.7620574869183656 ) ) ;
#12450 = CARTESIAN_POINT ( 'NONE',  ( -90.13164947921488590, -279.7980435887648696, -323.7076269281154737 ) ) ;
#12451 = CARTESIAN_POINT ( 'NONE',  ( 208.4306832106270519, 1.063508326895939771, 7.500000000000014211 ) ) ;
#12452 = CARTESIAN_POINT ( 'NONE',  ( 197.2116943569230330, 276.0000000000000568, -12.92446933126074882 ) ) ;
#12453 = CARTESIAN_POINT ( 'NONE',  ( -84.56886566593212251, -295.6515786158510650, -210.8332350491017166 ) ) ;
#12454 = CARTESIAN_POINT ( 'NONE',  ( -5.886936586929241599, -292.4543296146415514, -200.0645569234314678 ) ) ;
#12455 = CARTESIAN_POINT ( 'NONE',  ( -3.526492729702133566, -278.6070885756623738, -337.5063666857230373 ) ) ;
#12456 = CARTESIAN_POINT ( 'NONE',  ( -62.68212315426065118, -271.7221775671806085, -199.7717164491168660 ) ) ;
#12457 = DIRECTION ( 'NONE',  ( 0.000000000000000000, 1.000000000000000000, 0.000000000000000000 ) ) ;
#12458 = CARTESIAN_POINT ( 'NONE',  ( -98.19926406807867636, -287.0795824094070667, -225.4902741566391171 ) ) ;
#12459 = ORIENTED_EDGE ( 'NONE', *, *, #52360, .T. ) ;
#12460 = CARTESIAN_POINT ( 'NONE',  ( 156.1243321211817374, 16.88031981476169108, -7.577257116167564810 ) ) ;
#12461 = CARTESIAN_POINT ( 'NONE',  ( 27.76270265590576969, -285.0541829863706198, -233.0237446742606267 ) ) ;
#12462 = DIRECTION ( 'NONE',  ( -0.000000000000000000, 0.000000000000000000, 1.000000000000000000 ) ) ;
#12463 = CARTESIAN_POINT ( 'NONE',  ( 35.22822260306186593, -292.4955694429547748, -281.6792842409594186 ) ) ;
#12464 = CARTESIAN_POINT ( 'NONE',  ( 16.89279779366137646, -284.9745043794812887, -219.6522674753275055 ) ) ;
#12465 = CARTESIAN_POINT ( 'NONE',  ( 153.9079962421555763, 20.48904911123736028, -11.76949543550875354 ) ) ;
#12466 = CARTESIAN_POINT ( 'NONE',  ( 30.18445706015723218, -291.9833174569805010, -303.1184909934207781 ) ) ;
#12467 = CARTESIAN_POINT ( 'NONE',  ( -104.8099393678581777, -283.4977786297754960, -234.6005336521887443 ) ) ;
#12468 = CARTESIAN_POINT ( 'NONE',  ( -57.34945749769401857, -281.3897339644024100, -199.3249999978065148 ) ) ;
#12469 = CARTESIAN_POINT ( 'NONE',  ( 36.30518844575019699, -288.4895252718519032, -249.0981684694154978 ) ) ;
#12470 = CARTESIAN_POINT ( 'NONE',  ( 0.8838624597298744279, -278.7942357344136326, -204.6294405367410434 ) ) ;
#12471 = CARTESIAN_POINT ( 'NONE',  ( 35.62999201901077129, -287.5969868136489822, -273.7598291364836314 ) ) ;
#12472 = CARTESIAN_POINT ( 'NONE',  ( -99.97873118599717657, -280.5069134843076313, -231.6377465715746951 ) ) ;
#12473 = CARTESIAN_POINT ( 'NONE',  ( -19.50506179501759618, -281.0901914715744851, -199.3548134191441363 ) ) ;
#12474 = CARTESIAN_POINT ( 'NONE',  ( -63.98964146788656393, -287.6862320653694383, -199.8611244874135480 ) ) ;
#12475 = ORIENTED_EDGE ( 'NONE', *, *, #37335, .F. ) ;
#12476 = CARTESIAN_POINT ( 'NONE',  ( -34.04482923856807020, -297.9256827530350051, -193.3612081204445019 ) ) ;
#12477 = CARTESIAN_POINT ( 'NONE',  ( -96.23301752009128052, -291.8998068935681545, -316.2474274031009145 ) ) ;
#12478 = DIRECTION ( 'NONE',  ( 1.000000000000000000, 0.000000000000000000, 0.000000000000000000 ) ) ;
#12479 = CARTESIAN_POINT ( 'NONE',  ( -111.2586520408596868, -292.6233781216987495, -305.9938812882205070 ) ) ;
#12480 = VERTEX_POINT ( 'NONE', #23739 ) ;
#12481 = CARTESIAN_POINT ( 'NONE',  ( 12.76187576679671487, -272.7485685143941510, -214.2588703792187346 ) ) ;
#12482 = FACE_OUTER_BOUND ( 'NONE', #51875, .T. ) ;
#12483 = CARTESIAN_POINT ( 'NONE',  ( -47.54483155135947214, -293.5796661298963386, -345.8749347531792750 ) ) ;
#12484 = CARTESIAN_POINT ( 'NONE',  ( -77.54060728728036622, -297.0045600447964489, -209.2918332226240068 ) ) ;
#12485 = CARTESIAN_POINT ( 'NONE',  ( -75.05424157569694898, -291.0844731753718406, -333.6884367479887032 ) ) ;
#12486 = CARTESIAN_POINT ( 'NONE',  ( 32.31580917044831835, -283.6426652404380775, -295.5288839550758553 ) ) ;
#12487 = CARTESIAN_POINT ( 'NONE',  ( -95.00164907939179670, -291.2944362752274401, -320.5002901026065274 ) ) ;
#12488 = CARTESIAN_POINT ( 'NONE',  ( -40.30279585126334041, -290.4037821986844392, -346.8236431289408301 ) ) ;
#12489 = CARTESIAN_POINT ( 'NONE',  ( -101.3285898918744294, -287.0781584886605060, -231.1382287861074758 ) ) ;
#12490 = CARTESIAN_POINT ( 'NONE',  ( -56.55870617511166643, -279.9778946840347658, -195.7426766231734234 ) ) ;
#12491 = CARTESIAN_POINT ( 'NONE',  ( -112.6828941468750713, -294.7134820151158578, -263.9675006785436722 ) ) ;
#12492 = CARTESIAN_POINT ( 'NONE',  ( -37.31638290146443637, -282.8851281031414260, -347.3741790559139417 ) ) ;
#12493 = CARTESIAN_POINT ( 'NONE',  ( 30.28916643297933575, -277.8182393984351393, -300.9704525998034796 ) ) ;
#12494 = CARTESIAN_POINT ( 'NONE',  ( -105.5795714935544112, -280.8376638359844151, -285.9686137636504668 ) ) ;
#12495 = CARTESIAN_POINT ( 'NONE',  ( 26.78150406902601333, -274.3346237493449848, -311.2288291974931553 ) ) ;
#12497 = CIRCLE ( 'NONE', #42763, 0.4999999999999938938 ) ;
#12496 = CARTESIAN_POINT ( 'NONE',  ( 160.5350683151633291, 275.0000000000000568, 7.500000000000000000 ) ) ;
#12498 = CARTESIAN_POINT ( 'NONE',  ( 34.28977249104462999, -281.2502315824781363, -284.8087857765748936 ) ) ;
#12499 = VECTOR ( 'NONE', #23598, 1000.000000000000000 ) ;
#12500 = CARTESIAN_POINT ( 'NONE',  ( -111.4394256844100539, -279.5121573902982277, -289.8428990881785126 ) ) ;
#12501 = CARTESIAN_POINT ( 'NONE',  ( -95.63002029292010775, -284.2877062388921559, -220.3285079794843853 ) ) ;
#12502 = CARTESIAN_POINT ( 'NONE',  ( 17.47378833182729707, -294.6087169952544969, -220.5543350787875738 ) ) ;
#12503 = CARTESIAN_POINT ( 'NONE',  ( -46.80208557936183666, -275.5340609822649185, -194.7506589084638904 ) ) ;
#12504 = CIRCLE ( 'NONE', #65458, 0.9999999999999896749 ) ;
#12505 = CARTESIAN_POINT ( 'NONE',  ( -97.43617757623091791, -274.5046614627762551, -223.0118618609506598 ) ) ;
#12506 = CARTESIAN_POINT ( 'NONE',  ( 180.7149167944524493, -12.49482340714361506, 9.974999999999996092 ) ) ;
#12507 = CARTESIAN_POINT ( 'NONE',  ( 25.37448573153797682, -275.8990968957646146, -307.7199192978276869 ) ) ;
#12508 = CARTESIAN_POINT ( 'NONE',  ( -97.05215672422032469, -297.9339028496198694, -315.4897544189734617 ) ) ;
#12509 = CARTESIAN_POINT ( 'NONE',  ( -109.1060049771863874, -282.8278768419540370, -248.9704584469216684 ) ) ;
#12510 = CIRCLE ( 'NONE', #41187, 1.000000000000000888 ) ;
#12511 = CARTESIAN_POINT ( 'NONE',  ( 28.03664500919741087, -292.6860013646905827, -229.6227672039093761 ) ) ;
#12512 = CARTESIAN_POINT ( 'NONE',  ( 36.73520837720445087, -273.6961219794714566, -279.9623556402026452 ) ) ;
#12513 = CARTESIAN_POINT ( 'NONE',  ( -12.46543918051157362, -290.3341975005167797, -342.4414945516092530 ) ) ;
#12514 = CARTESIAN_POINT ( 'NONE',  ( -92.78128892305208808, -290.1530917711041297, -222.3957339172780507 ) ) ;
#12515 = EDGE_LOOP ( 'NONE', ( #47451, #72161, #50155, #89688 ) ) ;
#12516 = CARTESIAN_POINT ( 'NONE',  ( -71.88949824125222676, -290.1792740998022282, -202.1919846057980124 ) ) ;
#12517 = CARTESIAN_POINT ( 'NONE',  ( -107.4143889406865355, -290.4910701331420455, -249.7763837881663846 ) ) ;
#12518 = EDGE_LOOP ( 'NONE', ( #63470, #92519, #40437, #82367, #32218 ) ) ;
#12519 = CARTESIAN_POINT ( 'NONE',  ( 37.07354313463295625, -288.3988865489286582, -251.8175454820308801 ) ) ;
#12520 = CARTESIAN_POINT ( 'NONE',  ( -107.9941173629488276, -279.1295116272421524, -251.8641349634359017 ) ) ;
#12521 = CARTESIAN_POINT ( 'NONE',  ( -93.47264148177617926, -294.7571209237502217, -322.6376151942385491 ) ) ;
#12522 = CARTESIAN_POINT ( 'NONE',  ( -113.7193609928771423, -285.3154080728642157, -261.4299530372964000 ) ) ;
#12523 = CARTESIAN_POINT ( 'NONE',  ( -111.7019020203254058, -285.1370244877222149, -250.2533294845411547 ) ) ;
#12524 = CARTESIAN_POINT ( 'NONE',  ( 19.37114671263906374, -282.5362602063959798, -316.3780075690812623 ) ) ;
#12525 = CARTESIAN_POINT ( 'NONE',  ( 173.9735501344063948, 243.4424551670193466, -179.7288663750133821 ) ) ;
#12526 = CARTESIAN_POINT ( 'NONE',  ( -100.6629394507023250, -246.7894274234220404, -333.2501944198467072 ) ) ;
#12527 = CARTESIAN_POINT ( 'NONE',  ( 44.32992207132367213, 11.63825656539217235, -328.4651697331042328 ) ) ;
#12528 = CARTESIAN_POINT ( 'NONE',  ( 15.57062826419014634, -274.0214327175541484, -219.7616671598360654 ) ) ;
#12529 = CARTESIAN_POINT ( 'NONE',  ( 34.46457528060756914, -274.6664670583908219, -285.1288153808118295 ) ) ;
#12530 = CARTESIAN_POINT ( 'NONE',  ( -112.2473314949235146, -295.8391929396597106, -287.9872224215492906 ) ) ;
#12531 = CARTESIAN_POINT ( 'NONE',  ( 26.68328070931609020, -24.59112382776695682, -341.9535762841285873 ) ) ;
#12532 = CARTESIAN_POINT ( 'NONE',  ( 38.82803177079595969, -274.1398807313123598, -262.6468285325606189 ) ) ;
#12533 = CARTESIAN_POINT ( 'NONE',  ( -36.75017892490402005, -275.8198262182843337, -196.3375581050478331 ) ) ;
#12534 = EDGE_LOOP ( 'NONE', ( #25226, #90067, #51275, #74225 ) ) ;
#12535 = CARTESIAN_POINT ( 'NONE',  ( -112.9699592356097213, -297.3245466989074544, -283.8212697521575478 ) ) ;
#12536 = CARTESIAN_POINT ( 'NONE',  ( -5.760160217979543695, -289.1176213097603522, -336.2443083940181054 ) ) ;
#12537 = AXIS2_PLACEMENT_3D ( 'NONE', #41206, #62576, #25166 ) ;
#12538 = CARTESIAN_POINT ( 'NONE',  ( -114.0719024077377952, -297.2925955457415625, -275.3391217207804971 ) ) ;
#12539 = CARTESIAN_POINT ( 'NONE',  ( -74.57108344939425137, -296.0257622879685755, -337.7520507797435130 ) ) ;
#12540 = CARTESIAN_POINT ( 'NONE',  ( -12.26220003297685324, -292.5542633796108021, -201.7505587413596118 ) ) ;
#12541 = ORIENTED_EDGE ( 'NONE', *, *, #17686, .T. ) ;
#12542 = CARTESIAN_POINT ( 'NONE',  ( 24.89496570573188805, -278.0497655484517736, -313.2992567531924237 ) ) ;
#12543 = VERTEX_POINT ( 'NONE', #52150 ) ;
#12544 = CARTESIAN_POINT ( 'NONE',  ( -3.678867409004826339, -279.9921397825090708, -201.1632268794262757 ) ) ;
#12545 = ADVANCED_BREP_SHAPE_REPRESENTATION ( '', ( #58557, #18940 ), #6864 ) ;
#12546 = CARTESIAN_POINT ( 'NONE',  ( -61.85733367897015000, -278.3198946977102537, -339.4251157334522873 ) ) ;
#12547 = CARTESIAN_POINT ( 'NONE',  ( 38.30620234176479499, -277.2147004842683486, -262.6604537507460577 ) ) ;
#12548 = CARTESIAN_POINT ( 'NONE',  ( -99.13156550678466772, -275.9896795546921453, -313.4936966241423306 ) ) ;
#12549 = CARTESIAN_POINT ( 'NONE',  ( -110.3430300130309263, -297.1530649146155270, -274.1949806450746223 ) ) ;
#12550 = CARTESIAN_POINT ( 'NONE',  ( -78.29258560499850716, -294.1893375310316969, -331.5651323288159347 ) ) ;
#12551 = CARTESIAN_POINT ( 'NONE',  ( 185.0172044724083946, 275.5000000000000568, 22.46007009812148425 ) ) ;
#12552 = CARTESIAN_POINT ( 'NONE',  ( -33.92428390281050099, -280.5864098914588567, -193.4985902482769973 ) ) ;
#12553 = EDGE_CURVE ( 'NONE', #60279, #70988, #6644, .T. ) ;
#12554 = CARTESIAN_POINT ( 'NONE',  ( 9.665668289305965999, -276.5505233591932779, -326.2118773234645346 ) ) ;
#12555 = CARTESIAN_POINT ( 'NONE',  ( 29.70750037557199263, -285.7554731685211209, -233.4041290271505034 ) ) ;
#12556 = CARTESIAN_POINT ( 'NONE',  ( -34.16995150064371245, -300.0919240008499855, -195.1933642773144300 ) ) ;
#12557 = CARTESIAN_POINT ( 'NONE',  ( 82.64619460822838448, -299.7668101228608748, -197.8578870376357202 ) ) ;
#12558 = VECTOR ( 'NONE', #2327, 1000.000000000000000 ) ;
#12559 = CARTESIAN_POINT ( 'NONE',  ( 19.63281298001173880, -287.3968030300295027, -316.2578126745939358 ) ) ;
#12560 = CARTESIAN_POINT ( 'NONE',  ( -49.28363519112350843, -278.1377146732341430, -197.3175405894177459 ) ) ;
#12562 = CARTESIAN_POINT ( 'NONE',  ( -34.82181443857170677, -281.1001297837638049, -344.7711413711398905 ) ) ;
#12561 = CARTESIAN_POINT ( 'NONE',  ( -46.51203322022012543, -278.5083584211845391, -197.2939903880773329 ) ) ;
#12563 = CARTESIAN_POINT ( 'NONE',  ( -42.90293920771659231, -287.9821445867680723, -195.5548116255564253 ) ) ;
#12564 = CARTESIAN_POINT ( 'NONE',  ( -93.90226149250428023, -279.0974685749752666, -317.1572238003803363 ) ) ;
#12565 = DIRECTION ( 'NONE',  ( 0.9693563597868444237, 0.2456588035076248677, 0.000000000000000000 ) ) ;
#12566 = VECTOR ( 'NONE', #35159, 1000.000000000000000 ) ;
#12567 = CARTESIAN_POINT ( 'NONE',  ( -83.06769276739125019, -293.4268758816918421, -210.8470617778256440 ) ) ;
#12568 = B_SPLINE_CURVE_WITH_KNOTS ( 'NONE', 3,
 ( #87513, #44438, #80422, #15567, #73344, #8455, #37336, #66242, #76598, #69487, #54801, #3698 ),
 .UNSPECIFIED., .F., .F.,
 ( 4, 2, 2, 2, 2, 4 ),
 ( 1.734723475976806902E-18, 0.002272214944544886147, 0.004544429889089770559, 0.006816644833634654538, 0.007952752305907110839, 0.009088859778179567139 ),
 .UNSPECIFIED. ) ;
#12569 = CARTESIAN_POINT ( 'NONE',  ( -35.75543595774144023, -275.2724075324279625, -346.3441802229037307 ) ) ;
#12570 = TOROIDAL_SURFACE ( 'NONE', #76095, 5.654241149514406040, 1.000000000000000000 ) ;
#12571 = CARTESIAN_POINT ( 'NONE',  ( 28.12548131681101893, -276.6453486622205560, -303.0012608549447464 ) ) ;
#12572 = CARTESIAN_POINT ( 'NONE',  ( 33.88036123089335661, -283.8642270593254011, -294.5531513830283075 ) ) ;
#12573 = AXIS2_PLACEMENT_3D ( 'NONE', #24059, #31186, #52473 ) ;
#12574 = DIRECTION ( 'NONE',  ( -1.000000000000000000, -0.000000000000000000, -0.000000000000000000 ) ) ;
#12575 = CARTESIAN_POINT ( 'NONE',  ( -71.23814853932458391, -291.4163005853861819, -337.8914444056980528 ) ) ;
#12576 = CIRCLE ( 'NONE', #36759, 24.50000000000000355 ) ;
#12577 = CARTESIAN_POINT ( 'NONE',  ( -108.1215329218913581, -294.8749532840054712, -245.4043380101404352 ) ) ;
#12578 = CARTESIAN_POINT ( 'NONE',  ( -54.91772352308628058, -285.0288881253230784, -195.5597662460230310 ) ) ;
#12579 = CARTESIAN_POINT ( 'NONE',  ( 207.6175730408114930, 30.32598770090644180, 14.41714557868295898 ) ) ;
#12580 = CARTESIAN_POINT ( 'NONE',  ( 24.21564609138414426, -273.6843904535077172, -230.2121876813570793 ) ) ;
#12581 = CARTESIAN_POINT ( 'NONE',  ( 35.27090687749453224, -291.8927658334631019, -285.8581534860165903 ) ) ;
#12582 = FACE_OUTER_BOUND ( 'NONE', #53992, .T. ) ;
#12583 = FACE_BOUND ( 'NONE', #70208, .T. ) ;
#12584 = CARTESIAN_POINT ( 'NONE',  ( -96.03307207509081422, -289.6939516939546593, -221.5758770953208909 ) ) ;
#12585 = CARTESIAN_POINT ( 'NONE',  ( -105.9502146030623777, -285.7908552118423131, -297.6904242434161461 ) ) ;
#12586 = CARTESIAN_POINT ( 'NONE',  ( 38.62744524904720578, -285.7713300987560956, -268.7292595337831358 ) ) ;
#12587 = AXIS2_PLACEMENT_3D ( 'NONE', #82070, #90103, #90549 ) ;
#12588 = CARTESIAN_POINT ( 'NONE',  ( -91.97073117390672792, -286.6785543492987927, -220.9806032714806463 ) ) ;
#12589 = CARTESIAN_POINT ( 'NONE',  ( -2.117599204566144255, -287.3336202621802613, -206.1804585664824003 ) ) ;
#12590 = CARTESIAN_POINT ( 'NONE',  ( -70.20369978855059401, -293.6011619459533222, -202.5489082699899370 ) ) ;
#12591 = CARTESIAN_POINT ( 'NONE',  ( 35.49094456198201897, -273.8893841493771788, -290.5269593316224359 ) ) ;
#12592 = CARTESIAN_POINT ( 'NONE',  ( 33.69239798872150260, -275.5065372135939583, -240.5603346329096155 ) ) ;
#12593 = CARTESIAN_POINT ( 'NONE',  ( -40.54640512744872893, -290.0920261457404195, -194.8561688827246599 ) ) ;
#12594 = CARTESIAN_POINT ( 'NONE',  ( -79.91078213175143219, -279.4938746968505825, -206.1342929073309449 ) ) ;
#12595 = CARTESIAN_POINT ( 'NONE',  ( -111.8556681748940349, -298.5890412720779068, -265.9434980272143889 ) ) ;
#12596 = DIRECTION ( 'NONE',  ( 0.000000000000000000, 0.000000000000000000, 1.000000000000000000 ) ) ;
#12597 = DIRECTION ( 'NONE',  ( 0.000000000000000000, 0.000000000000000000, 1.000000000000000000 ) ) ;
#12598 = CARTESIAN_POINT ( 'NONE',  ( -110.4834773936178607, -283.3375926751205043, -262.6819869511061825 ) ) ;
#12599 = CARTESIAN_POINT ( 'NONE',  ( -70.33130833008823402, -277.6171799092439301, -203.0061894027116693 ) ) ;
#12600 = CARTESIAN_POINT ( 'NONE',  ( 186.2362647323748206, 275.5000000000000568, 22.80382896336986320 ) ) ;
#12601 = CARTESIAN_POINT ( 'NONE',  ( -27.07050527769958137, -272.6602060880990734, -194.6959316172027457 ) ) ;
#12602 = CARTESIAN_POINT ( 'NONE',  ( -53.98518798882874847, -276.6199614661547344, -341.5954021164458254 ) ) ;
#12603 = CARTESIAN_POINT ( 'NONE',  ( 33.42131565614240429, -295.3424034750860301, -290.9808527754635179 ) ) ;
#12604 = CONICAL_SURFACE ( 'NONE', #27751, 2.738891987356051327, 0.09862129276975473147 ) ;
#12605 = CARTESIAN_POINT ( 'NONE',  ( -36.74111090155958692, -278.9798690578548985, -193.6595869428859373 ) ) ;
#12606 = CARTESIAN_POINT ( 'NONE',  ( -86.63954514880765601, -296.6990598476846799, -324.5195053651119679 ) ) ;
#12607 = CARTESIAN_POINT ( 'NONE',  ( -97.01221858130472242, -297.2213807722670253, -318.2642803681642931 ) ) ;
#12608 = CARTESIAN_POINT ( 'NONE',  ( -66.81739334731882707, -297.4881823881186165, -203.5628329864630928 ) ) ;
#12609 = CARTESIAN_POINT ( 'NONE',  ( -19.62372796187571566, -294.2800220444470938, -197.4303042952196563 ) ) ;
#12610 = CARTESIAN_POINT ( 'NONE',  ( -111.7217710860096389, -284.9704502704320248, -250.2457526416982319 ) ) ;
#12611 = CARTESIAN_POINT ( 'NONE',  ( 26.59355548651324597, -274.2343652001097780, -311.1106352812315663 ) ) ;
#12612 = CARTESIAN_POINT ( 'NONE',  ( 27.44364859138365986, -287.9325248714616237, -312.0750310898934003 ) ) ;
#12613 = CARTESIAN_POINT ( 'NONE',  ( -88.67975864015495802, -281.3078126908787340, -216.1024819155032901 ) ) ;
#12614 = CARTESIAN_POINT ( 'NONE',  ( -72.47639672715835957, -284.6337607506645782, -206.0898606211825381 ) ) ;
#12615 = CARTESIAN_POINT ( 'NONE',  ( -91.35361185486713964, -289.2840923545999203, -218.2515613434582065 ) ) ;
#12616 = CARTESIAN_POINT ( 'NONE',  ( 189.0118003482855613, 275.4351431090623237, -122.7278359107281887 ) ) ;
#12617 = CARTESIAN_POINT ( 'NONE',  ( 35.51273965628178075, -287.1406200928090016, -276.4927356085705128 ) ) ;
#12618 = CARTESIAN_POINT ( 'NONE',  ( 156.9594811538147781, 18.65395765032316788, 11.57852291560509883 ) ) ;
#12619 = CARTESIAN_POINT ( 'NONE',  ( 37.32232758360850511, -282.7177957728447382, -288.2526722765618388 ) ) ;
#12620 = CARTESIAN_POINT ( 'NONE',  ( -79.45528720899983455, -290.5574938977147212, -206.1160746953016769 ) ) ;
#12621 = CARTESIAN_POINT ( 'NONE',  ( -59.09347548110813619, -281.3753634609538494, -197.3316671921994896 ) ) ;
#12622 = CARTESIAN_POINT ( 'NONE',  ( -67.18563426773714298, -280.9841186722829320, -199.9151254167732930 ) ) ;
#12623 = CARTESIAN_POINT ( 'NONE',  ( 20.51722863426464016, -280.7587912809323711, -225.8285062069620039 ) ) ;
#12624 = CARTESIAN_POINT ( 'NONE',  ( 37.60176673436281192, -277.6041177088840186, -274.3954965778123096 ) ) ;
#12625 = CARTESIAN_POINT ( 'NONE',  ( -96.51141804342559283, -295.8891836041329952, -319.6557963897648733 ) ) ;
#12626 = CARTESIAN_POINT ( 'NONE',  ( -111.6068495014022801, -288.6692574196476926, -262.8421825658129478 ) ) ;
#12627 = EDGE_CURVE ( 'NONE', #76858, #24854, #75925, .T. ) ;
#12628 = CARTESIAN_POINT ( 'NONE',  ( -75.35923858213155313, -296.4530220869546611, -207.6213878589962860 ) ) ;
#12629 = ORIENTED_EDGE ( 'NONE', *, *, #43955, .F. ) ;
#12630 = VERTEX_POINT ( 'NONE', #45485 ) ;
#12631 = CARTESIAN_POINT ( 'NONE',  ( -67.11346878464723886, -285.3656372158049521, -338.6021921623116100 ) ) ;
#12632 = CARTESIAN_POINT ( 'NONE',  ( -104.7801134663028648, -296.5942811263462886, -242.3584771585584292 ) ) ;
#12633 = VECTOR ( 'NONE', #3593, 1000.000000000000000 ) ;
#12634 = CARTESIAN_POINT ( 'NONE',  ( 13.06492628264923717, -293.8170295869656456, -212.5626359711301347 ) ) ;
#12635 = CARTESIAN_POINT ( 'NONE',  ( -58.97038684478827264, -283.9907842108303271, -340.2433558536980058 ) ) ;
#12636 = CARTESIAN_POINT ( 'NONE',  ( 2.306766587584209383, -273.6284961275996466, -204.6281787519848194 ) ) ;
#12637 = CARTESIAN_POINT ( 'NONE',  ( -107.1713513255442649, -291.6175047298950176, -238.0296777572972644 ) ) ;
#12638 = CARTESIAN_POINT ( 'NONE',  ( -36.55408705261230295, -284.2015279658127724, -194.5875779140718578 ) ) ;
#12639 = CARTESIAN_POINT ( 'NONE',  ( -109.8442033155404971, -290.5570573798880787, -296.3866958251232973 ) ) ;
#12641 = CARTESIAN_POINT ( 'NONE',  ( 34.98190542943792991, -288.0194236988548369, -280.5211343545892078 ) ) ;
#12640 = CIRCLE ( 'NONE', #65589, 4.999999999999990230 ) ;
#12642 = LINE ( 'NONE', #14519, #26290 ) ;
#12643 = AXIS2_PLACEMENT_3D ( 'NONE', #42105, #72872, #7996 ) ;
#12644 = CARTESIAN_POINT ( 'NONE',  ( 154.7381521964306330, 128.4861308677204761, -12.50226176571347381 ) ) ;
#12645 = CARTESIAN_POINT ( 'NONE',  ( 198.7186473392949324, 285.8615890216420894, -96.28303562970221208 ) ) ;
#12646 = CARTESIAN_POINT ( 'NONE',  ( -38.70061381994710104, -284.5890215064887343, -346.6556859975646603 ) ) ;
#12647 = CARTESIAN_POINT ( 'NONE',  ( 21.27581636871891391, -291.6952119285919025, -317.1477375740089997 ) ) ;
#12648 = ORIENTED_EDGE ( 'NONE', *, *, #28991, .T. ) ;
#12649 = CARTESIAN_POINT ( 'NONE',  ( 12.11514108265188483, -281.2648853495474555, -324.4743966704918989 ) ) ;
#12650 = CARTESIAN_POINT ( 'NONE',  ( 26.04705649364418818, -275.7966940058047953, -314.1295641626779229 ) ) ;
#12651 = CARTESIAN_POINT ( 'NONE',  ( -102.1583477803547169, -280.0508082361629363, -307.8660742968231716 ) ) ;
#12652 = CARTESIAN_POINT ( 'NONE',  ( -75.49606648588520841, -209.3771256275476276, -355.3995788168579111 ) ) ;
#12653 = CARTESIAN_POINT ( 'NONE',  ( 34.77762986152587388, -279.8042023697440186, -244.9560258808108415 ) ) ;
#12655 = AXIS2_PLACEMENT_3D ( 'NONE', #19670, #75110, #76037 ) ;
#12654 = CARTESIAN_POINT ( 'NONE',  ( -109.9599198805907889, -282.7957885906049000, -253.0307059700666628 ) ) ;
#12656 = CARTESIAN_POINT ( 'NONE',  ( -108.4808413058894132, -297.9682693022463695, -297.2151912524603290 ) ) ;
#12657 = PRODUCT_DEFINITION_SHAPE ( 'NONE', 'NONE',  #79429 ) ;
#12658 = CARTESIAN_POINT ( 'NONE',  ( 14.91514181625562330, -293.3056538800829003, -219.2278077630834048 ) ) ;
#12659 = ORIENTED_EDGE ( 'NONE', *, *, #63702, .F. ) ;
#12660 = CARTESIAN_POINT ( 'NONE',  ( -52.45493329255374704, -290.5394774719989073, -198.3864549677211073 ) ) ;
#12661 = CARTESIAN_POINT ( 'NONE',  ( 1.003413464882473294, -277.2061890039088325, -337.0770896462618111 ) ) ;
#12662 = CARTESIAN_POINT ( 'NONE',  ( -60.51791045767454591, -297.9098365572439775, -201.0843626165640501 ) ) ;
#12663 = ORIENTED_EDGE ( 'NONE', *, *, #61955, .T. ) ;
#12664 = EDGE_CURVE ( 'NONE', #85724, #23580, #67046, .T. ) ;
#12665 = CARTESIAN_POINT ( 'NONE',  ( -81.06283476543683264, -272.3941941989601219, -207.2891952767791111 ) ) ;
#12666 = DIRECTION ( 'NONE',  ( 0.000000000000000000, 0.000000000000000000, -1.000000000000000000 ) ) ;
#12667 = SPHERICAL_SURFACE ( 'NONE', #59724, 3.000000000000000000 ) ;
#12668 = VECTOR ( 'NONE', #72103, 1000.000000000000000 ) ;
#12669 = EDGE_CURVE ( 'NONE', #31408, #10505, #9570, .T. ) ;
#12670 = CARTESIAN_POINT ( 'NONE',  ( 157.7670607448531541, 18.75975317436490286, 10.28854280544483402 ) ) ;
#12671 = AXIS2_PLACEMENT_3D ( 'NONE', #12024, #5415, #62226 ) ;
#12672 = CARTESIAN_POINT ( 'NONE',  ( 33.62620332539215440, -282.8740246278042036, -288.7900241679112696 ) ) ;
#12673 = CARTESIAN_POINT ( 'NONE',  ( 38.62658439766818930, -283.2706922622728030, -267.0784978993007712 ) ) ;
#12674 = CARTESIAN_POINT ( 'NONE',  ( -76.26229071936403159, -282.6447775006108714, -332.4581522303788006 ) ) ;
#12675 = CARTESIAN_POINT ( 'NONE',  ( 33.91367453616346950, -283.1417020225867418, -249.5395651381631126 ) ) ;
#12676 = CARTESIAN_POINT ( 'NONE',  ( -1.146417747012285604, -275.0428483524368630, -334.6108277334010381 ) ) ;
#12677 = DIRECTION ( 'NONE',  ( -0.000000000000000000, -0.000000000000000000, 1.000000000000000000 ) ) ;
#12678 = CARTESIAN_POINT ( 'NONE',  ( -100.9929541079603297, -274.1292678856114549, -233.8894580073142606 ) ) ;
#12679 = FACE_OUTER_BOUND ( 'NONE', #88112, .T. ) ;
#12680 = CARTESIAN_POINT ( 'NONE',  ( -103.4616172954073505, -278.8427701030904018, -309.6102358343944729 ) ) ;
#12681 = ORIENTED_EDGE ( 'NONE', *, *, #81096, .F. ) ;
#12682 = ORIENTED_EDGE ( 'NONE', *, *, #44981, .F. ) ;
#12683 = DIRECTION ( 'NONE',  ( 0.9693563597868433135, 0.2456588035076293641, 0.000000000000000000 ) ) ;
#12684 = CARTESIAN_POINT ( 'NONE',  ( -31.01105954805349896, -287.9917252804136183, -194.8481791191904904 ) ) ;
#12685 = CARTESIAN_POINT ( 'NONE',  ( 6.781745895150870673, -291.8673093068106823, -212.0025433129018211 ) ) ;
#12686 = EDGE_CURVE ( 'NONE', #44672, #9702, #66378, .T. ) ;
#12687 = CARTESIAN_POINT ( 'NONE',  ( 16.60852260737198804, -287.6580931582129210, -325.2319275647414543 ) ) ;
#12688 = CARTESIAN_POINT ( 'NONE',  ( -46.83290882217585249, -284.1699898011024175, -196.9073841552745137 ) ) ;
#12690 = CARTESIAN_POINT ( 'NONE',  ( 10.75701678634182734, -286.6167590674494932, -326.6826433891713464 ) ) ;
#12689 = CARTESIAN_POINT ( 'NONE',  ( -103.5506706064534086, -282.6941346864935554, -302.5990274579521611 ) ) ;
#12691 = CARTESIAN_POINT ( 'NONE',  ( -97.85104321354928913, -285.1810060938734637, -311.9918183803483771 ) ) ;
#12692 = CARTESIAN_POINT ( 'NONE',  ( 22.74954937165943392, -274.1649601502861060, -315.2392015557825857 ) ) ;
#12693 = CARTESIAN_POINT ( 'NONE',  ( -26.71232985919517944, -284.5849339588338012, -194.8531745398550186 ) ) ;
#12694 = CARTESIAN_POINT ( 'NONE',  ( -105.9539577227053826, -298.9505159662763276, -239.9446853690348576 ) ) ;
#12695 = CARTESIAN_POINT ( 'NONE',  ( -10.62127270455772710, -284.3995729523576870, -200.0486533792515615 ) ) ;
#12696 = AXIS2_PLACEMENT_3D ( 'NONE', #50032, #84451, #56067 ) ;
#12697 = CARTESIAN_POINT ( 'NONE',  ( 35.93841738125772878, -282.5058196220105060, -271.3048669382784510 ) ) ;
#12698 = CARTESIAN_POINT ( 'NONE',  ( 37.52611708050940109, -289.4593949972093014, -263.1082099610706564 ) ) ;
#12699 = CARTESIAN_POINT ( 'NONE',  ( 199.5070675535761495, 288.7003404203971400, -6.034989766317571558 ) ) ;
#12700 = DIRECTION ( 'NONE',  ( 0.000000000000000000, -0.000000000000000000, 1.000000000000000000 ) ) ;
#12701 = CARTESIAN_POINT ( 'NONE',  ( -3.844741996609786661, -296.5339779675770160, -338.1048239028524449 ) ) ;
#12702 = CARTESIAN_POINT ( 'NONE',  ( 3.822411524978964970, -278.6056800016013995, -207.6049561217071755 ) ) ;
#12703 = CARTESIAN_POINT ( 'NONE',  ( -113.5046801578881599, -289.8816134664136257, -259.8053904173704609 ) ) ;
#12704 = CARTESIAN_POINT ( 'NONE',  ( -73.71424022065239967, -293.9435149377666789, -334.5754368140970314 ) ) ;
#12705 = CARTESIAN_POINT ( 'NONE',  ( -99.87861719279139550, -277.7669087314573062, -231.6586605190708781 ) ) ;
#12706 = CARTESIAN_POINT ( 'NONE',  ( -37.12257269282081751, -296.1945163819850109, -196.1230835325061435 ) ) ;
#12707 = CARTESIAN_POINT ( 'NONE',  ( 35.91734243256483694, -294.9441356797200910, -276.2225307994201557 ) ) ;
#12708 = CARTESIAN_POINT ( 'NONE',  ( -106.6379572354042153, -298.6233781216988064, -303.7686719486574134 ) ) ;
#12709 = CARTESIAN_POINT ( 'NONE',  ( -57.19053941056941426, -296.2805962430873592, -196.6264160508500822 ) ) ;
#12710 = CARTESIAN_POINT ( 'NONE',  ( -33.56698644350797167, -290.3389179041185457, -194.4682622474768721 ) ) ;
#12711 = CARTESIAN_POINT ( 'NONE',  ( -110.2866629565564267, -292.1095333635684028, -260.2661270485664318 ) ) ;
#12712 = CARTESIAN_POINT ( 'NONE',  ( 165.2494399300530290, 8.542400036368780647, 10.00000000000000000 ) ) ;
#12713 = CARTESIAN_POINT ( 'NONE',  ( -25.39276830906507243, -293.0110508689361950, -198.1304107910130767 ) ) ;
#12714 = CARTESIAN_POINT ( 'NONE',  ( 161.2244399300530233, 8.542400036368780647, 13.00000000000000178 ) ) ;
#12715 = CARTESIAN_POINT ( 'NONE',  ( -84.03651937796948346, -292.6319190584698617, -209.5686206708755321 ) ) ;
#12717 = CARTESIAN_POINT ( 'NONE',  ( -9.727477383730715133, -292.4230616058530359, -202.7317849118470576 ) ) ;
#12716 = CARTESIAN_POINT ( 'NONE',  ( 33.78377332379238851, -279.2496718533679996, -245.3138771476903912 ) ) ;
#12718 = AXIS2_PLACEMENT_3D ( 'NONE', #17331, #4052, #91117 ) ;
#12719 = CARTESIAN_POINT ( 'NONE',  ( 29.28658259053174007, -281.0502294714270306, -231.7648494845747962 ) ) ;
#12720 = CARTESIAN_POINT ( 'NONE',  ( -34.48400638747325075, -282.6838719749498523, -347.2869126035777185 ) ) ;
#12721 = CARTESIAN_POINT ( 'NONE',  ( -73.26066703526196022, -287.5294987995197289, -336.0106133696477855 ) ) ;
#12722 = CARTESIAN_POINT ( 'NONE',  ( -10.55175458754369444, -280.8386386964761527, -339.6482790735918798 ) ) ;
#12723 = CARTESIAN_POINT ( 'NONE',  ( -33.92675524242982732, -278.5742659129874141, -194.1309014981059988 ) ) ;
#12724 = AXIS2_PLACEMENT_3D ( 'NONE', #43548, #6, #35985 ) ;
#12725 = CARTESIAN_POINT ( 'NONE',  ( -36.55473865310689519, -284.9821459890060282, -193.6612795405494580 ) ) ;
#12726 = DIRECTION ( 'NONE',  ( -0.000000000000000000, -1.000000000000000000, -0.000000000000000000 ) ) ;
#12727 = CARTESIAN_POINT ( 'NONE',  ( 35.69659821302300884, -295.0142856207962154, -259.7853253038214234 ) ) ;
#12728 = CARTESIAN_POINT ( 'NONE',  ( 9.137444172736250536, -276.1016893901243066, -209.7121655071458122 ) ) ;
#12729 = CARTESIAN_POINT ( 'NONE',  ( -110.4131071039217176, -278.2152713700334061, -270.6338982105727382 ) ) ;
#12730 = CARTESIAN_POINT ( 'NONE',  ( -108.7976714184257361, -290.3547422290420741, -299.0498644076387791 ) ) ;
#12731 = AXIS2_PLACEMENT_3D ( 'NONE', #60106, #75231, #52048 ) ;
#12732 = CARTESIAN_POINT ( 'NONE',  ( -101.7045171753228772, -282.1048300662653787, -309.9432096195405961 ) ) ;
#12733 = CARTESIAN_POINT ( 'NONE',  ( 0.03942425826137266331, -291.6217399924299798, -207.3844557355665188 ) ) ;
#12734 = CARTESIAN_POINT ( 'NONE',  ( -95.86329552514342822, -293.9065832499758244, -317.2879913062499213 ) ) ;
#12735 = ORIENTED_EDGE ( 'NONE', *, *, #61465, .T. ) ;
#12736 = LINE ( 'NONE', #78986, #59005 ) ;
#12737 = AXIS2_PLACEMENT_3D ( 'NONE', #90881, #26997, #70096 ) ;
#12738 = CARTESIAN_POINT ( 'NONE',  ( -77.28356070118236687, -291.0080949154977361, -209.1840290069833088 ) ) ;
#12739 = DIRECTION ( 'NONE',  ( -1.000000000000000000, 0.000000000000000000, 0.000000000000000000 ) ) ;
#12740 = CARTESIAN_POINT ( 'NONE',  ( -6.941161984400256557, -277.9809262143061233, -207.3071070584150277 ) ) ;
#12741 = CARTESIAN_POINT ( 'NONE',  ( -110.9930382571182292, -295.3381014873089612, -292.0477620371522107 ) ) ;
#12742 = CARTESIAN_POINT ( 'NONE',  ( -6.707720012253735042, -278.5896021565122282, -201.0515836639664826 ) ) ;
#12743 = CARTESIAN_POINT ( 'NONE',  ( -85.77714865942333233, -285.0220606485902977, -329.5836271914230338 ) ) ;
#12744 = CARTESIAN_POINT ( 'NONE',  ( 9.032126467930954306, -286.5429111326134830, -213.9832126354646391 ) ) ;
#12745 = CARTESIAN_POINT ( 'NONE',  ( 5.818377028963960917, -277.9756536651902366, -330.1561749321234061 ) ) ;
#12746 = CARTESIAN_POINT ( 'NONE',  ( -110.8923452054956300, -294.7365372722920256, -257.6273277775270572 ) ) ;
#12747 = CARTESIAN_POINT ( 'NONE',  ( -56.03793337859627144, -297.0562554884706401, -342.0272453920001112 ) ) ;
#12748 = AXIS2_PLACEMENT_3D ( 'NONE', #65973, #86780, #19704 ) ;
#12749 = CARTESIAN_POINT ( 'NONE',  ( -61.93726522194137374, -276.1739129192278597, -339.5685261531830292 ) ) ;
#12750 = EDGE_LOOP ( 'NONE', ( #90163, #51490, #34785, #16257 ) ) ;
#12751 = CARTESIAN_POINT ( 'NONE',  ( 194.7541945649814181, 39.97853125882125624, 13.97297966198307506 ) ) ;
#12752 = CARTESIAN_POINT ( 'NONE',  ( -105.9407881765222470, -295.7676562329083367, -305.4057536379166891 ) ) ;
#12753 = CARTESIAN_POINT ( 'NONE',  ( -99.29584816917089540, -291.9102256989351076, -311.6517058737210846 ) ) ;
#12754 = CARTESIAN_POINT ( 'NONE',  ( 200.1063562618922447, 64.94916223748940354, -5.267193185415704804 ) ) ;
#12755 = EDGE_CURVE ( 'NONE', #31130, #21613, #7616, .T. ) ;
#12756 = CARTESIAN_POINT ( 'NONE',  ( -68.79432972687121151, -290.1283612228955349, -336.3506986745339304 ) ) ;
#12757 = VERTEX_POINT ( 'NONE', #89504 ) ;
#12758 = CARTESIAN_POINT ( 'NONE',  ( -48.07399228421011372, -278.9776893724890101, -194.2966627046170345 ) ) ;
#12759 = CARTESIAN_POINT ( 'NONE',  ( -112.2046537130600967, -296.9827680700414589, -287.9922031837843974 ) ) ;
#12760 = CARTESIAN_POINT ( 'NONE',  ( -71.59233948002955117, -289.7442008569637437, -202.7656983099762442 ) ) ;
#12761 = CARTESIAN_POINT ( 'NONE',  ( -26.21778484358500450, -298.5211383845050932, -193.3816517618556645 ) ) ;
#12762 = CARTESIAN_POINT ( 'NONE',  ( 12.91463599043121313, -293.1108799237808284, -217.3857636499863588 ) ) ;
#12763 = DIRECTION ( 'NONE',  ( 0.000000000000000000, 1.000000000000000000, 0.000000000000000000 ) ) ;
#12764 = CARTESIAN_POINT ( 'NONE',  ( 175.2296996224750103, 276.0000000000000568, 24.50000000000000355 ) ) ;
#12765 = CARTESIAN_POINT ( 'NONE',  ( -7.176037701193298979, -290.1837073577079877, -340.4661767328307747 ) ) ;
#12766 = CARTESIAN_POINT ( 'NONE',  ( -99.86837403722181250, -280.4090924074130839, -320.2651865833026363 ) ) ;
#12767 = ORIENTED_EDGE ( 'NONE', *, *, #11727, .T. ) ;
#12768 = CARTESIAN_POINT ( 'NONE',  ( 10.76571107480143397, -280.0456659282253327, -210.3012804972890990 ) ) ;
#12769 = CARTESIAN_POINT ( 'NONE',  ( -98.87766549156962981, -287.1312837310651389, -227.7549693876415802 ) ) ;
#12770 = CARTESIAN_POINT ( 'NONE',  ( 17.93786329305483918, -285.3993143061658770, -217.5327653407140929 ) ) ;
#12771 = CARTESIAN_POINT ( 'NONE',  ( -88.57024709705110865, -271.3319616237362766, -215.7405433434926749 ) ) ;
#12772 = CARTESIAN_POINT ( 'NONE',  ( -27.11609820263379333, -276.1031604155282366, -196.5748878261711923 ) ) ;
#12773 = CARTESIAN_POINT ( 'NONE',  ( -110.3558600276854662, -288.4435754079615890, -284.9263076712960583 ) ) ;
#12774 = CARTESIAN_POINT ( 'NONE',  ( 38.15176543325043923, -277.4939952727524428, -276.7675316607811169 ) ) ;
#12775 = ORIENTED_EDGE ( 'NONE', *, *, #36530, .T. ) ;
#12777 = CARTESIAN_POINT ( 'NONE',  ( -19.50166052244104620, -279.6361796699416686, -199.4171059962247057 ) ) ;
#12776 = CARTESIAN_POINT ( 'NONE',  ( -108.1720813378868229, -278.3184213534494802, -288.0777871115324160 ) ) ;
#12778 = CARTESIAN_POINT ( 'NONE',  ( -45.60259956673103687, -278.2340497529474987, -346.6586354221760757 ) ) ;
#12779 = CARTESIAN_POINT ( 'NONE',  ( -99.91572761369815225, -277.9348204407071421, -226.1740180188839986 ) ) ;
#12780 = CARTESIAN_POINT ( 'NONE',  ( -107.8763801708993384, -260.0240351709692845, -316.1980822346592390 ) ) ;
#12781 = CARTESIAN_POINT ( 'NONE',  ( -10.44133255412179473, -275.3358280256182411, -198.4074893679850788 ) ) ;
#12782 = CONTEXT_DEPENDENT_SHAPE_REPRESENTATION ( #23308, #58842 ) ;
#12783 = CARTESIAN_POINT ( 'NONE',  ( -31.97937589946915793, -299.5433120510044205, -193.9490722229001847 ) ) ;
#12784 = EDGE_CURVE ( 'NONE', #7661, #1451, #82169, .T. ) ;
#12785 = CARTESIAN_POINT ( 'NONE',  ( -85.28047601435908120, -292.1948066931273615, -330.5268031993605859 ) ) ;
#12786 = ORIENTED_EDGE ( 'NONE', *, *, #57360, .F. ) ;
#12787 = AXIS2_PLACEMENT_3D ( 'NONE', #11028, #90097, #10100 ) ;
#12788 = CARTESIAN_POINT ( 'NONE',  ( 139.6539576904058606, 275.0000000000000568, -10.49999999999999822 ) ) ;
#12789 = CARTESIAN_POINT ( 'NONE',  ( 12.37549240880803225, -289.4201731558272286, -324.3042861944137485 ) ) ;
#12790 = CARTESIAN_POINT ( 'NONE',  ( 26.27695026892089913, -288.7590823455798841, -228.8082440162733349 ) ) ;
#12791 = CARTESIAN_POINT ( 'NONE',  ( -23.77438266417697221, -288.2229187652478117, -342.2447789095239727 ) ) ;
#12792 = CARTESIAN_POINT ( 'NONE',  ( -102.4630494542463595, -284.5967666444706197, -229.3887277045673159 ) ) ;
#12793 = CARTESIAN_POINT ( 'NONE',  ( 18.58395493326880654, -279.2735022965443932, -222.1881921483092697 ) ) ;
#12794 = CARTESIAN_POINT ( 'NONE',  ( -42.78799873117153396, -287.8431525050246478, -196.3131295468711812 ) ) ;
#12795 = CARTESIAN_POINT ( 'NONE',  ( 34.13273993873682599, -279.7967935555730037, -252.3623101591499562 ) ) ;
#12796 = CARTESIAN_POINT ( 'NONE',  ( -108.7729123399310396, -280.0938733723111227, -253.0745509007568046 ) ) ;
#12797 = CARTESIAN_POINT ( 'NONE',  ( -76.38340974404744088, -278.0816915890506493, -332.1760475079382786 ) ) ;
#12798 = CARTESIAN_POINT ( 'NONE',  ( 14.32451743060643601, -287.1402686412513958, -326.9892462897971654 ) ) ;
#12799 = CARTESIAN_POINT ( 'NONE',  ( -0.4439788245232155206, -283.3773613274281615, -337.7757075228396388 ) ) ;
#12800 = CARTESIAN_POINT ( 'NONE',  ( -52.89903591155184870, -283.7386127523722053, -345.7647274539809814 ) ) ;
#12801 = CARTESIAN_POINT ( 'NONE',  ( 34.56672463139790352, -281.5529226777233589, -257.7842164114974253 ) ) ;
#12802 = ORIENTED_EDGE ( 'NONE', *, *, #68670, .T. ) ;
#12803 = ORIENTED_EDGE ( 'NONE', *, *, #37560, .F. ) ;
#12804 = CARTESIAN_POINT ( 'NONE',  ( 159.4851178187871312, 15.00000000000000000, -10.00000000000000000 ) ) ;
#12805 = CARTESIAN_POINT ( 'NONE',  ( -95.64379628515675336, -293.0739427394873360, -221.9554113389173722 ) ) ;
#12806 = CARTESIAN_POINT ( 'NONE',  ( 8.568464601607562514, -291.3508187861314696, -209.0940478909424485 ) ) ;
#12807 = AXIS2_PLACEMENT_3D ( 'NONE', #61227, #25668, #2969 ) ;
#12808 = CARTESIAN_POINT ( 'NONE',  ( 35.83640159367509170, -274.6631786878368757, -274.3373165245678251 ) ) ;
#12809 = EDGE_CURVE ( 'NONE', #47975, #62368, #77199, .T. ) ;
#12810 = CARTESIAN_POINT ( 'NONE',  ( -13.82111854622414171, -294.1033084075639863, -343.5737878452090968 ) ) ;
#12811 = CARTESIAN_POINT ( 'NONE',  ( -85.14939795273411960, -288.2058409473071379, -326.5099619300196423 ) ) ;
#12812 = CARTESIAN_POINT ( 'NONE',  ( 23.43264825056165179, -291.2110688170663479, -228.0959965685837290 ) ) ;
#12813 = CARTESIAN_POINT ( 'NONE',  ( -95.25444729854719128, -291.1251159771306902, -315.4729269737616733 ) ) ;
#12814 = CARTESIAN_POINT ( 'NONE',  ( 154.1407330040854333, 250.5000000000000568, -13.42592592592594158 ) ) ;
#12815 = CARTESIAN_POINT ( 'NONE',  ( -111.6871824480867019, -292.6841544288588466, -260.0930899425639495 ) ) ;
#12816 = CARTESIAN_POINT ( 'NONE',  ( -112.1789260973729512, -288.6489151968917781, -262.7955414915831511 ) ) ;
#12817 = CARTESIAN_POINT ( 'NONE',  ( 18.97023693299322389, -294.8637363602957748, -220.8045126366333477 ) ) ;
#12818 = CARTESIAN_POINT ( 'NONE',  ( 0.2792775019406475434, -287.5074061434601731, -207.4683283593129488 ) ) ;
#12819 = CARTESIAN_POINT ( 'NONE',  ( 14.23956241590369665, -296.3295367544030796, -325.0365400558924875 ) ) ;
#12820 = CARTESIAN_POINT ( 'NONE',  ( 199.0061125298537377, 215.0000000000000568, -7.725424859374024678 ) ) ;
#12821 = CARTESIAN_POINT ( 'NONE',  ( 1.547107284693248319, -276.5491691831819594, -205.8160371446255397 ) ) ;
#12822 = AXIS2_PLACEMENT_3D ( 'NONE', #68164, #3284, #53949 ) ;
#12823 = CARTESIAN_POINT ( 'NONE',  ( -40.42352086366273767, -297.2116406593179931, -193.5324033616849420 ) ) ;
#12824 = CARTESIAN_POINT ( 'NONE',  ( -16.11134798781873556, -275.0138508440573446, -341.3179334723345164 ) ) ;
#12825 = CARTESIAN_POINT ( 'NONE',  ( -41.09990449428941872, -278.0843240821507152, -196.0160435026627681 ) ) ;
#12826 = CARTESIAN_POINT ( 'NONE',  ( -96.61105071479227036, -274.3611641720453349, -226.9837623274275984 ) ) ;
#12827 = AXIS2_PLACEMENT_3D ( 'NONE', #33571, #79493, #86098 ) ;
#12828 = EDGE_CURVE ( 'NONE', #62353, #11375, #20287, .T. ) ;
#12829 = CARTESIAN_POINT ( 'NONE',  ( -92.62139973357824374, -297.2895323889403585, -318.9361087662082923 ) ) ;
#12830 = CARTESIAN_POINT ( 'NONE',  ( -98.86356132045459333, -296.8071256839359080, -310.0476217724072967 ) ) ;
#12831 = FACE_OUTER_BOUND ( 'NONE', #38015, .T. ) ;
#12833 = CARTESIAN_POINT ( 'NONE',  ( -57.90478048487656793, -297.7790149154793653, -200.3171337566467400 ) ) ;
#12832 = CARTESIAN_POINT ( 'NONE',  ( 37.45469921927907109, -285.6946673156867291, -279.9396689795746056 ) ) ;
#12834 = CARTESIAN_POINT ( 'NONE',  ( 18.35149761149446945, -286.8243567422333626, -217.1121641910426092 ) ) ;
#12835 = CARTESIAN_POINT ( 'NONE',  ( -41.76358626444396549, -288.7731194933020902, -347.2260848123033270 ) ) ;
#12836 = CARTESIAN_POINT ( 'NONE',  ( -67.54193801458228563, -299.6379745472079321, -201.2667484842886836 ) ) ;
#12837 = CARTESIAN_POINT ( 'NONE',  ( -45.31066793678635918, -293.1530363351437813, -344.8206848949831738 ) ) ;
#12838 = CARTESIAN_POINT ( 'NONE',  ( 24.46794854450271117, -280.1414208134771116, -224.7132686151190342 ) ) ;
#12839 = CARTESIAN_POINT ( 'NONE',  ( -4.771743288812454686, -283.9809262143061233, -202.8022627189028810 ) ) ;
#12840 = DIRECTION ( 'NONE',  ( -0.000000000000000000, -0.000000000000000000, -1.000000000000000000 ) ) ;
#12841 = CARTESIAN_POINT ( 'NONE',  ( 22.27530300331472546, -286.9423534689038888, -313.1740067325638961 ) ) ;
#12842 = DIRECTION ( 'NONE',  ( 0.000000000000000000, 0.000000000000000000, 1.000000000000000000 ) ) ;
#12843 = CARTESIAN_POINT ( 'NONE',  ( -56.60315071815340104, -287.3001343420163494, -342.8995813082674431 ) ) ;
#12844 = CARTESIAN_POINT ( 'NONE',  ( -41.93830527140335107, -299.5933930275830903, -196.7044031693784234 ) ) ;
#12845 = CARTESIAN_POINT ( 'NONE',  ( 3.491637004783563647, -282.0146376710927711, -205.7134519838564870 ) ) ;
#12847 = CARTESIAN_POINT ( 'NONE',  ( 17.60485798695175319, -282.2378917936061953, -318.4222847527424847 ) ) ;
#12846 = CARTESIAN_POINT ( 'NONE',  ( -54.20210191688631340, -295.8567615428426052, -196.9163519930568498 ) ) ;
#12848 = CARTESIAN_POINT ( 'NONE',  ( -84.18352103965089839, -295.8426409876597063, -331.5417106358412411 ) ) ;
#12849 = CARTESIAN_POINT ( 'NONE',  ( -110.7781188841123310, -274.0490587354074137, -264.8875579083942284 ) ) ;
#12850 = CARTESIAN_POINT ( 'NONE',  ( 37.36559402475907632, -285.4866337887550571, -258.9551431836123925 ) ) ;
#12851 = CARTESIAN_POINT ( 'NONE',  ( 28.94201066895371000, -283.0857735435578206, -235.1581556957312102 ) ) ;
#12852 = CARTESIAN_POINT ( 'NONE',  ( -37.13695615579317888, -297.1135314523854163, -197.1229975639101610 ) ) ;
#12853 = ORIENTED_EDGE ( 'NONE', *, *, #17274, .F. ) ;
#12854 = CARTESIAN_POINT ( 'NONE',  ( 180.7287904564219332, 275.0000000000000568, -24.90000000000003411 ) ) ;
#12855 = CARTESIAN_POINT ( 'NONE',  ( -108.5474871138090549, -286.2417338954609818, -292.7571601043123337 ) ) ;
#12856 = CARTESIAN_POINT ( 'NONE',  ( -186.9122233887894140, -89.54582641780471874, -21.50000000000000000 ) ) ;
#12857 = CARTESIAN_POINT ( 'NONE',  ( -2.659677404128736544, -274.1237833571632905, -342.4524372437778652 ) ) ;
#12858 = CARTESIAN_POINT ( 'NONE',  ( 39.15757917469888127, -274.6521396190461246, -262.6068260781826780 ) ) ;
#12859 = CARTESIAN_POINT ( 'NONE',  ( -67.79925558043403555, -291.4742574353348914, -204.0048084319964516 ) ) ;
#12860 = CARTESIAN_POINT ( 'NONE',  ( -65.56348126283084810, -284.9481178865611355, -338.4500877506414440 ) ) ;
#12861 = CARTESIAN_POINT ( 'NONE',  ( 34.95230614102256794, -277.3458333096415913, -285.1940905349864011 ) ) ;
#12862 = CARTESIAN_POINT ( 'NONE',  ( -113.7382910024855533, -286.0177996698006950, -267.1573561207084140 ) ) ;
#12863 = CARTESIAN_POINT ( 'NONE',  ( -69.19529939205334301, -282.2757161854602828, -336.4997186565072980 ) ) ;
#12864 = CARTESIAN_POINT ( 'NONE',  ( -52.24914702988790793, -281.8615825267725654, -196.8044388012513366 ) ) ;
#12865 = CARTESIAN_POINT ( 'NONE',  ( -7.692542024774548182, -274.5967035126004134, -199.2416801386512759 ) ) ;
#12866 = CARTESIAN_POINT ( 'NONE',  ( 22.75968331239080911, -274.7405064548540281, -222.2068134651589162 ) ) ;
#12867 = CARTESIAN_POINT ( 'NONE',  ( -109.9920108096132907, -298.2624124991974099, -286.5859927051400291 ) ) ;
#12868 = CIRCLE ( 'NONE', #34010, 0.4999999999999985567 ) ;
#12869 = EDGE_CURVE ( 'NONE', #63051, #82273, #55004, .T. ) ;
#12870 = CARTESIAN_POINT ( 'NONE',  ( 160.5350683151633291, 250.0000000000000568, 20.22542485937379908 ) ) ;
#12871 = CARTESIAN_POINT ( 'NONE',  ( -109.1821406003631978, -294.3837371573162613, -294.4288680343846636 ) ) ;
#12872 = CARTESIAN_POINT ( 'NONE',  ( 33.64483044088866137, -275.2883494617894939, -287.7025516250984651 ) ) ;
#12873 = CARTESIAN_POINT ( 'NONE',  ( -57.69426220730361621, -287.5460253404503419, -199.1477575376319464 ) ) ;
#12874 = AXIS2_PLACEMENT_3D ( 'NONE', #38352, #67266, #36976 ) ;
#12875 = CARTESIAN_POINT ( 'NONE',  ( -1.018999310745072329, -296.0991715007161247, -337.4830177702351079 ) ) ;
#12876 = CARTESIAN_POINT ( 'NONE',  ( -16.59956865210886434, -295.9951589218848653, -344.1573245609079663 ) ) ;
#12877 = CARTESIAN_POINT ( 'NONE',  ( -98.84141721499349842, -291.9725364720823109, -313.0194412108830306 ) ) ;
#12878 = CARTESIAN_POINT ( 'NONE',  ( -109.7399485568272723, -276.7964472466167081, -251.3761731370418602 ) ) ;
#12879 = CARTESIAN_POINT ( 'NONE',  ( -100.7060863049831028, -281.0017155072604282, -231.1952410859327358 ) ) ;
#12880 = CARTESIAN_POINT ( 'NONE',  ( -70.38483200865748302, -293.5710378368185047, -337.0654329635964928 ) ) ;
#12881 = CARTESIAN_POINT ( 'NONE',  ( -78.46902979880994167, -285.4598642992408486, -333.9916785110635260 ) ) ;
#12882 = AXIS2_PLACEMENT_3D ( 'NONE', #24997, #53869, #64289 ) ;
#12883 = CARTESIAN_POINT ( 'NONE',  ( -103.7597201120072583, -283.8911662319997617, -239.2106381586119142 ) ) ;
#12884 = CARTESIAN_POINT ( 'NONE',  ( 46.98483951095349909, 11.15615824186278005, -331.1643732653742518 ) ) ;
#12885 = ORIENTED_EDGE ( 'NONE', *, *, #48330, .F. ) ;
#12886 = CARTESIAN_POINT ( 'NONE',  ( -102.2552504324740994, -284.6733491823260351, -236.9198489641671301 ) ) ;
#12887 = ORIENTED_EDGE ( 'NONE', *, *, #85032, .T. ) ;
#12888 = CARTESIAN_POINT ( 'NONE',  ( -3.018798571468261471, -283.6890445247593675, -338.9572776022216658 ) ) ;
#12889 = CARTESIAN_POINT ( 'NONE',  ( -108.6531869413102811, -283.7051868586116257, -242.2405080801414670 ) ) ;
#12890 = CARTESIAN_POINT ( 'NONE',  ( -103.2158630380051534, -280.0100581557256874, -230.8443507147514993 ) ) ;
#12891 = CLOSED_SHELL ( 'NONE', ( #10384, #55547, #52294, #52932, #69157, #65, #91315, #23330, #5457, #87661, #20887, #25465, #65910, #36404, #88027, #50712, #73319, #74739, #15971, #51544, #56439, #20906, #78512, #62357, #38799, #26815, #84374, #51967, #23454, #44619, #24725, #66306, #82902, #76916, #71878, #71024, #78352, #77875, #50999, #93461, #93687, #65131, #36314, #57046, #85549, #48216, #36009, #53886, #73628, #56259, #72074, #87370, #2293, #361, #39249, #82139, #29537, #78861, #44512, #45415, #32468, #66676, #60125, #59950, #64549, #31870, #61165, #88420, #61089, #64336, #85860, #19859, #58095, #83200, #9635, #13313, #70090, #80042, #61953, #48034, #71460, #20269, #25549, #12442, #93296, #53587, #25147, #61188, #44387, #89731, #39023, #77158, #62925, #5708, #60651, #80248, #61339, #12996, #23035, #32868, #60761, #78811, #15814, #43232, #48494, #42514, #85563, #41728, #88796 ) ) ;
#12892 = CARTESIAN_POINT ( 'NONE',  ( -112.6120434078924575, -279.9140996689043845, -282.8944007058090051 ) ) ;
#12893 = CARTESIAN_POINT ( 'NONE',  ( -8.906525419621885931, -281.0659159457808869, -198.9135594103130416 ) ) ;
#12894 = CARTESIAN_POINT ( 'NONE',  ( -53.35057174420112602, -274.7666405000204009, -340.3538533559490702 ) ) ;
#12895 = CARTESIAN_POINT ( 'NONE',  ( 175.2421902450908533, 242.6932815909999306, -179.6955966096621466 ) ) ;
#12896 = EDGE_LOOP ( 'NONE', ( #75994, #73754, #68849, #92774 ) ) ;
#12897 = CARTESIAN_POINT ( 'NONE',  ( -36.74644463627333835, -276.0598066089866052, -195.5174214593769193 ) ) ;
#12898 = CARTESIAN_POINT ( 'NONE',  ( 44.42952696178269179, 12.78217976624798879, -331.7054304614241005 ) ) ;
#12899 = CARTESIAN_POINT ( 'NONE',  ( -77.69020372323333845, -277.5280634081740914, -207.4994738444986808 ) ) ;
#12900 = CARTESIAN_POINT ( 'NONE',  ( -11.51897694432051900, -294.1439391656043085, -198.8414213500067547 ) ) ;
#12901 = CARTESIAN_POINT ( 'NONE',  ( -69.77674570138822219, -294.8395733358574944, -335.8734106245736939 ) ) ;
#12902 = CARTESIAN_POINT ( 'NONE',  ( -108.7436840526381587, -289.6958211182744094, -299.0191638811032817 ) ) ;
#12904 = CARTESIAN_POINT ( 'NONE',  ( -65.37846775173028391, -284.0794418382948834, -202.0397517839834052 ) ) ;
#12903 = CARTESIAN_POINT ( 'NONE',  ( -68.00650040173375999, -294.0216715123015661, -340.3488048878853078 ) ) ;
#12905 = CARTESIAN_POINT ( 'NONE',  ( -103.5212993092666096, -292.8630687204117748, -236.6150369288597233 ) ) ;
#12906 = CARTESIAN_POINT ( 'NONE',  ( -11.76335267563215758, -284.8712125508853887, -201.2492095016121993 ) ) ;
#12907 = CARTESIAN_POINT ( 'NONE',  ( -83.08869381652628761, -285.0083970499785551, -327.9455883539226306 ) ) ;
#12908 = VERTEX_POINT ( 'NONE', #41173 ) ;
#12909 = CARTESIAN_POINT ( 'NONE',  ( -77.05782195959486103, -292.4753047542684499, -204.6077246947470485 ) ) ;
#12910 = CARTESIAN_POINT ( 'NONE',  ( -34.83815681930158803, -283.5122410187837545, -343.3921976036638171 ) ) ;
#12911 = CARTESIAN_POINT ( 'NONE',  ( -113.3787734148549617, -295.4639119296739977, -261.0674532495754647 ) ) ;
#12912 = CARTESIAN_POINT ( 'NONE',  ( -108.6448071687833306, -290.9907923289092082, -298.9972096576212834 ) ) ;
#12913 = CARTESIAN_POINT ( 'NONE',  ( -71.87322625413527533, -289.9887247457808144, -339.1150313759645769 ) ) ;
#12914 = CARTESIAN_POINT ( 'NONE',  ( 17.77479428399139749, -287.0364495593480001, -222.4949289944469797 ) ) ;
#12915 = ORIENTED_EDGE ( 'NONE', *, *, #92, .T. ) ;
#12916 = LINE ( 'NONE', #34670, #44242 ) ;
#12917 = CARTESIAN_POINT ( 'NONE',  ( -94.63171407982453331, -297.7318221147525605, -319.9409504139586602 ) ) ;
#12918 = CARTESIAN_POINT ( 'NONE',  ( -110.3375233717847550, -295.5287121118184928, -247.2747539743806158 ) ) ;
#12919 = CARTESIAN_POINT ( 'NONE',  ( -19.46555647645083553, -279.3463875274569546, -199.2885757961579429 ) ) ;
#12920 = CARTESIAN_POINT ( 'NONE',  ( 28.45317866480812086, -274.5376530778539177, -230.3774195733493855 ) ) ;
#12921 = CARTESIAN_POINT ( 'NONE',  ( -104.5770583508462153, -294.6280095406722808, -300.6540327414994067 ) ) ;
#12922 = CARTESIAN_POINT ( 'NONE',  ( 19.98044599088153817, -277.9663116656553257, -317.2014515432399548 ) ) ;
#12923 = CARTESIAN_POINT ( 'NONE',  ( -79.53803314091729249, -271.6154073949409167, -209.2222210029422058 ) ) ;
#12924 = CARTESIAN_POINT ( 'NONE',  ( -23.42860723102124254, -296.0755340508383711, -342.4793376116002150 ) ) ;
#12925 = CARTESIAN_POINT ( 'NONE',  ( -6.622910189156639760, -295.7186998073491395, -336.9237352633185765 ) ) ;
#12926 = LINE ( 'NONE', #63595, #29365 ) ;
#12927 = CARTESIAN_POINT ( 'NONE',  ( -44.69789722621516859, -296.7437646801308802, -346.2580642009152712 ) ) ;
#12928 = B_SPLINE_CURVE_WITH_KNOTS ( 'NONE', 3,
 ( #81962, #10926, #16644, #31788, #2456, #67324 ),
 .UNSPECIFIED., .F., .F.,
 ( 4, 2, 4 ),
 ( -4.472146915492242146E-06, 0.0004206930844425495024, 0.0008458583158005913028 ),
 .UNSPECIFIED. ) ;
#12929 = CARTESIAN_POINT ( 'NONE',  ( -33.42740386265555941, -296.1008865582589920, -195.1957734180984119 ) ) ;
#12930 = CARTESIAN_POINT ( 'NONE',  ( -83.90032894964507193, -292.0440802214554878, -214.0034499143460778 ) ) ;
#12931 = CARTESIAN_POINT ( 'NONE',  ( -31.28301405184805972, -274.9296399455838014, -193.7485750489041720 ) ) ;
#12932 = CARTESIAN_POINT ( 'NONE',  ( -98.61123969104716025, -288.5653390216393177, -311.1445675930501693 ) ) ;
#12933 = DIRECTION ( 'NONE',  ( 0.000000000000000000, 0.000000000000000000, -1.000000000000000000 ) ) ;
#12934 = CARTESIAN_POINT ( 'NONE',  ( -46.87958923498909058, -274.4264582998733886, -194.0161405805469030 ) ) ;
#12935 = CARTESIAN_POINT ( 'NONE',  ( -102.7852251685376785, -296.4450991252521703, -302.8672277728502422 ) ) ;
#12936 = CARTESIAN_POINT ( 'NONE',  ( 26.44532598430231829, -282.9940970792346775, -230.1432839529457794 ) ) ;
#12937 = CARTESIAN_POINT ( 'NONE',  ( 18.80967482594860130, -279.5246084189157045, -218.3965015245213408 ) ) ;
#12938 = ADVANCED_FACE ( 'NONE', ( #34587 ), #33864, .F. ) ;
#12939 = CARTESIAN_POINT ( 'NONE',  ( -54.11710349943030707, -276.6105596820148662, -345.4616639157244435 ) ) ;
#12940 = CARTESIAN_POINT ( 'NONE',  ( 38.91001426787408235, -279.9468928874801463, -269.9550827114948106 ) ) ;
#12941 = CARTESIAN_POINT ( 'NONE',  ( 26.31271014087302262, -279.0146858653869799, -230.2867233043065198 ) ) ;
#12942 = EDGE_CURVE ( 'NONE', #25794, #79714, #33168, .T. ) ;
#12943 = CARTESIAN_POINT ( 'NONE',  ( -31.27317142014541318, -272.7049893050045739, -197.0097824073637582 ) ) ;
#12944 = CARTESIAN_POINT ( 'NONE',  ( -112.2832128605261772, -280.5002450324488450, -274.4165853928661818 ) ) ;
#12945 = CARTESIAN_POINT ( 'NONE',  ( 82.12347693879148380, -301.5478687382300222, -195.3203844934047311 ) ) ;
#12946 = PLANE ( 'NONE',  #14081 ) ;
#12947 = CARTESIAN_POINT ( 'NONE',  ( -35.47996997805969954, -296.3150216663414085, -194.3749935974277037 ) ) ;
#12948 = CARTESIAN_POINT ( 'NONE',  ( -47.49624196822620092, -289.9439384386781740, -195.6405958643876204 ) ) ;
#12949 = CARTESIAN_POINT ( 'NONE',  ( -64.38880357372521246, -291.7088732485124183, -198.2115734829788494 ) ) ;
#12950 = CARTESIAN_POINT ( 'NONE',  ( 37.31975202022893967, -277.6693848268944862, -279.4991216609959679 ) ) ;
#12951 = CARTESIAN_POINT ( 'NONE',  ( 4.054503818188253561, -272.6092366707648580, -207.7582114533805111 ) ) ;
#12952 = DIRECTION ( 'NONE',  ( 0.000000000000000000, 1.000000000000000000, 0.000000000000000000 ) ) ;
#12953 = CARTESIAN_POINT ( 'NONE',  ( -19.23923631631214448, -284.7412941686194472, -343.7745435736915169 ) ) ;
#12954 = CARTESIAN_POINT ( 'NONE',  ( 209.4353741342548005, 38.08050248846151220, 13.99694255477028015 ) ) ;
#12955 = CARTESIAN_POINT ( 'NONE',  ( -9.014712081650293030, -284.4224206629857008, -200.9026544543546322 ) ) ;
#12956 = FACE_OUTER_BOUND ( 'NONE', #43600, .T. ) ;
#12957 = CARTESIAN_POINT ( 'NONE',  ( 23.25216914410762215, -292.9213619464269414, -311.8687276326587039 ) ) ;
#12958 = CARTESIAN_POINT ( 'NONE',  ( -5.243467808546058428, -284.6186346517775405, -203.4100468069346164 ) ) ;
#12959 = CARTESIAN_POINT ( 'NONE',  ( 19.47122598114649961, -292.2309370901153329, -319.3428406447990824 ) ) ;
#12960 = CARTESIAN_POINT ( 'NONE',  ( -41.55043331426213626, -281.5839976357776209, -346.6034860639621797 ) ) ;
#12961 = CARTESIAN_POINT ( 'NONE',  ( -108.7517935008075085, -280.3961540006297923, -251.6824428764662400 ) ) ;
#12962 = CARTESIAN_POINT ( 'NONE',  ( 38.16286399629263570, -288.5937650722264607, -257.3585025162579427 ) ) ;
#12963 = CARTESIAN_POINT ( 'NONE',  ( 33.63291808743266387, -280.1402041058048553, -297.5010807902614829 ) ) ;
#12964 = CARTESIAN_POINT ( 'NONE',  ( -2.186385233618647117, -286.5309173464250989, -206.3270319700781386 ) ) ;
#12965 = CARTESIAN_POINT ( 'NONE',  ( -77.15578709489253129, -280.9326792680672611, -208.4116458274089894 ) ) ;
#12966 = CARTESIAN_POINT ( 'NONE',  ( 25.26919453014395245, -281.8339834524051639, -232.4148785957278847 ) ) ;
#12967 = CARTESIAN_POINT ( 'NONE',  ( -75.30046551474629268, -287.5290830154123682, -205.2046368264381329 ) ) ;
#12968 = ORIENTED_EDGE ( 'NONE', *, *, #50836, .T. ) ;
#12969 = CARTESIAN_POINT ( 'NONE',  ( -99.09116807551103534, -296.9975421848020005, -224.3390779066832863 ) ) ;
#12970 = CARTESIAN_POINT ( 'NONE',  ( -103.8870829031500591, -292.9825257437038886, -236.4300764022034684 ) ) ;
#12971 = DIRECTION ( 'NONE',  ( -0.9693563597868444237, -0.2456588035076248677, -0.000000000000000000 ) ) ;
#12972 = EDGE_CURVE ( 'NONE', #34180, #5640, #63025, .T. ) ;
#12973 = CARTESIAN_POINT ( 'NONE',  ( -88.47809603358389552, -298.1948066931273615, -334.5364918783848793 ) ) ;
#12974 = ORIENTED_EDGE ( 'NONE', *, *, #37852, .F. ) ;
#12975 = CARTESIAN_POINT ( 'NONE',  ( -49.39943109210859973, -271.8987596746026156, -196.1153375487108690 ) ) ;
#12976 = CARTESIAN_POINT ( 'NONE',  ( -79.05622870561278148, -294.0045880868150334, -334.1289666190540402 ) ) ;
#12977 = CARTESIAN_POINT ( 'NONE',  ( -66.83843959832350379, -297.1625678877363157, -203.5048449782682951 ) ) ;
#12978 = CARTESIAN_POINT ( 'NONE',  ( 20.91739395978089888, -289.7020571447915813, -315.5101034797131661 ) ) ;
#12979 = CARTESIAN_POINT ( 'NONE',  ( 33.94136413198724256, -283.5719364506622355, -290.2784161074279154 ) ) ;
#12980 = CARTESIAN_POINT ( 'NONE',  ( -98.54619287633666147, -291.3638534986807826, -316.1278726033087310 ) ) ;
#12981 = CARTESIAN_POINT ( 'NONE',  ( -106.0631321381372345, -291.4313685608193509, -304.1068196155210330 ) ) ;
#12982 = CARTESIAN_POINT ( 'NONE',  ( -60.62300076900870494, -287.7502956331037467, -199.0660852843546138 ) ) ;
#12983 = CARTESIAN_POINT ( 'NONE',  ( -6.232313260442182923, -280.6163704206869625, -199.9110166355659999 ) ) ;
#12984 = CARTESIAN_POINT ( 'NONE',  ( 12.42859662767392059, -292.4455311813479170, -327.2831899499475981 ) ) ;
#12985 = CARTESIAN_POINT ( 'NONE',  ( 25.92911623498276441, -281.9654566476276614, -314.2682874409046008 ) ) ;
#12986 = CARTESIAN_POINT ( 'NONE',  ( -8.512653817610086548, -276.2938300422520683, -201.8975937578110802 ) ) ;
#12987 = CARTESIAN_POINT ( 'NONE',  ( -53.35057174420112602, -282.3376638359844151, -200.3683826091709648 ) ) ;
#12988 = CARTESIAN_POINT ( 'NONE',  ( 25.21966653337349840, -274.3700642518234645, -313.5804427869251185 ) ) ;
#12989 = DIRECTION ( 'NONE',  ( -0.000000000000000000, -1.000000000000000000, -0.000000000000000000 ) ) ;
#12990 = CARTESIAN_POINT ( 'NONE',  ( 34.12670680731089590, -280.8590426642495004, -255.1273190691508717 ) ) ;
#12991 = CARTESIAN_POINT ( 'NONE',  ( -95.83599969088056980, -279.0871572331816424, -319.8427136825275738 ) ) ;
#12992 = CARTESIAN_POINT ( 'NONE',  ( -38.10416821729442205, -275.3575766837120113, -196.8719206675939120 ) ) ;
#12993 = CARTESIAN_POINT ( 'NONE',  ( -18.22898541540989115, -285.3512484480527860, -195.9588593539383794 ) ) ;
#12994 = CARTESIAN_POINT ( 'NONE',  ( -107.9115756068716934, -292.0185642881020271, -292.8433918286247604 ) ) ;
#12995 = CARTESIAN_POINT ( 'NONE',  ( -107.3506509167288385, -274.5410603450831104, -240.1412642514910374 ) ) ;
#12996 = ADVANCED_FACE ( 'NONE', ( #91856 ), #63494, .T. ) ;
#12997 = CARTESIAN_POINT ( 'NONE',  ( -94.72774099892640720, -274.5568185179035368, -219.7632861451976964 ) ) ;
#12998 = CARTESIAN_POINT ( 'NONE',  ( 157.4851178187871312, 1.000000000000001332, 7.000000000000000000 ) ) ;
#13000 = EDGE_CURVE ( 'NONE', #13010, #67402, #11210, .T. ) ;
#12999 = CARTESIAN_POINT ( 'NONE',  ( -5.067995457303488216, -276.4484191422664594, -335.8533099289364259 ) ) ;
#13001 = CARTESIAN_POINT ( 'NONE',  ( -83.47038087616263624, -297.6859669677472198, -329.3523175785386456 ) ) ;
#13002 = CARTESIAN_POINT ( 'NONE',  ( -95.53196003705915018, -283.2013669065388513, -223.2884845940816660 ) ) ;
#13003 = CARTESIAN_POINT ( 'NONE',  ( 39.63502101225977015, -293.1823495328365539, -267.4416400126836493 ) ) ;
#13004 = CARTESIAN_POINT ( 'NONE',  ( 18.65273970250616387, -274.2618134532861518, -319.7409997881770778 ) ) ;
#13005 = CARTESIAN_POINT ( 'NONE',  ( 38.83979864417077721, -289.1310588803307269, -268.6819341795176683 ) ) ;
#13006 = CARTESIAN_POINT ( 'NONE',  ( -81.90610081340983584, -290.3491984532741981, -212.0882981895577188 ) ) ;
#13007 = ORIENTED_EDGE ( 'NONE', *, *, #56360, .T. ) ;
#13008 = CARTESIAN_POINT ( 'NONE',  ( -68.07498969488386820, -290.2312129412768513, -200.3892241402413958 ) ) ;
#13009 = CARTESIAN_POINT ( 'NONE',  ( -89.82856992196482793, -290.9522623577512377, -219.5948300937954514 ) ) ;
#13010 = VERTEX_POINT ( 'NONE', #18035 ) ;
#13011 = CARTESIAN_POINT ( 'NONE',  ( 29.85406381361815775, -288.1499330768536424, -233.2885271821867263 ) ) ;
#13012 = CARTESIAN_POINT ( 'NONE',  ( -106.2827641536922272, -278.5635628395485810, -294.5813718221854742 ) ) ;
#13013 = CARTESIAN_POINT ( 'NONE',  ( -30.63174672532532483, -293.8895191435576635, -346.7579047930188381 ) ) ;
#13014 = CARTESIAN_POINT ( 'NONE',  ( -110.5859223994486626, -284.9082078208705298, -293.8266679287471561 ) ) ;
#13015 = CARTESIAN_POINT ( 'NONE',  ( -106.9847104616108169, -284.4652246864134213, -303.1573891596178782 ) ) ;
#13016 = CARTESIAN_POINT ( 'NONE',  ( -7.240884720463841795, -282.9794092498300984, -336.9032389114767057 ) ) ;
#13017 = CARTESIAN_POINT ( 'NONE',  ( 25.45548143946952280, -22.91915814266209139, -345.1898414876856123 ) ) ;
#13018 = CARTESIAN_POINT ( 'NONE',  ( -84.98129659660571633, -218.6007500822886698, -351.5046871484345274 ) ) ;
#13019 = CARTESIAN_POINT ( 'NONE',  ( -111.8582150891662650, -270.5933945666634486, -270.3361783062999848 ) ) ;
#13020 = CARTESIAN_POINT ( 'NONE',  ( 33.39571117036256709, -274.9953942226081836, -289.0378513739431696 ) ) ;
#13021 = CARTESIAN_POINT ( 'NONE',  ( 20.93559475271237957, -273.8494510930563024, -225.8659299357156272 ) ) ;
#13022 = CARTESIAN_POINT ( 'NONE',  ( -104.5522034484624356, -295.5727186817607048, -307.9170098336240926 ) ) ;
#13023 = CARTESIAN_POINT ( 'NONE',  ( 197.5414458789393279, 281.6342289571271635, -110.4094420167315747 ) ) ;
#13024 = CARTESIAN_POINT ( 'NONE',  ( 38.64572984594678218, -274.3545847953408270, -279.7044014839854640 ) ) ;
#13025 = CARTESIAN_POINT ( 'NONE',  ( -109.3792446928450062, -298.6458408137543188, -252.3797673348543356 ) ) ;
#13026 = CARTESIAN_POINT ( 'NONE',  ( -90.99475429689738348, -292.3472438696775271, -220.3868148038729942 ) ) ;
#13027 = EDGE_LOOP ( 'NONE', ( #34980, #88322 ) ) ;
#13028 = CARTESIAN_POINT ( 'NONE',  ( -113.8872091155850086, -297.5744272293689505, -263.9022236224023459 ) ) ;
#13029 = AXIS2_PLACEMENT_3D ( 'NONE', #44407, #79937, #16464 ) ;
#13030 = CARTESIAN_POINT ( 'NONE',  ( -29.16001087379421008, -289.4380187972297449, -342.9631041988759534 ) ) ;
#13031 = CARTESIAN_POINT ( 'NONE',  ( -104.4568706530885862, -296.8676899480395264, -307.8825977626626695 ) ) ;
#13032 = CARTESIAN_POINT ( 'NONE',  ( -13.79491257405529936, -295.2468845651835636, -343.6077950334290563 ) ) ;
#13033 = CARTESIAN_POINT ( 'NONE',  ( 33.94934584891574758, -293.5109205467754805, -254.6002432636048525 ) ) ;
#13034 = ORIENTED_EDGE ( 'NONE', *, *, #47255, .T. ) ;
#13035 = CARTESIAN_POINT ( 'NONE',  ( 23.22826953505513004, -278.0846408482625520, -315.5340410194270362 ) ) ;
#13036 = CARTESIAN_POINT ( 'NONE',  ( 34.26944720202351391, -280.7012568199019711, -242.0843685209363798 ) ) ;
#13037 = CARTESIAN_POINT ( 'NONE',  ( 33.47276509706586722, -276.7391968001456917, -289.0351631674133728 ) ) ;
#13038 = CARTESIAN_POINT ( 'NONE',  ( 19.26578590883388031, -276.6148802463860648, -219.5929287616562249 ) ) ;
#13039 = CARTESIAN_POINT ( 'NONE',  ( -34.38149873138987545, -275.0352162665833475, -345.6581565222509766 ) ) ;
#13040 = CARTESIAN_POINT ( 'NONE',  ( -110.1526375655736416, -297.2966128626596287, -263.2980455959078654 ) ) ;
#13041 = CARTESIAN_POINT ( 'NONE',  ( -71.21807424455170121, -294.0831976299256212, -335.7033590814297668 ) ) ;
#13042 = DIRECTION ( 'NONE',  ( -0.000000000000000000, -1.000000000000000000, -0.000000000000000000 ) ) ;
#13043 = CARTESIAN_POINT ( 'NONE',  ( -114.1497829663616272, -279.1005366207717771, -265.8839186587057384 ) ) ;
#13044 = CARTESIAN_POINT ( 'NONE',  ( 30.27882968814611075, -276.0888587007171964, -297.9995209854804443 ) ) ;
#13045 = CARTESIAN_POINT ( 'NONE',  ( -23.85626398058290221, -284.9056691563109780, -194.9982742528010817 ) ) ;
#13046 = CARTESIAN_POINT ( 'NONE',  ( -64.89429579173447848, -299.6934189820075289, -200.3706295696523512 ) ) ;
#13047 = CARTESIAN_POINT ( 'NONE',  ( 215.9306832106270804, -199.2391364535880882, 9.184850993605165694E-16 ) ) ;
#13048 = CARTESIAN_POINT ( 'NONE',  ( 35.84217703549991541, -286.7224235668668371, -268.3181286021995788 ) ) ;
#13049 = CARTESIAN_POINT ( 'NONE',  ( -88.21104146923185851, -277.5683815971250965, -216.5289483050232207 ) ) ;
#13052 = ADVANCED_FACE ( 'NONE', ( #4756 ), #85609, .F. ) ;
#13051 = CARTESIAN_POINT ( 'NONE',  ( -87.92492737254799806, -281.8453857191601060, -325.0453156086622926 ) ) ;
#13050 = CARTESIAN_POINT ( 'NONE',  ( -106.9966160351694384, -277.4416931496293159, -246.4651712220571653 ) ) ;
#13053 = CARTESIAN_POINT ( 'NONE',  ( -41.52575460317072498, -287.9996389986643521, -195.4652721004907789 ) ) ;
#13054 = CARTESIAN_POINT ( 'NONE',  ( -73.02167804767384496, -278.7412739595085895, -334.5165905436804792 ) ) ;
#13055 = DIRECTION ( 'NONE',  ( 0.000000000000000000, 1.000000000000000000, 0.000000000000000000 ) ) ;
#13056 = CARTESIAN_POINT ( 'NONE',  ( 21.52209751963951945, -294.9138446577944137, -223.8642244884936474 ) ) ;
#13057 = CARTESIAN_POINT ( 'NONE',  ( -94.46403227200600838, -276.1049076941987437, -320.4711288144811192 ) ) ;
#13058 = CARTESIAN_POINT ( 'NONE',  ( 32.15613502198027618, -275.9012243513387261, -247.5280129497101598 ) ) ;
#13059 = CARTESIAN_POINT ( 'NONE',  ( 5.891857655372181313, -284.4680844835685321, -331.9137060373463441 ) ) ;
#13060 = CARTESIAN_POINT ( 'NONE',  ( 41.08708295871279859, -293.9068999365417199, -472.6442049081569508 ) ) ;
#13061 = CARTESIAN_POINT ( 'NONE',  ( 30.40733201666325414, -289.9117772095127066, -303.9363763766240254 ) ) ;
#13062 = CARTESIAN_POINT ( 'NONE',  ( -99.37396939430259124, -295.1236747451754354, -228.1168886516929035 ) ) ;
#13063 = CARTESIAN_POINT ( 'NONE',  ( 198.6884013828325521, 64.61450673763174279, -9.555809373750800972 ) ) ;
#13064 = CARTESIAN_POINT ( 'NONE',  ( 11.88921313126211565, -273.4378169972527530, -215.7255500305664100 ) ) ;
#13065 = CARTESIAN_POINT ( 'NONE',  ( -25.18384741761302337, -290.3482310621494662, -197.0759035933843393 ) ) ;
#13066 = CARTESIAN_POINT ( 'NONE',  ( 138.4517698930976621, 181.0451598467585939, -241.7086681466011271 ) ) ;
#13067 = DIRECTION ( 'NONE',  ( -0.000000000000000000, -0.000000000000000000, 1.000000000000000000 ) ) ;
#13068 = CARTESIAN_POINT ( 'NONE',  ( -113.4946700605296286, -289.0931220403244311, -265.5203616729537544 ) ) ;
#13069 = CARTESIAN_POINT ( 'NONE',  ( -109.4979902225110351, -285.9493890096130713, -285.9100982614749569 ) ) ;
#13070 = CARTESIAN_POINT ( 'NONE',  ( 32.93096371817990331, -285.4181899331740624, -241.3146186784875340 ) ) ;
#13071 = CARTESIAN_POINT ( 'NONE',  ( -69.04509906562462618, -287.0520909847288635, -203.9373558796297914 ) ) ;
#13072 = CARTESIAN_POINT ( 'NONE',  ( -33.23980564483053257, -286.9078165065594135, -197.2647899026690936 ) ) ;
#13073 = CARTESIAN_POINT ( 'NONE',  ( -73.90340961557159005, -293.5488941257589772, -204.4699334168999769 ) ) ;
#13074 = CARTESIAN_POINT ( 'NONE',  ( 13.88854926926081212, -274.4205738416655436, -325.9730657272613712 ) ) ;
#13075 = CARTESIAN_POINT ( 'NONE',  ( 28.48226406185101567, -275.3631484397516260, -230.3474458447223299 ) ) ;
#13076 = CARTESIAN_POINT ( 'NONE',  ( -112.5706509030317903, -288.7289087283336926, -262.7570976468396680 ) ) ;
#13077 = CARTESIAN_POINT ( 'NONE',  ( -34.29109513770518447, -277.0147884556819236, -347.3006644407546446 ) ) ;
#13078 = CARTESIAN_POINT ( 'NONE',  ( -64.13638638193125985, -297.3831825584928765, -340.0857498392702496 ) ) ;
#13079 = CARTESIAN_POINT ( 'NONE',  ( -48.18343439338445933, -248.5908816770286762, -477.2051880179521959 ) ) ;
#13080 = DIRECTION ( 'NONE',  ( 1.000000000000000000, -0.000000000000000000, 0.000000000000000000 ) ) ;
#13081 = CARTESIAN_POINT ( 'NONE',  ( -96.32749537631258363, -282.6262012106118391, -314.2008196018245485 ) ) ;
#13082 = CARTESIAN_POINT ( 'NONE',  ( -74.00735558725403962, -277.5648361339606254, -204.9345915605718460 ) ) ;
#13083 = CARTESIAN_POINT ( 'NONE',  ( 202.4316997032785537, 63.54496854667812755, 6.999999999999996447 ) ) ;
#13084 = CARTESIAN_POINT ( 'NONE',  ( -36.92391245623485929, -272.5372109556587361, -194.0426576421041318 ) ) ;
#13085 = CARTESIAN_POINT ( 'NONE',  ( -56.63505139962715873, -276.6559627413939211, -340.9236851857388046 ) ) ;
#13086 = CARTESIAN_POINT ( 'NONE',  ( 35.52649840252095714, -295.2203273087150706, -281.6905790513746979 ) ) ;
#13087 = CARTESIAN_POINT ( 'NONE',  ( 31.74898901914198390, -280.0423713706244939, -236.9527273951630661 ) ) ;
#13088 = CARTESIAN_POINT ( 'NONE',  ( -97.36938833928104486, -296.9102845637692667, -312.3144861001824211 ) ) ;
#13089 = CARTESIAN_POINT ( 'NONE',  ( -41.89933291420142325, -296.4234854456285575, -346.7841541728756170 ) ) ;
#13090 = CARTESIAN_POINT ( 'NONE',  ( -96.09905745091680274, -296.9928507279720975, -227.0205856304320662 ) ) ;
#13091 = CARTESIAN_POINT ( 'NONE',  ( -105.3811154459989439, -292.9668639513399739, -238.8073763842450603 ) ) ;
#13092 = CARTESIAN_POINT ( 'NONE',  ( -85.51456223545741864, -285.5733461173820729, -210.2913638556467788 ) ) ;
#13093 = CARTESIAN_POINT ( 'NONE',  ( -100.1707604848266300, -271.2597680969976182, -227.9261168779661659 ) ) ;
#13094 = CARTESIAN_POINT ( 'NONE',  ( -73.17575076540566670, -289.3471611511228616, -338.5295305579006140 ) ) ;
#13095 = CARTESIAN_POINT ( 'NONE',  ( -82.29815515474960819, -281.4155730172693097, -210.7079116666343452 ) ) ;
#13096 = CARTESIAN_POINT ( 'NONE',  ( -42.67935526091009990, -285.0419367525855705, -197.3079294672511139 ) ) ;
#13097 = CARTESIAN_POINT ( 'NONE',  ( -71.03151128435941075, -287.4966203679318255, -337.3685599341721399 ) ) ;
#13098 = CARTESIAN_POINT ( 'NONE',  ( -30.04969936926732288, -125.9919632799748683, -361.3284013991797110 ) ) ;
#13099 = CARTESIAN_POINT ( 'NONE',  ( 13.18663659086080031, -286.2891020732555489, -217.5193923262981457 ) ) ;
#13100 = CARTESIAN_POINT ( 'NONE',  ( 196.7647826491495096, 294.9769576964061457, -7.939513337131741011 ) ) ;
#13101 = CARTESIAN_POINT ( 'NONE',  ( -55.63446246692085850, -284.2232996921275685, -344.9144214526192513 ) ) ;
#13102 = CARTESIAN_POINT ( 'NONE',  ( -111.6971304372364813, -289.3707883968131114, -289.4948841157578272 ) ) ;
#13103 = CARTESIAN_POINT ( 'NONE',  ( -110.9634365019315823, -280.4015158755510697, -250.6566750267772932 ) ) ;
#13104 = ADVANCED_FACE ( 'NONE', ( #5712 ), #69163, .T. ) ;
#13105 = CARTESIAN_POINT ( 'NONE',  ( -105.7422402517998421, -280.3123565708022511, -235.9696995371090225 ) ) ;
#13106 = CARTESIAN_POINT ( 'NONE',  ( 34.56745690993932385, -281.2196164527435371, -257.7884039319196177 ) ) ;
#13107 = CARTESIAN_POINT ( 'NONE',  ( 25.45452036444216759, -276.9991902721627071, -229.3533706632188682 ) ) ;
#13108 = CARTESIAN_POINT ( 'NONE',  ( -64.26618685996827196, -295.3939646809603801, -342.5003723051854649 ) ) ;
#13109 = CARTESIAN_POINT ( 'NONE',  ( -111.9820258855963573, -288.5617055105353757, -271.1787795172390361 ) ) ;
#13110 = CARTESIAN_POINT ( 'NONE',  ( -75.83200796478132588, -294.4991503684483973, -332.8119906804576544 ) ) ;
#13111 = VERTEX_POINT ( 'NONE', #68703 ) ;
#13112 = ORIENTED_EDGE ( 'NONE', *, *, #34764, .F. ) ;
#13113 = CARTESIAN_POINT ( 'NONE',  ( -32.01880167513055397, -284.9046274631432993, -344.6105688262024955 ) ) ;
#13114 = CARTESIAN_POINT ( 'NONE',  ( -110.0709601562335109, -296.3120770961277799, -263.2933892711366752 ) ) ;
#13115 = CARTESIAN_POINT ( 'NONE',  ( 29.20058581790802421, -294.1344513205390285, -232.2347925612275787 ) ) ;
#13116 = CARTESIAN_POINT ( 'NONE',  ( -91.73535024486200484, -284.5053536241732104, -319.2187010217430725 ) ) ;
#13117 = CARTESIAN_POINT ( 'NONE',  ( 25.14237595999650310, -274.0181648292290788, -225.7453482768341644 ) ) ;
#13118 = CARTESIAN_POINT ( 'NONE',  ( -113.5662411612886302, -291.3356247030081363, -259.8155710765743152 ) ) ;
#13119 = CARTESIAN_POINT ( 'NONE',  ( -112.2623025429352595, -282.8394819047600777, -258.7371879021617929 ) ) ;
#13120 = CARTESIAN_POINT ( 'NONE',  ( -97.44971819883089381, -291.5297832156729214, -222.2698458504537484 ) ) ;
#13121 = CARTESIAN_POINT ( 'NONE',  ( 21.98134771310451896, -288.4804618505643248, -312.9388525589154710 ) ) ;
#13122 = DIRECTION ( 'NONE',  ( 0.000000000000000000, 0.000000000000000000, 1.000000000000000000 ) ) ;
#13123 = CYLINDRICAL_SURFACE ( 'NONE', #26653, 9.103929867429224387 ) ;
#13124 = CARTESIAN_POINT ( 'NONE',  ( -107.5458925959985947, -264.4132577019892665, -305.3929582931264122 ) ) ;
#13125 = CARTESIAN_POINT ( 'NONE',  ( -24.62984935714912282, -284.4130276570701312, -345.6551408998312240 ) ) ;
#13126 = CARTESIAN_POINT ( 'NONE',  ( -20.25526795762938548, -286.3380690714490697, -345.3683826091709648 ) ) ;
#13127 = ORIENTED_EDGE ( 'NONE', *, *, #73397, .F. ) ;
#13128 = CARTESIAN_POINT ( 'NONE',  ( -46.48142157134198982, -278.8539036382458107, -197.5726601185043307 ) ) ;
#13129 = CARTESIAN_POINT ( 'NONE',  ( -65.09141310736701769, -277.0715631795633840, -342.2205774995742900 ) ) ;
#13130 = CARTESIAN_POINT ( 'NONE',  ( -59.71956267270761032, -279.3428711032244678, -341.7702188895860900 ) ) ;
#13131 = CARTESIAN_POINT ( 'NONE',  ( 46.92461508910208323, 10.64641740143134641, -329.6966147455941609 ) ) ;
#13132 = CARTESIAN_POINT ( 'NONE',  ( 36.61688497611752524, -280.3690785119252382, -289.5635653221009420 ) ) ;
#13133 = CARTESIAN_POINT ( 'NONE',  ( -111.0411660237937923, -282.7260753879510276, -258.4382146118613832 ) ) ;
#13134 = CARTESIAN_POINT ( 'NONE',  ( -90.93689066507117502, -299.0640243673317400, -216.4952701389109961 ) ) ;
#13135 = CARTESIAN_POINT ( 'NONE',  ( 1.607939867105836473, -295.0087424573893031, -332.2345811614868012 ) ) ;
#13136 = ORIENTED_EDGE ( 'NONE', *, *, #66277, .T. ) ;
#13137 = CARTESIAN_POINT ( 'NONE',  ( -108.8340143552357944, -289.0137826064509454, -287.3932196156199552 ) ) ;
#13138 = CARTESIAN_POINT ( 'NONE',  ( 22.67358366012044613, -275.5584672508655331, -222.2624020364694672 ) ) ;
#13139 = CARTESIAN_POINT ( 'NONE',  ( -100.7177656438344826, -273.0497703128482385, -234.0313802245705119 ) ) ;
#13140 = ORIENTED_EDGE ( 'NONE', *, *, #60551, .T. ) ;
#13141 = DIRECTION ( 'NONE',  ( -0.000000000000000000, -1.000000000000000000, -0.000000000000000000 ) ) ;
#13142 = DIRECTION ( 'NONE',  ( 1.000000000000000000, 0.000000000000000000, 0.000000000000000000 ) ) ;
#13143 = DIRECTION ( 'NONE',  ( 0.000000000000000000, 1.000000000000000000, 0.000000000000000000 ) ) ;
#13144 = CARTESIAN_POINT ( 'NONE',  ( 36.01230307701023037, -282.6442167609558282, -271.3040711246267165 ) ) ;
#13145 = CARTESIAN_POINT ( 'NONE',  ( -61.74371412948401172, -281.4996016295623917, -198.3437147946767425 ) ) ;
#13146 = CARTESIAN_POINT ( 'NONE',  ( -45.67811780719655701, -282.2190079251647035, -343.1715554817286034 ) ) ;
#13147 = CARTESIAN_POINT ( 'NONE',  ( -13.94161494949410773, -282.2192806148665909, -199.8560781612178516 ) ) ;
#13148 = CARTESIAN_POINT ( 'NONE',  ( 24.55632538609000193, -274.5815952029155937, -310.4469483047266749 ) ) ;
#13149 = CARTESIAN_POINT ( 'NONE',  ( 154.7659666677267865, 20.47222690886501439, 12.53936336329526391 ) ) ;
#13150 = LINE ( 'NONE', #92183, #19924 ) ;
#13151 = CARTESIAN_POINT ( 'NONE',  ( -31.45241933482986596, -277.7825403288708230, -347.0261310258046592 ) ) ;
#13152 = ORIENTED_EDGE ( 'NONE', *, *, #26870, .F. ) ;
#13153 = VERTEX_POINT ( 'NONE', #3833 ) ;
#13154 = DIRECTION ( 'NONE',  ( 0.000000000000000000, 0.000000000000000000, 1.000000000000000000 ) ) ;
#13155 = CARTESIAN_POINT ( 'NONE',  ( -80.59635609174226545, -285.6149197981504244, -332.1290540324805534 ) ) ;
#13156 = CARTESIAN_POINT ( 'NONE',  ( 32.90235342443019562, -293.0198240527508915, -290.8603332812532472 ) ) ;
#13157 = CARTESIAN_POINT ( 'NONE',  ( 39.50202748138706710, -286.9516424454297976, -274.4258296723526769 ) ) ;
#13158 = CARTESIAN_POINT ( 'NONE',  ( -104.3941293239210069, -283.2108059009918861, -238.9036887440992700 ) ) ;
#13160 = CARTESIAN_POINT ( 'NONE',  ( -72.86463856696799724, -287.7694792911642026, -335.2925807679086461 ) ) ;
#13159 = CARTESIAN_POINT ( 'NONE',  ( -110.0836111539618827, -282.9768764429899761, -281.8236110394187790 ) ) ;
#13161 = CARTESIAN_POINT ( 'NONE',  ( 24.47309893579775775, -283.3028150041392905, -310.0280693981140416 ) ) ;
#13162 = CARTESIAN_POINT ( 'NONE',  ( 35.35315640183767982, -273.3149533290148270, -251.9096008031456790 ) ) ;
#13163 = CARTESIAN_POINT ( 'NONE',  ( 26.47897666945932471, -285.3993546640204499, -228.7274581860868068 ) ) ;
#13164 = CARTESIAN_POINT ( 'NONE',  ( -54.17178713204996399, -299.8361736930494885, -197.2738494807453264 ) ) ;
#13165 = CARTESIAN_POINT ( 'NONE',  ( -110.5678219994499614, -282.7694014896367776, -253.3916304481684278 ) ) ;
#13166 = CARTESIAN_POINT ( 'NONE',  ( -34.31556683640382488, -281.0323473273051604, -197.1757865294947862 ) ) ;
#13167 = CARTESIAN_POINT ( 'NONE',  ( 37.80659957834622986, -289.5310266043937304, -268.6993494226722987 ) ) ;
#13168 = DIRECTION ( 'NONE',  ( -0.000000000000000000, 1.000000000000000000, -0.000000000000000000 ) ) ;
#13169 = DIRECTION ( 'NONE',  ( -0.8457827187922973833, -0.5335274993777826547, 0.000000000000000000 ) ) ;
#13170 = CARTESIAN_POINT ( 'NONE',  ( -108.0806307988865598, -298.1282563709747819, -297.0664273263981272 ) ) ;
#13171 =( BOUNDED_CURVE ( )  B_SPLINE_CURVE ( 3, ( #45369, #1844, #31660, #81833 ),
 .UNSPECIFIED., .F., .F. ) 
 B_SPLINE_CURVE_WITH_KNOTS ( ( 4, 4 ),
 ( 3.665191429188093597, 4.712388980384689674 ),
 .UNSPECIFIED. ) 
 CURVE ( )  GEOMETRIC_REPRESENTATION_ITEM ( )  RATIONAL_B_SPLINE_CURVE ( ( 1.000000000000000000, 0.9106836025229593234, 0.9106836025229593234, 1.000000000000000000 ) ) 
 REPRESENTATION_ITEM ( '' )  );
#13172 = CARTESIAN_POINT ( 'NONE',  ( -98.53179750385400837, -275.9623592474047200, -313.7513081070798080 ) ) ;
#13173 = CARTESIAN_POINT ( 'NONE',  ( -110.2743876131848424, -290.0562869382329154, -246.0082799058550904 ) ) ;
#13174 = CARTESIAN_POINT ( 'NONE',  ( -20.68723561645209230, -293.2347711971108311, -342.3100293269384906 ) ) ;
#13175 = CARTESIAN_POINT ( 'NONE',  ( -59.86897441637935202, -278.4390357109370484, -200.3520043454716131 ) ) ;
#13176 = CARTESIAN_POINT ( 'NONE',  ( 97.23951108435230140, -297.8936950320585311, -196.1691743667933281 ) ) ;
#13177 = CARTESIAN_POINT ( 'NONE',  ( 19.71814889672734949, -294.2161614112207531, -224.0225727172560539 ) ) ;
#13178 = CARTESIAN_POINT ( 'NONE',  ( -95.99890600148557951, -287.6948066931273615, -223.6242672951989618 ) ) ;
#13179 = CARTESIAN_POINT ( 'NONE',  ( -110.5556815663805565, -294.7593249774552078, -291.9112155208854915 ) ) ;
#13180 = CARTESIAN_POINT ( 'NONE',  ( 12.71320640249439649, -289.9405463420261526, -324.6610746390530267 ) ) ;
#13182 = CARTESIAN_POINT ( 'NONE',  ( 5.937709055172086359, -290.8701842108746405, -207.9041988101028835 ) ) ;
#13181 =( BOUNDED_SURFACE ( )  B_SPLINE_SURFACE ( 3, 2, ( 
 ( #35975, #51102, #92317 ),
 ( #6169, #71986, #6642 ),
 ( #85227, #58239, #7104 ),
 ( #86149, #71509, #27471 ),
 ( #14682, #21300, #50172 ),
 ( #78602, #20508, #28876 ) ),
 .UNSPECIFIED., .F., .F., .F. ) 
 B_SPLINE_SURFACE_WITH_KNOTS ( ( 4, 2, 4 ),
 ( 3, 3 ),
 ( 5.756444938927698374, 6.019815123053642303, 6.283185307179586232 ),
 ( 0.000000000000000000, 1.000000000000000000 ),
 .UNSPECIFIED. ) 
 GEOMETRIC_REPRESENTATION_ITEM ( )  RATIONAL_B_SPLINE_SURFACE ( (
 ( 1.000000000000000000, 0.9186651033962678348, 1.000000000000000000),
 ( 1.000000000000000000, 0.9282241625911032967, 1.000000000000000000),
 ( 1.000000000000000000, 0.9354614375524443748, 1.000000000000000000),
 ( 1.000000000000000000, 0.9451322790882570324, 1.000000000000000000),
 ( 1.000000000000000000, 0.9475641245298920268, 1.000000000000000000),
 ( 1.000000000000000000, 0.9475641245298920268, 1.000000000000000000) ) ) 
 REPRESENTATION_ITEM ( '' )  SURFACE ( )  );
#13183 = CARTESIAN_POINT ( 'NONE',  ( -85.05336978111068902, -291.1507612481433398, -326.4548881838513239 ) ) ;
#13184 = DIRECTION ( 'NONE',  ( 1.000000000000000000, -0.000000000000000000, 0.000000000000000000 ) ) ;
#13185 = CARTESIAN_POINT ( 'NONE',  ( -110.1345733825187096, -291.4515337883765369, -263.0263153193224070 ) ) ;
#13186 = DIRECTION ( 'NONE',  ( -0.2456588035076305854, 0.9693563597868429804, 0.000000000000000000 ) ) ;
#13187 = CARTESIAN_POINT ( 'NONE',  ( -103.4479646406618514, -291.2496717990660500, -309.1696249320678476 ) ) ;
#13189 = CARTESIAN_POINT ( 'NONE',  ( 33.64776568011784263, -293.3270417843093583, -253.2931411323557995 ) ) ;
#13188 = CARTESIAN_POINT ( 'NONE',  ( 32.80281012903238747, -279.2139513374593207, -242.6839718336630654 ) ) ;
#13190 = CARTESIAN_POINT ( 'NONE',  ( 37.33125482342504142, -281.3170909118201166, -251.5741597718676417 ) ) ;
#13191 = CARTESIAN_POINT ( 'NONE',  ( 37.31178805815597599, -280.9838636417387079, -251.5834452499970268 ) ) ;
#13192 = CARTESIAN_POINT ( 'NONE',  ( -37.29173687890931888, -287.0513678794694670, -345.1944390038898973 ) ) ;
#13193 = CARTESIAN_POINT ( 'NONE',  ( -6.766014609581612937, -280.7860669639875368, -338.0211470727738856 ) ) ;
#13194 = CARTESIAN_POINT ( 'NONE',  ( -100.8120201606800634, -283.0891964045927125, -230.4046526402919426 ) ) ;
#13195 = CARTESIAN_POINT ( 'NONE',  ( -14.41743743185335980, -278.8238259178663725, -197.5239472378277696 ) ) ;
#13196 = CARTESIAN_POINT ( 'NONE',  ( -60.40381468904433859, -284.6803934060176857, -197.1645944589982093 ) ) ;
#13197 = CARTESIAN_POINT ( 'NONE',  ( 22.40680990774804116, -275.7666686549721362, -228.1171986848795257 ) ) ;
#13198 = CARTESIAN_POINT ( 'NONE',  ( 195.9379236003509845, 41.56271157415176987, 14.00773366423596045 ) ) ;
#13199 = CARTESIAN_POINT ( 'NONE',  ( 28.18763796841624369, -294.6956310842564903, -236.4148919517652985 ) ) ;
#13200 = CARTESIAN_POINT ( 'NONE',  ( -7.934260883709791656, -275.8550925137372474, -199.7797254809386231 ) ) ;
#13201 = CARTESIAN_POINT ( 'NONE',  ( -90.98626821953766353, -277.5068799541975295, -319.9760468343509388 ) ) ;
#13202 = CARTESIAN_POINT ( 'NONE',  ( -70.89963077793883883, -291.7882434108544203, -201.0584102790545558 ) ) ;
#13203 = CARTESIAN_POINT ( 'NONE',  ( -4.806455117229143426, -280.7069051779081406, -338.5719025573442309 ) ) ;
#13204 = ADVANCED_FACE ( 'NONE', ( #32715 ), #70168, .F. ) ;
#13205 = CARTESIAN_POINT ( 'NONE',  ( -110.5724608677903262, -289.6001785506539932, -271.1760589972295747 ) ) ;
#13206 = CARTESIAN_POINT ( 'NONE',  ( -85.14078402382351385, -293.7120025835242814, -328.1559985897099523 ) ) ;
#13207 = ORIENTED_EDGE ( 'NONE', *, *, #80212, .F. ) ;
#13208 = CARTESIAN_POINT ( 'NONE',  ( 152.9200301536615427, 20.54241773159251494, 11.30461213544953480 ) ) ;
#13209 = CARTESIAN_POINT ( 'NONE',  ( 23.39588687650400800, -292.4963591593925116, -229.7540500443035398 ) ) ;
#13210 = CARTESIAN_POINT ( 'NONE',  ( 208.1134247887914057, 29.32324166632049156, 13.52119360038336460 ) ) ;
#13211 = CARTESIAN_POINT ( 'NONE',  ( -105.5795714935544112, -270.2666405000204009, -254.7536222014695397 ) ) ;
#13212 = CARTESIAN_POINT ( 'NONE',  ( -102.1114193182946650, -296.1526308626056903, -229.1579180011978565 ) ) ;
#13213 = CARTESIAN_POINT ( 'NONE',  ( 36.34147294759234370, -279.9165812688573283, -288.0542821122240866 ) ) ;
#13214 = CARTESIAN_POINT ( 'NONE',  ( -91.56535843695301935, -286.6144295479914490, -216.3880399548188223 ) ) ;
#13215 = CARTESIAN_POINT ( 'NONE',  ( 6.928609633152132297, -286.5069850563670002, -212.2529581264224419 ) ) ;
#13216 = CARTESIAN_POINT ( 'NONE',  ( 34.84761650350014150, -277.2658398318063746, -285.1736234600069793 ) ) ;
#13217 = CARTESIAN_POINT ( 'NONE',  ( -102.6415336746871674, -295.0556475122322695, -234.1978971791031370 ) ) ;
#13218 = CARTESIAN_POINT ( 'NONE',  ( -108.5720322254002923, -298.0501579400387300, -290.4661870977500939 ) ) ;
#13219 = CARTESIAN_POINT ( 'NONE',  ( 15.87527022550933431, -275.0718221360676807, -320.9089623607256954 ) ) ;
#13220 = ORIENTED_EDGE ( 'NONE', *, *, #4023, .F. ) ;
#13221 = CARTESIAN_POINT ( 'NONE',  ( 195.6548686469884331, 40.46313866827317440, 13.67209655823288550 ) ) ;
#13222 = CARTESIAN_POINT ( 'NONE',  ( -113.5802273811413272, -296.3532992165808082, -259.6153921970017109 ) ) ;
#13223 = CARTESIAN_POINT ( 'NONE',  ( 36.70431915697744074, -289.3733650648983371, -262.7125086578888045 ) ) ;
#13224 = LINE ( 'NONE', #63892, #8263 ) ;
#13225 = ADVANCED_FACE ( 'NONE', ( #56859 ), #58251, .F. ) ;
#13226 = CARTESIAN_POINT ( 'NONE',  ( 35.22640332184441547, -288.3197350429695121, -279.1794528485765454 ) ) ;
#13227 = VERTEX_POINT ( 'NONE', #7562 ) ;
#13228 = CARTESIAN_POINT ( 'NONE',  ( -72.38866415002550525, -278.6586142101342602, -202.0491439790257857 ) ) ;
#13229 = CARTESIAN_POINT ( 'NONE',  ( -84.11661706964751772, -296.3272961550989635, -331.4644670987712516 ) ) ;
#13230 = CARTESIAN_POINT ( 'NONE',  ( -112.5897301300584985, -288.5739364756557848, -279.6292772476776349 ) ) ;
#13231 = CARTESIAN_POINT ( 'NONE',  ( -105.9369329510236213, -296.4341113216348731, -305.4132990448233613 ) ) ;
#13232 = CARTESIAN_POINT ( 'NONE',  ( 18.85208633331983563, -294.5465951587702875, -316.9909994963678059 ) ) ;
#13233 = CARTESIAN_POINT ( 'NONE',  ( 175.2296996224750103, 161.0000000000000853, -9.550761578869391144 ) ) ;
#13234 = CARTESIAN_POINT ( 'NONE',  ( 157.7374095173865385, 14.19731191252289015, 13.00000000000000178 ) ) ;
#13235 = CARTESIAN_POINT ( 'NONE',  ( -69.05136874130262470, -290.9817495608907052, -339.7814949663526249 ) ) ;
#13236 = CARTESIAN_POINT ( 'NONE',  ( 13.79469577742117714, -277.1948066931273047, -206.1857440867352693 ) ) ;
#13237 = CARTESIAN_POINT ( 'NONE',  ( 26.63247633025644845, -281.4631305591855153, -313.0298129828989318 ) ) ;
#13238 = CARTESIAN_POINT ( 'NONE',  ( 8.947493384365307278, -284.4160441842945488, -329.2264556882181523 ) ) ;
#13239 = CARTESIAN_POINT ( 'NONE',  ( 0.01172085390532574128, -285.1138947430600297, -203.6878892655028892 ) ) ;
#13240 = CARTESIAN_POINT ( 'NONE',  ( -100.9292277647859919, -289.1547526071266816, -231.6578813548579490 ) ) ;
#13241 = CARTESIAN_POINT ( 'NONE',  ( 36.08224369344183913, -277.1749053330518677, -251.6734226417129321 ) ) ;
#13242 = ORIENTED_EDGE ( 'NONE', *, *, #45431, .F. ) ;
#13244 = CARTESIAN_POINT ( 'NONE',  ( 26.55194987874112300, -280.4158114208411234, -234.8435989714105006 ) ) ;
#13243 = CARTESIAN_POINT ( 'NONE',  ( -106.4447276250628249, -278.8667357064120438, -246.6735348530797296 ) ) ;
#13245 = CARTESIAN_POINT ( 'NONE',  ( 20.59579138533102949, -277.3137119525053436, -320.6277849164667941 ) ) ;
#13246 = CARTESIAN_POINT ( 'NONE',  ( -64.58667833182528284, -278.4993097295289886, -198.7110506695674701 ) ) ;
#13247 = CARTESIAN_POINT ( 'NONE',  ( 177.9591486883064704, 253.1359646847975569, -165.0577554255288817 ) ) ;
#13248 = CARTESIAN_POINT ( 'NONE',  ( -21.41534048864555473, -275.1928476423493635, -195.2667022053635151 ) ) ;
#13249 = ITEM_DEFINED_TRANSFORMATION ( 'NONE', 'NONE', #49155,  #18940 ) ;
#13250 = CARTESIAN_POINT ( 'NONE',  ( -107.4482365777889896, -274.4610668013719419, -240.0980019203336724 ) ) ;
#13251 = CARTESIAN_POINT ( 'NONE',  ( -69.91165696735023971, -288.1233781216987495, -202.8022627189028810 ) ) ;
#13252 = CARTESIAN_POINT ( 'NONE',  ( 82.61807361380685677, -301.9754278600166799, -194.6565851556404141 ) ) ;
#13253 = CARTESIAN_POINT ( 'NONE',  ( 34.59012354649429710, -288.8184694851551626, -284.5695791274170006 ) ) ;
#13254 = CARTESIAN_POINT ( 'NONE',  ( -104.5464866480762538, -286.7775138937134329, -234.7872787116800453 ) ) ;
#13255 = CARTESIAN_POINT ( 'NONE',  ( 16.07979082962989636, -287.6181351154477284, -320.3354455872358244 ) ) ;
#13256 = CARTESIAN_POINT ( 'NONE',  ( -100.9420828770734602, -284.6322877313541539, -226.9713096542522237 ) ) ;
#13257 = CARTESIAN_POINT ( 'NONE',  ( -1.560555935284581475, -278.9347858037416472, -205.8153966966281132 ) ) ;
#13258 = CARTESIAN_POINT ( 'NONE',  ( -16.85332721199014117, -288.1798577463021616, -198.9554921802975969 ) ) ;
#13259 = CARTESIAN_POINT ( 'NONE',  ( 31.72684376296890818, -279.6908102532306657, -244.5194006846924424 ) ) ;
#13260 = CARTESIAN_POINT ( 'NONE',  ( -93.08985695592467380, -279.1900557387588151, -318.2504329638941272 ) ) ;
#13261 = CARTESIAN_POINT ( 'NONE',  ( 29.13944126306517646, -275.6348210317758571, -239.9361765859873685 ) ) ;
#13262 = CARTESIAN_POINT ( 'NONE',  ( 32.49654814952607751, -286.7512063388230104, -301.8353581640465109 ) ) ;
#13263 = CARTESIAN_POINT ( 'NONE',  ( -1.699944976556255982, -283.3948059126345811, -338.4333157630394453 ) ) ;
#13264 = CARTESIAN_POINT ( 'NONE',  ( -110.6250167409816783, -284.7491674640791075, -293.8370608886457376 ) ) ;
#13265 = CARTESIAN_POINT ( 'NONE',  ( 28.15200699728796252, -282.1571155903004069, -302.7182719269644053 ) ) ;
#13266 = EDGE_LOOP ( 'NONE', ( #83894, #50637, #46520, #79412 ) ) ;
#13267 = ORIENTED_EDGE ( 'NONE', *, *, #18976, .F. ) ;
#13268 = DIRECTION ( 'NONE',  ( -0.000000000000000000, -1.000000000000000000, -0.000000000000000000 ) ) ;
#13269 = CARTESIAN_POINT ( 'NONE',  ( -79.82804075928844156, -291.4799941684432270, -333.1557867698357427 ) ) ;
#13270 = CARTESIAN_POINT ( 'NONE',  ( -6.073065037973113256, -291.1393682624394614, -200.5216321678052509 ) ) ;
#13271 = CARTESIAN_POINT ( 'NONE',  ( 9.067659185125956256, -297.8449062927535920, -197.2061706911376859 ) ) ;
#13272 = CARTESIAN_POINT ( 'NONE',  ( 24.79900619645963644, -293.5030016537069741, -315.6805956289199457 ) ) ;
#13273 = CARTESIAN_POINT ( 'NONE',  ( -61.50040692830693700, -287.8516458893056438, -339.9819815044450024 ) ) ;
#13274 = CARTESIAN_POINT ( 'NONE',  ( 17.50396740551644825, -291.0890028363598390, -220.5875647013370724 ) ) ;
#13275 = CARTESIAN_POINT ( 'NONE',  ( -110.7339212150326375, -291.7461608775428772, -271.2051485149819428 ) ) ;
#13276 = CARTESIAN_POINT ( 'NONE',  ( 208.4306832106270804, -147.7221692137691775, -8.500000000000007105 ) ) ;
#13277 = CARTESIAN_POINT ( 'NONE',  ( -69.75114221688832572, -291.4789367044171513, -338.0112273654578985 ) ) ;
#13278 = CARTESIAN_POINT ( 'NONE',  ( -83.12893142027415649, -289.4271986122948874, -210.6838080538360032 ) ) ;
#13279 = CARTESIAN_POINT ( 'NONE',  ( -15.43824080252674413, -294.3356916071157912, -198.5771203424665146 ) ) ;
#13280 = CARTESIAN_POINT ( 'NONE',  ( -60.06297201360979443, -286.6915577389756322, -200.7396252404172685 ) ) ;
#13281 = CARTESIAN_POINT ( 'NONE',  ( 16.16620465187848765, -294.8088544805097513, -217.4964467051408974 ) ) ;
#13282 = CARTESIAN_POINT ( 'NONE',  ( 222.8344101925596306, -44.55766379199612004, 21.50000000000000000 ) ) ;
#13283 = DIRECTION ( 'NONE',  ( 0.000000000000000000, -0.000000000000000000, 1.000000000000000000 ) ) ;
#13284 = CARTESIAN_POINT ( 'NONE',  ( -34.19760693703548782, -276.0714005109367690, -195.0715338223843389 ) ) ;
#13285 = CARTESIAN_POINT ( 'NONE',  ( -79.39714900560086619, -294.8017554348708131, -334.6689560731301754 ) ) ;
#13286 = CARTESIAN_POINT ( 'NONE',  ( -40.80016292372313558, -272.2480494399781605, -196.3782366482245152 ) ) ;
#13287 = CARTESIAN_POINT ( 'NONE',  ( -93.83512398945097743, -275.9552506792462623, -318.8359285611423388 ) ) ;
#13288 = CARTESIAN_POINT ( 'NONE',  ( -35.81942213812178721, -299.3867755882932897, -196.8676142273301650 ) ) ;
#13289 = CARTESIAN_POINT ( 'NONE',  ( 32.02582921031893193, -273.7123508140779222, -238.1920797287320397 ) ) ;
#13290 = CARTESIAN_POINT ( 'NONE',  ( -72.38934847890529056, -296.9507956390861523, -335.0828205206771031 ) ) ;
#13291 = LINE ( 'NONE', #28426, #41404 ) ;
#13292 = CARTESIAN_POINT ( 'NONE',  ( -109.9634803927136346, -297.2329020091125926, -279.6364362873392793 ) ) ;
#13293 = DIRECTION ( 'NONE',  ( -5.501794166262391869E-14, -0.01273136352371387336, 0.9999189529070978688 ) ) ;
#13295 = CARTESIAN_POINT ( 'NONE',  ( -71.90585480228867254, -273.4154427323843493, -206.0061226401631131 ) ) ;
#13294 = CARTESIAN_POINT ( 'NONE',  ( 29.96425324400670931, -285.1267148682284756, -236.4743146447557933 ) ) ;
#13296 = CARTESIAN_POINT ( 'NONE',  ( -23.78590587996978911, -286.2206314835377725, -194.5095368467766264 ) ) ;
#13297 = CARTESIAN_POINT ( 'NONE',  ( -96.37757304929139934, -289.5536556097736707, -319.7830831870003863 ) ) ;
#13298 = CARTESIAN_POINT ( 'NONE',  ( -108.7782547143636265, -298.2234260206692511, -294.3449765333902519 ) ) ;
#13299 = CARTESIAN_POINT ( 'NONE',  ( 2.525515051747646122, -292.5166364658471139, -333.7520399652273113 ) ) ;
#13300 = CARTESIAN_POINT ( 'NONE',  ( -36.74352194544972150, -279.2566630304733621, -193.5119037040155945 ) ) ;
#13301 = CARTESIAN_POINT ( 'NONE',  ( -110.4542110544635705, -282.2666405000204009, -253.6410175316879361 ) ) ;
#13302 = DIRECTION ( 'NONE',  ( 0.000000000000000000, 0.000000000000000000, -1.000000000000000000 ) ) ;
#13303 = CARTESIAN_POINT ( 'NONE',  ( -96.09535074574621660, -288.7327123666485136, -314.3723131753113762 ) ) ;
#13304 = LINE ( 'NONE', #27023, #54729 ) ;
#13305 = CARTESIAN_POINT ( 'NONE',  ( -48.37982755296233250, -287.1923466009893673, -344.5968286482300300 ) ) ;
#13306 = CARTESIAN_POINT ( 'NONE',  ( -34.46092253694913410, -299.6889310377678726, -196.5603117501235033 ) ) ;
#13307 = CARTESIAN_POINT ( 'NONE',  ( -14.42192968462125613, -281.7687458506202915, -197.4133293322394707 ) ) ;
#13309 = CARTESIAN_POINT ( 'NONE',  ( 33.65014977728414181, -281.7771729484286425, -287.4189228401804144 ) ) ;
#13308 = CARTESIAN_POINT ( 'NONE',  ( -98.68457016061034892, -293.9788964776909097, -314.2150028641716517 ) ) ;
#13310 = CARTESIAN_POINT ( 'NONE',  ( -114.3661541337180125, -296.6924334952742583, -272.4719108930375455 ) ) ;
#13311 = CARTESIAN_POINT ( 'NONE',  ( -110.9316044294118910, -274.0131273331129478, -267.6333776901211650 ) ) ;
#13312 = CARTESIAN_POINT ( 'NONE',  ( 36.28629328887802785, -283.3689571366431323, -256.0810886769661465 ) ) ;
#13313 = ADVANCED_FACE ( 'NONE', ( #92325 ), #471, .T. ) ;
#13314 = CARTESIAN_POINT ( 'NONE',  ( -102.9843626886730021, -295.1707710223560071, -302.9480397092364683 ) ) ;
#13315 = DIRECTION ( 'NONE',  ( -0.000000000000000000, 1.000000000000000000, -0.000000000000000000 ) ) ;
#13316 = CARTESIAN_POINT ( 'NONE',  ( -40.27429429716867304, -285.0690948919350376, -344.9482931299669417 ) ) ;
#13317 = DIRECTION ( 'NONE',  ( -0.000000000000000000, -0.000000000000000000, 1.000000000000000000 ) ) ;
#13318 = CARTESIAN_POINT ( 'NONE',  ( 39.58706461736021254, -291.0523547857346784, -270.3937649182068981 ) ) ;
#13319 = CARTESIAN_POINT ( 'NONE',  ( 12.59191402391305914, -275.5735453205755903, -328.7631127921176812 ) ) ;
#13320 = CARTESIAN_POINT ( 'NONE',  ( 34.71428584965417485, -293.2300723150740396, -258.5810196915511483 ) ) ;
#13321 = CARTESIAN_POINT ( 'NONE',  ( 32.89800957462700381, -283.3670599640123555, -292.8229907658758293 ) ) ;
#13322 = CARTESIAN_POINT ( 'NONE',  ( 20.66376293287339649, -277.7890978393866135, -316.0082958466583136 ) ) ;
#13323 = CARTESIAN_POINT ( 'NONE',  ( -58.30751316631194925, -284.7430964692247244, -343.8943545077620456 ) ) ;
#13324 = CARTESIAN_POINT ( 'NONE',  ( -48.40358893006416707, -281.9910141141397730, -342.9198191846614350 ) ) ;
#13325 = CARTESIAN_POINT ( 'NONE',  ( -100.8556012367507719, -280.0150311124909877, -310.3452307262088539 ) ) ;
#13326 = CARTESIAN_POINT ( 'NONE',  ( -113.5446204578502289, -272.8615831427289891, -258.9468195243208584 ) ) ;
#13327 = CARTESIAN_POINT ( 'NONE',  ( 38.72794106646267664, -275.2351641450217130, -258.3425603676383275 ) ) ;
#13328 = CARTESIAN_POINT ( 'NONE',  ( 35.74272605931487590, -295.6552476390149309, -284.5025765085347302 ) ) ;
#13329 = DIRECTION ( 'NONE',  ( 0.000000000000000000, 0.000000000000000000, 1.000000000000000000 ) ) ;
#13330 = EDGE_CURVE ( 'NONE', #72522, #69300, #80001, .T. ) ;
#13331 = EDGE_CURVE ( 'NONE', #3498, #55409, #13291, .T. ) ;
#13332 = CARTESIAN_POINT ( 'NONE',  ( -91.82548206730525919, -293.9587943249416071, -323.0092232242637920 ) ) ;
#13333 = VECTOR ( 'NONE', #26325, 1000.000000000000000 ) ;
#13334 = CARTESIAN_POINT ( 'NONE',  ( 35.76030458812795843, -275.0760287836251905, -271.5922547362052910 ) ) ;
#13335 = CARTESIAN_POINT ( 'NONE',  ( -34.85764802893503145, -296.5415923271413590, -346.6273440562115411 ) ) ;
#13336 = CARTESIAN_POINT ( 'NONE',  ( 38.42607710878368721, -294.8990354538168503, -281.6417496667460796 ) ) ;
#13337 = CARTESIAN_POINT ( 'NONE',  ( -61.83153189358446156, -291.3713609529248743, -341.0737516871702155 ) ) ;
#13338 = CARTESIAN_POINT ( 'NONE',  ( -71.30711949780425130, -275.5015684789742068, -337.0422901157353976 ) ) ;
#13339 = CARTESIAN_POINT ( 'NONE',  ( -105.5818647435220470, -280.0786088314952167, -300.2323094017955327 ) ) ;
#13340 = CARTESIAN_POINT ( 'NONE',  ( -108.2482811207109279, -294.3353342821780529, -293.1902690051132367 ) ) ;
#13341 = CARTESIAN_POINT ( 'NONE',  ( 38.40471398893728860, -283.3709508381015212, -267.0867437688525570 ) ) ;
#13342 = CARTESIAN_POINT ( 'NONE',  ( -109.4948291701508367, -283.6437434264569788, -257.3232252405673535 ) ) ;
#13343 = CARTESIAN_POINT ( 'NONE',  ( 175.7829685710282490, 241.4225270720233993, -178.8902070973051650 ) ) ;
#13344 = ORIENTED_EDGE ( 'NONE', *, *, #32210, .F. ) ;
#13345 = CARTESIAN_POINT ( 'NONE',  ( -101.0076760093505186, -284.7092620005935828, -234.4981560243688818 ) ) ;
#13346 = VERTEX_POINT ( 'NONE', #79080 ) ;
#13347 = CARTESIAN_POINT ( 'NONE',  ( 38.48696822839085740, -282.4835041891510059, -258.5495064154487750 ) ) ;
#13348 = CARTESIAN_POINT ( 'NONE',  ( -112.7488796467082466, -283.1739298605095314, -284.1347429643098508 ) ) ;
#13349 = CARTESIAN_POINT ( 'NONE',  ( -98.39652796683617453, -280.1158059992869767, -223.8087629838302632 ) ) ;
#13350 =( NAMED_UNIT ( * ) PLANE_ANGLE_UNIT ( ) SI_UNIT ( $, .RADIAN. ) );
#13351 = CARTESIAN_POINT ( 'NONE',  ( -73.74885610911908884, -279.0465600014897518, -337.4373486444525270 ) ) ;
#13352 = CARTESIAN_POINT ( 'NONE',  ( -42.43160071744534889, -280.6409504488445350, -193.6316862197214732 ) ) ;
#13353 = CARTESIAN_POINT ( 'NONE',  ( -107.3381139276884824, -270.1608578419545665, -262.4421837807431075 ) ) ;
#13354 = CARTESIAN_POINT ( 'NONE',  ( 104.3268223557888632, 115.7811322214007106, -282.9140813606151710 ) ) ;
#13355 = ORIENTED_EDGE ( 'NONE', *, *, #8701, .T. ) ;
#13356 = CARTESIAN_POINT ( 'NONE',  ( -4.526546245600342466, -276.4856637597059148, -203.0922537475019283 ) ) ;
#13357 = CARTESIAN_POINT ( 'NONE',  ( 196.8892120694305561, 285.3822140004605217, -111.7264957686566760 ) ) ;
#13358 = CARTESIAN_POINT ( 'NONE',  ( -24.57073831618998483, -278.2360412430826386, -196.8169181132106473 ) ) ;
#13359 = CARTESIAN_POINT ( 'NONE',  ( 12.59545223515086043, -294.4973898731731197, -213.0876090509810581 ) ) ;
#13360 = CARTESIAN_POINT ( 'NONE',  ( 31.90025972733708670, -292.5878521765746996, -246.7632736836748109 ) ) ;
#13361 = CARTESIAN_POINT ( 'NONE',  ( -48.86597568641041534, -288.7026992182203458, -346.4855001391566702 ) ) ;
#13362 = FACE_OUTER_BOUND ( 'NONE', #92185, .T. ) ;
#13364 = CARTESIAN_POINT ( 'NONE',  ( -101.6788648948478624, -283.4426187345664516, -234.1016384298702633 ) ) ;
#13363 = CARTESIAN_POINT ( 'NONE',  ( 34.92318372090718981, -292.4440451094114906, -295.3504073259857705 ) ) ;
#13365 = CARTESIAN_POINT ( 'NONE',  ( -49.92095674834108365, -293.7505379155027185, -197.1472666823371469 ) ) ;
#13366 = CARTESIAN_POINT ( 'NONE',  ( -10.47937405178511838, -284.8889527304158378, -201.7244105465882740 ) ) ;
#13367 = CARTESIAN_POINT ( 'NONE',  ( -10.78202387840521936, -284.0137163142777013, -338.9411714401007316 ) ) ;
#13368 = VERTEX_POINT ( 'NONE', #28886 ) ;
#13369 = CARTESIAN_POINT ( 'NONE',  ( -96.40553567100263876, -292.1549274917594516, -221.3073061160637849 ) ) ;
#13370 = CARTESIAN_POINT ( 'NONE',  ( -24.04815227689346813, -283.3701023588765793, -342.2030975419046399 ) ) ;
#13371 = CARTESIAN_POINT ( 'NONE',  ( 4.000022826579053614, -293.3038497304150951, -334.9128697508077721 ) ) ;
#13372 = CARTESIAN_POINT ( 'NONE',  ( 33.89647625926698993, -288.7229474330244443, -299.3001277534231122 ) ) ;
#13373 = CARTESIAN_POINT ( 'NONE',  ( -89.44519963789684880, -290.2554453254734881, -326.9716491752652132 ) ) ;
#13374 = CARTESIAN_POINT ( 'NONE',  ( 20.33934892975745257, -287.0886295873547169, -225.6185590020763527 ) ) ;
#13375 = EDGE_LOOP ( 'NONE', ( #39374, #53160, #70901, #40643, #54433, #65990 ) ) ;
#13376 = CARTESIAN_POINT ( 'NONE',  ( -109.1670816552720140, -298.1039690335233558, -294.4737712642309475 ) ) ;
#13377 = CARTESIAN_POINT ( 'NONE',  ( -35.46997145530772855, -296.7599569347117949, -193.8546733024735431 ) ) ;
#13378 = CARTESIAN_POINT ( 'NONE',  ( -94.11536208669448911, -278.2636532426420217, -224.0992572687231075 ) ) ;
#13379 = CARTESIAN_POINT ( 'NONE',  ( -104.1729650447399820, -272.5565160551118424, -232.1345486481228590 ) ) ;
#13380 = CARTESIAN_POINT ( 'NONE',  ( -102.0855929066622423, -294.5561278674812797, -305.5596420800655437 ) ) ;
#13381 = CARTESIAN_POINT ( 'NONE',  ( 36.11462389192714539, -277.4355523422403849, -279.8341022204190836 ) ) ;
#13382 = CARTESIAN_POINT ( 'NONE',  ( -41.90878636754561626, -296.2336660129101915, -196.4888245454744151 ) ) ;
#13383 = CARTESIAN_POINT ( 'NONE',  ( -69.88640781717172956, -296.6957617585835010, -336.1484458471023800 ) ) ;
#13384 = CARTESIAN_POINT ( 'NONE',  ( -86.68794316496197894, -296.8374569706748503, -324.5752708490456371 ) ) ;
#13385 = DIRECTION ( 'NONE',  ( -0.000000000000000000, -0.000000000000000000, -1.000000000000000000 ) ) ;
#13386 = CARTESIAN_POINT ( 'NONE',  ( -39.06906525273071651, -296.6736123252691186, -346.5415395318700007 ) ) ;
#13387 = CARTESIAN_POINT ( 'NONE',  ( -109.8467046344627818, -294.8085908945579945, -250.3434754030240299 ) ) ;
#13388 = CARTESIAN_POINT ( 'NONE',  ( -1.213505996069036197, -293.1964363068412354, -206.7962790582370474 ) ) ;
#13389 = CARTESIAN_POINT ( 'NONE',  ( -109.0196755427803907, -273.7080437808004945, -242.5301953407418978 ) ) ;
#13390 = CARTESIAN_POINT ( 'NONE',  ( -89.08819371414298871, -288.3722507930980896, -322.6839172010979269 ) ) ;
#13391 = CARTESIAN_POINT ( 'NONE',  ( -80.01335438358211150, -275.4753622634503358, -208.6203852425925618 ) ) ;
#13392 = CARTESIAN_POINT ( 'NONE',  ( -38.36288823930932779, -274.5320166602838867, -193.4294334932374397 ) ) ;
#13393 = CARTESIAN_POINT ( 'NONE',  ( -108.8007042618494182, -297.0843360651410308, -255.2777241437379416 ) ) ;
#13394 = CARTESIAN_POINT ( 'NONE',  ( 31.65657358356577333, -283.1372703942421367, -240.0684616986798403 ) ) ;
#13395 = CARTESIAN_POINT ( 'NONE',  ( -14.35983336860481430, -279.0287408646465224, -197.3320692362628392 ) ) ;
#13396 = CARTESIAN_POINT ( 'NONE',  ( -27.39351775990539295, -282.2776311530182056, -346.6662700881418004 ) ) ;
#13397 = CARTESIAN_POINT ( 'NONE',  ( 39.52113530922233764, -274.9469028837197015, -274.0473619053024095 ) ) ;
#13398 = CARTESIAN_POINT ( 'NONE',  ( 25.63110975818091219, -279.3791782628262013, -227.3637065693968964 ) ) ;
#13399 = CARTESIAN_POINT ( 'NONE',  ( -89.76095616019094336, -277.3149834530008206, -216.4160454584225306 ) ) ;
#13400 = ADVANCED_FACE ( 'NONE', ( #93273 ), #78612, .F. ) ;
#13401 = CARTESIAN_POINT ( 'NONE',  ( -40.78448521491121426, -272.5828642711813359, -196.8023618114719113 ) ) ;
#13402 = CARTESIAN_POINT ( 'NONE',  ( 1.685545664834484203, -278.5308743098423179, -334.4663451851374703 ) ) ;
#13403 = CARTESIAN_POINT ( 'NONE',  ( -56.02477538461528184, -229.5268262511776527, 22.50000000000000000 ) ) ;
#13404 = AXIS2_PLACEMENT_3D ( 'NONE', #51337, #29113, #14463 ) ;
#13405 = CARTESIAN_POINT ( 'NONE',  ( 153.6987871352711181, 19.48326534539918597, 11.45812909362558152 ) ) ;
#13406 = CARTESIAN_POINT ( 'NONE',  ( -99.08491283637989966, -295.3868079081368023, -226.0694743079803004 ) ) ;
#13407 = CARTESIAN_POINT ( 'NONE',  ( -2.787112871733855801, -290.5266824355647373, -203.3810858706880822 ) ) ;
#13408 = CARTESIAN_POINT ( 'NONE',  ( -77.16926297131196577, -291.5342045405558338, -204.3999652569031582 ) ) ;
#13409 = CARTESIAN_POINT ( 'NONE',  ( 36.41477744666235594, -277.3666505435139129, -255.8693808431033858 ) ) ;
#13410 = CARTESIAN_POINT ( 'NONE',  ( -49.16631192836808850, -271.9014379791024112, -196.2465487400072846 ) ) ;
#13411 = CARTESIAN_POINT ( 'NONE',  ( 193.6287972472565286, 250.3431421874260252, 16.89650703080491922 ) ) ;
#13412 = CARTESIAN_POINT ( 'NONE',  ( 8.357681713831279779, -284.3522448830555618, -330.5348721822093694 ) ) ;
#13413 = CARTESIAN_POINT ( 'NONE',  ( -112.1648252337331684, -282.6270792006542365, -264.5128473677176544 ) ) ;
#13414 = DIRECTION ( 'NONE',  ( 0.000000000000000000, 0.000000000000000000, 1.000000000000000000 ) ) ;
#13415 = CARTESIAN_POINT ( 'NONE',  ( 21.63643313585999195, -292.9563448865433202, -314.0499071902663673 ) ) ;
#13416 = CARTESIAN_POINT ( 'NONE',  ( 19.62461394300983741, -285.0272024204127206, -222.7418884018648271 ) ) ;
#13417 = CARTESIAN_POINT ( 'NONE',  ( 195.4781563537916043, 39.36132622696000283, 15.50000000000000000 ) ) ;
#13418 = CARTESIAN_POINT ( 'NONE',  ( -83.61320397315417097, -293.6862896726714780, -329.4523320296373754 ) ) ;
#13419 = CARTESIAN_POINT ( 'NONE',  ( -113.6473458733575654, -283.0370184922652470, -269.9659240068711483 ) ) ;
#13420 = CARTESIAN_POINT ( 'NONE',  ( -49.29129547746521212, -281.4974432588339255, -197.5349716856522377 ) ) ;
#13421 = CARTESIAN_POINT ( 'NONE',  ( -113.8108999243323467, -285.6900414147070819, -275.7054469216830057 ) ) ;
#13422 = CARTESIAN_POINT ( 'NONE',  ( 22.09687524660148128, -279.1495881088794704, -223.0009075289071063 ) ) ;
#13423 = CARTESIAN_POINT ( 'NONE',  ( 28.22776145414211868, -287.9868029682542101, -302.4492109115161043 ) ) ;
#13424 = CARTESIAN_POINT ( 'NONE',  ( -83.36121065967330424, -279.1220558802091887, -327.8512440487249933 ) ) ;
#13425 = CARTESIAN_POINT ( 'NONE',  ( -91.42305940489916338, -280.0599531982767303, -221.0883231976278296 ) ) ;
#13426 = CARTESIAN_POINT ( 'NONE',  ( -36.60734052983629994, -288.0412138422577186, -194.9967321662178108 ) ) ;
#13427 = ORIENTED_EDGE ( 'NONE', *, *, #78743, .F. ) ;
#13428 = CARTESIAN_POINT ( 'NONE',  ( -95.56970503785156268, -297.0667602902819340, -219.8980202769687082 ) ) ;
#13429 = CARTESIAN_POINT ( 'NONE',  ( 25.63937023511052260, -290.0737759971342484, -310.4264593361086781 ) ) ;
#13430 = CARTESIAN_POINT ( 'NONE',  ( 175.2296996224750103, 133.0000000000000000, 24.00000000000001066 ) ) ;
#13431 = CARTESIAN_POINT ( 'NONE',  ( -37.37352853689063181, -276.5519495502701375, -190.3611179825600175 ) ) ;
#13432 = ORIENTED_EDGE ( 'NONE', *, *, #12942, .T. ) ;
#13433 = CARTESIAN_POINT ( 'NONE',  ( -0.9111392813347855002, -272.5344510735800441, -204.5981512583235542 ) ) ;
#13434 = VERTEX_POINT ( 'NONE', #8023 ) ;
#13435 = CARTESIAN_POINT ( 'NONE',  ( 24.22772893737646882, -292.5544397841053410, -315.2790340227438719 ) ) ;
#13436 = CARTESIAN_POINT ( 'NONE',  ( -109.6824026222367650, -272.0439004232600269, -259.4933110379953973 ) ) ;
#13437 = CARTESIAN_POINT ( 'NONE',  ( 29.43007877499893254, -288.6551880316985148, -239.1803980963613583 ) ) ;
#13438 = CARTESIAN_POINT ( 'NONE',  ( -2.694300823879401729, -282.2769208599086141, -204.9439034008434817 ) ) ;
#13439 = CARTESIAN_POINT ( 'NONE',  ( -103.2807020242395453, -291.4698329008068640, -309.0747240418270394 ) ) ;
#13440 = CARTESIAN_POINT ( 'NONE',  ( -82.54768766615792686, -290.9706569002191259, -332.0840226631880796 ) ) ;
#13441 = CARTESIAN_POINT ( 'NONE',  ( -111.1660888676446319, -286.7230776760448521, -257.0614793527809070 ) ) ;
#13442 = CARTESIAN_POINT ( 'NONE',  ( 6.182507220174499274, -280.7919689324610317, -206.8422752727321949 ) ) ;
#13443 = CARTESIAN_POINT ( 'NONE',  ( 8.021756606764650854, -292.5172960263182631, -330.7885206101265680 ) ) ;
#13444 = CARTESIAN_POINT ( 'NONE',  ( 10.82466232920867810, -280.5303210993626521, -210.2178094354298423 ) ) ;
#13445 = CARTESIAN_POINT ( 'NONE',  ( 21.00780541608521901, -278.0493432586400218, -316.2749593928757577 ) ) ;
#13446 = CARTESIAN_POINT ( 'NONE',  ( -95.95921662488163406, -298.4090924074130271, -317.1477375740089997 ) ) ;
#13447 = CARTESIAN_POINT ( 'NONE',  ( 30.93479702270423815, -274.2273258260684088, -303.8319642929401425 ) ) ;
#13448 = CARTESIAN_POINT ( 'NONE',  ( -47.80257052418233599, -229.5268262511776527, 21.50000000000000000 ) ) ;
#13449 = CARTESIAN_POINT ( 'NONE',  ( 30.38923339019997982, -281.4263598119951553, -297.7565388818734959 ) ) ;
#13450 = CARTESIAN_POINT ( 'NONE',  ( -22.99812280010903365, -278.0777919906360012, -345.6630850139743529 ) ) ;
#13451 = CARTESIAN_POINT ( 'NONE',  ( -46.25508524873569627, -275.2518853581394183, -197.4104836937257517 ) ) ;
#13452 = CARTESIAN_POINT ( 'NONE',  ( -4.862571616127334018, -285.5282560630977855, -200.8059138270792232 ) ) ;
#13453 = CARTESIAN_POINT ( 'NONE',  ( -90.56031213854326722, -293.0453471498078102, -218.9242309377517017 ) ) ;
#13454 = CARTESIAN_POINT ( 'NONE',  ( -35.56310030641039788, -275.6742104319949362, -194.1688814032446544 ) ) ;
#13455 = CARTESIAN_POINT ( 'NONE',  ( -35.55221805428152493, -275.3893021518002797, -193.8621512453394757 ) ) ;
#13456 = CARTESIAN_POINT ( 'NONE',  ( 201.2104617360081704, 60.19600395700749829, -10.00000000000000000 ) ) ;
#13457 = CARTESIAN_POINT ( 'NONE',  ( -108.6075794412710422, -298.2550165231253914, -293.3585549387979654 ) ) ;
#13458 = CARTESIAN_POINT ( 'NONE',  ( -37.57109341822355475, -281.0549083887496522, -345.2068460694425767 ) ) ;
#13459 = CARTESIAN_POINT ( 'NONE',  ( -109.4525424624268766, -290.5613925118248630, -243.2691022053596726 ) ) ;
#13460 = CARTESIAN_POINT ( 'NONE',  ( 20.28437203150357604, -272.9147228879465388, -222.9155427002361591 ) ) ;
#13461 = CARTESIAN_POINT ( 'NONE',  ( -36.59396453843113761, -287.6615115858832041, -194.1518809281834024 ) ) ;
#13462 = EDGE_CURVE ( 'NONE', #92893, #85445, #29349, .T. ) ;
#13463 = CARTESIAN_POINT ( 'NONE',  ( -77.41266988040224817, -290.4208653339846933, -208.9726544388240086 ) ) ;
#13464 = EDGE_LOOP ( 'NONE', ( #34100, #37556, #53503 ) ) ;
#13465 = CARTESIAN_POINT ( 'NONE',  ( -109.3167036544355994, -288.7987872607223494, -296.1735964451011682 ) ) ;
#13466 = CARTESIAN_POINT ( 'NONE',  ( -102.8662730884401242, -289.7823053697941305, -302.5887121378839311 ) ) ;
#13467 = EDGE_LOOP ( 'NONE', ( #74735, #90252, #1413, #93246 ) ) ;
#13468 = CARTESIAN_POINT ( 'NONE',  ( 21.26174044678009167, -289.3009245332277715, -319.8295853482165967 ) ) ;
#13469 = CARTESIAN_POINT ( 'NONE',  ( -96.90048367997997047, -278.2954240465713838, -312.6301846521262178 ) ) ;
#13470 = ADVANCED_FACE ( 'NONE', ( #85701 ), #71045, .T. ) ;
#13471 = CARTESIAN_POINT ( 'NONE',  ( 8.709529664622065681, -293.3576434169266349, -331.6862901672117232 ) ) ;
#13472 = CARTESIAN_POINT ( 'NONE',  ( -104.3241436687142283, -284.7115606680596898, -308.2401673304548240 ) ) ;
#13473 = CARTESIAN_POINT ( 'NONE',  ( -114.1310962253205048, -284.9618296608421701, -264.2541438960388405 ) ) ;
#13475 = CARTESIAN_POINT ( 'NONE',  ( 32.98095433172179725, -282.1453069389218626, -290.0286484974020595 ) ) ;
#13474 = CIRCLE ( 'NONE', #48235, 2.500000000000002220 ) ;
#13476 = CARTESIAN_POINT ( 'NONE',  ( 161.3244612304466159, 220.3882197354448351, -205.3170049622447380 ) ) ;
#13477 = CARTESIAN_POINT ( 'NONE',  ( -114.3093106393634457, -272.1053998528684588, -270.3554297553863535 ) ) ;
#13478 = CARTESIAN_POINT ( 'NONE',  ( 152.2530320059421172, 205.4471442928643796, -214.5373374589507875 ) ) ;
#13479 = CARTESIAN_POINT ( 'NONE',  ( -94.73303068411735239, -272.3882235749208576, -224.9867099471016445 ) ) ;
#13480 = CARTESIAN_POINT ( 'NONE',  ( -16.53984002476758874, -273.2475306711547205, -200.0123176032929564 ) ) ;
#13481 = CARTESIAN_POINT ( 'NONE',  ( -69.50790991053510481, -294.9719039886864493, -340.2673269313805235 ) ) ;
#13482 = CARTESIAN_POINT ( 'NONE',  ( -20.63144351428918810, -109.4982264660226576, -359.4589932074380840 ) ) ;
#13483 = CARTESIAN_POINT ( 'NONE',  ( 2.177696442613713756, -273.2546344100842362, -204.8514578770309811 ) ) ;
#13484 = CARTESIAN_POINT ( 'NONE',  ( -50.19060934628063109, -299.7468415103493271, -197.2463382883373697 ) ) ;
#13485 = CARTESIAN_POINT ( 'NONE',  ( -65.45817679620414253, -292.7554010913407865, -202.6445925528496161 ) ) ;
#13486 = ORIENTED_EDGE ( 'NONE', *, *, #75312, .F. ) ;
#13487 = CARTESIAN_POINT ( 'NONE',  ( -109.2130038030962140, -297.1495119633174795, -297.4801917730546279 ) ) ;
#13488 = CARTESIAN_POINT ( 'NONE',  ( 31.45945645978850180, -288.3715571168639826, -294.9454482309709533 ) ) ;
#13489 = CARTESIAN_POINT ( 'NONE',  ( 4.148728207827702796, -295.3114345161935148, -335.0975886019558629 ) ) ;
#13490 = CARTESIAN_POINT ( 'NONE',  ( -64.23879607682715687, -295.8862324646661364, -342.4449104238736368 ) ) ;
#13491 = CARTESIAN_POINT ( 'NONE',  ( 35.64203388477530865, -293.7600669576484620, -273.4868538195490828 ) ) ;
#13492 = ORIENTED_EDGE ( 'NONE', *, *, #4124, .F. ) ;
#13493 = CARTESIAN_POINT ( 'NONE',  ( 15.01136962998648627, -276.7038833034889080, -215.8774481058583490 ) ) ;
#13494 = ORIENTED_EDGE ( 'NONE', *, *, #2808, .T. ) ;
#13495 = CARTESIAN_POINT ( 'NONE',  ( -112.9345415303678521, -278.2400050572518353, -255.9641669578193728 ) ) ;
#13496 = CARTESIAN_POINT ( 'NONE',  ( 28.06607261930422581, -276.0477296939782264, -237.4182627388365177 ) ) ;
#13497 = CARTESIAN_POINT ( 'NONE',  ( -35.57017976351612987, -275.8341973885931111, -194.3821433837524353 ) ) ;
#13498 = CARTESIAN_POINT ( 'NONE',  ( 11.61645939648166781, -274.3966751625560505, -327.6455435786719477 ) ) ;
#13499 = CARTESIAN_POINT ( 'NONE',  ( -72.90371501913402597, -298.2190285998299828, -206.4922228517793030 ) ) ;
#13500 = CARTESIAN_POINT ( 'NONE',  ( -58.59562452442588665, -293.9071611937879993, -340.8142627927078934 ) ) ;
#13501 = DIRECTION ( 'NONE',  ( 1.000000000000000000, 0.000000000000000000, 0.000000000000000000 ) ) ;
#13502 = CARTESIAN_POINT ( 'NONE',  ( -101.8430560150894308, -279.5968424816661582, -228.3230530242886118 ) ) ;
#13503 = CARTESIAN_POINT ( 'NONE',  ( 34.16499180440508354, -275.9126168619873738, -285.0510129244357813 ) ) ;
#13504 = CARTESIAN_POINT ( 'NONE',  ( 19.92880294605765101, -285.5447086534340997, -219.5543232368817144 ) ) ;
#13505 = CARTESIAN_POINT ( 'NONE',  ( 50.87328029350005210, -301.1541834273529616, -195.1644496284779677 ) ) ;
#13506 = CARTESIAN_POINT ( 'NONE',  ( 82.67889722225095284, -297.1983528236896746, -196.2154390527394696 ) ) ;
#13507 = CARTESIAN_POINT ( 'NONE',  ( 17.90482521173569097, -286.0670936331465555, -222.3983911501829880 ) ) ;
#13508 = CARTESIAN_POINT ( 'NONE',  ( 18.74691343918777875, -279.1135153199455772, -222.0504407886007527 ) ) ;
#13509 = CARTESIAN_POINT ( 'NONE',  ( -32.90953544718430379, -278.6838097926006981, -196.9054794376219490 ) ) ;
#13510 = CARTESIAN_POINT ( 'NONE',  ( 37.53054988629661182, -289.6188008232904849, -275.5390759478623863 ) ) ;
#13511 = CARTESIAN_POINT ( 'NONE',  ( 25.72455309725347661, -277.2706316976319840, -307.9081312897818066 ) ) ;
#13512 = DIRECTION ( 'NONE',  ( -1.224646799147353207E-16, 1.000000000000000000, 0.000000000000000000 ) ) ;
#13513 = CARTESIAN_POINT ( 'NONE',  ( -12.22259462212732473, -274.9697639968247813, -342.1310461003222372 ) ) ;
#13514 = CARTESIAN_POINT ( 'NONE',  ( 34.47208661321728584, -276.0235836508264242, -256.6982960807466156 ) ) ;
#13515 = CARTESIAN_POINT ( 'NONE',  ( 22.27724916253489340, -282.9264981055762860, -224.5622743000091930 ) ) ;
#13516 = EDGE_CURVE ( 'NONE', #17445, #16234, #6655, .T. ) ;
#13517 = EDGE_CURVE ( 'NONE', #62986, #27803, #82242, .T. ) ;
#13518 = DIRECTION ( 'NONE',  ( 0.000000000000000000, 0.000000000000000000, 1.000000000000000000 ) ) ;
#13519 = CARTESIAN_POINT ( 'NONE',  ( 20.40462421395662318, -290.1412712707963237, -319.0917677415128537 ) ) ;
#13520 = CARTESIAN_POINT ( 'NONE',  ( 19.28000976063265171, -292.2350807588355224, -319.6207172758767570 ) ) ;
#13521 = DIRECTION ( 'NONE',  ( 1.000000000000000000, 0.000000000000000000, 0.000000000000000000 ) ) ;
#13522 = CARTESIAN_POINT ( 'NONE',  ( -0.2832286685470876697, -273.2408585354322668, -206.8805842461288478 ) ) ;
#13523 = CARTESIAN_POINT ( 'NONE',  ( 27.32195216699895113, -291.1997340639658773, -233.7940983206480325 ) ) ;
#13524 = CARTESIAN_POINT ( 'NONE',  ( 207.9738562182569979, 291.4636489450775798, -54.00000000000000711 ) ) ;
#13525 = DIRECTION ( 'NONE',  ( -0.000000000000000000, 1.000000000000000000, -0.000000000000000000 ) ) ;
#13526 = CARTESIAN_POINT ( 'NONE',  ( -86.94852856739331060, -288.2075733138581199, -328.4121739672628451 ) ) ;
#13527 = CARTESIAN_POINT ( 'NONE',  ( 24.73045771854012997, -285.2040517441172938, -226.5092194211633512 ) ) ;
#13528 = CARTESIAN_POINT ( 'NONE',  ( -94.73323218916556243, -285.3314873833873548, -316.4418447705828044 ) ) ;
#13529 = CARTESIAN_POINT ( 'NONE',  ( -48.34289721544971030, -283.9985990840805243, -342.6907480745336443 ) ) ;
#13530 = CARTESIAN_POINT ( 'NONE',  ( -83.28395150143130365, -293.4066108457627138, -210.5649731911737774 ) ) ;
#13531 = CIRCLE ( 'NONE', #37686, 4.025000000000000355 ) ;
#13532 = CARTESIAN_POINT ( 'NONE',  ( -2.160298843411634806, -274.6699511095773119, -337.2310155755658911 ) ) ;
#13533 = CARTESIAN_POINT ( 'NONE',  ( 2.403449765068615296, -274.9028237398029546, -204.4364082640365154 ) ) ;
#13534 = CARTESIAN_POINT ( 'NONE',  ( -89.76885926844288122, -289.3996929548900425, -215.8761442644450881 ) ) ;
#13535 = CARTESIAN_POINT ( 'NONE',  ( -97.05439269249619372, -277.8995837625887475, -318.9965197993265633 ) ) ;
#13536 = CARTESIAN_POINT ( 'NONE',  ( -110.9815431279644145, -298.3745585545444214, -282.5685061910308491 ) ) ;
#13537 = DIRECTION ( 'NONE',  ( 1.000000000000000000, 0.000000000000000000, 0.000000000000000000 ) ) ;
#13538 = CARTESIAN_POINT ( 'NONE',  ( 196.7806748523260012, 249.5000000000000568, -12.67104836398113576 ) ) ;
#13539 = CARTESIAN_POINT ( 'NONE',  ( -91.87598027012479918, -283.9385504751987241, -221.0191736467336909 ) ) ;
#13540 = CARTESIAN_POINT ( 'NONE',  ( -12.15633219618137417, -278.3795462078329024, -199.6617102941171140 ) ) ;
#13541 = DIRECTION ( 'NONE',  ( 1.000000000000000000, 0.000000000000000000, 1.224646799147353207E-16 ) ) ;
#13542 = CARTESIAN_POINT ( 'NONE',  ( 17.60392472315898260, -273.2997933078729034, -217.3354019604138614 ) ) ;
#13543 = CARTESIAN_POINT ( 'NONE',  ( -9.957867048168388635, -276.0334830791300647, -338.1538900878304617 ) ) ;
#13544 = CARTESIAN_POINT ( 'NONE',  ( 27.77974248919749556, -295.5390377263745449, -304.9652207855666575 ) ) ;
#13545 = CARTESIAN_POINT ( 'NONE',  ( 27.59696584744239445, -279.9350265949417462, -229.4637475159331359 ) ) ;
#13546 = CARTESIAN_POINT ( 'NONE',  ( -9.129195875786994208, -295.6152360973462123, -337.9577774052037284 ) ) ;
#13547 = CARTESIAN_POINT ( 'NONE',  ( -27.79267219791408650, -296.2486165386041534, -346.3226617902165003 ) ) ;
#13548 = CARTESIAN_POINT ( 'NONE',  ( -40.51584640065840404, -297.8444832038135814, -197.4176100758153609 ) ) ;
#13549 = CARTESIAN_POINT ( 'NONE',  ( -110.0535777945787856, -292.7890840132592984, -251.9244869546794519 ) ) ;
#13550 = CARTESIAN_POINT ( 'NONE',  ( -114.3267303197576865, -284.7594099805384076, -267.1165243605342425 ) ) ;
#13551 = CARTESIAN_POINT ( 'NONE',  ( -70.83508992561124273, -271.7546121252059947, -202.4015835200080744 ) ) ;
#13552 = CARTESIAN_POINT ( 'NONE',  ( -36.56330013558817882, -285.8949894264509908, -193.3520135210320632 ) ) ;
#13553 = CARTESIAN_POINT ( 'NONE',  ( -92.52950425866059447, -281.2368227782607164, -220.1002676227183485 ) ) ;
#13554 = CARTESIAN_POINT ( 'NONE',  ( -65.17156383942467812, -284.7382118471848571, -202.5656685514693436 ) ) ;
#13555 = CARTESIAN_POINT ( 'NONE',  ( -99.04992516383904899, -287.9740693113418502, -312.9885224604685163 ) ) ;
#13556 = CARTESIAN_POINT ( 'NONE',  ( 181.0595704366054690, 252.2700355933461651, -164.3583243123303532 ) ) ;
#13557 = CARTESIAN_POINT ( 'NONE',  ( -14.54085261312238408, -285.8633414116842459, -200.8954475590673212 ) ) ;
#13558 = CARTESIAN_POINT ( 'NONE',  ( -18.96307513166993530, -283.7625496074473972, -344.9480931306172806 ) ) ;
#13559 = CARTESIAN_POINT ( 'NONE',  ( -99.83251601703139499, -290.2032452199792374, -225.7772852312661485 ) ) ;
#13560 = CARTESIAN_POINT ( 'NONE',  ( -67.06934635342329898, -281.2690270038789322, -200.1991092711630529 ) ) ;
#13561 = CARTESIAN_POINT ( 'NONE',  ( -111.6919312326862581, -279.6395943707336755, -288.4531644820152678 ) ) ;
#13562 = CARTESIAN_POINT ( 'NONE',  ( 7.144005322061190100, -280.5105622456058541, -212.4177844322115334 ) ) ;
#13563 = CARTESIAN_POINT ( 'NONE',  ( 35.77807340377263046, -277.3373698500812452, -253.6154860658987218 ) ) ;
#13564 = CARTESIAN_POINT ( 'NONE',  ( -93.68946994483439994, -295.8366181018540715, -322.8584262593573726 ) ) ;
#13565 = CARTESIAN_POINT ( 'NONE',  ( -71.95741865491031319, -287.5321977798403168, -336.5087509784855229 ) ) ;
#13566 = CARTESIAN_POINT ( 'NONE',  ( -95.52605175127334292, -296.0974704478106219, -225.7446226865440622 ) ) ;
#13567 = ORIENTED_EDGE ( 'NONE', *, *, #14703, .T. ) ;
#13568 = VERTEX_POINT ( 'NONE', #51115 ) ;
#13569 = CARTESIAN_POINT ( 'NONE',  ( -34.77282814818167367, -284.9398170641782713, -344.7694654354556860 ) ) ;
#13570 = CARTESIAN_POINT ( 'NONE',  ( -108.9062948670838864, -296.0266673669443662, -284.9353404755230486 ) ) ;
#13571 = CARTESIAN_POINT ( 'NONE',  ( 36.78026919083271196, -294.3838242233839537, -250.6273429870099392 ) ) ;
#13572 = CARTESIAN_POINT ( 'NONE',  ( -82.85170864116497569, -284.3447430437678918, -327.6338618906827378 ) ) ;
#13573 = CARTESIAN_POINT ( 'NONE',  ( -0.1489144665720578964, -273.5931885471683813, -203.1932328212933783 ) ) ;
#13574 = CARTESIAN_POINT ( 'NONE',  ( 7.881276161537572378, -289.1040618707446583, -332.6216034741153749 ) ) ;
#13575 = CARTESIAN_POINT ( 'NONE',  ( -96.22759931379648890, -282.0417459461705789, -318.0549475543778044 ) ) ;
#13576 = CARTESIAN_POINT ( 'NONE',  ( -107.7103179318719555, -290.4855756983972128, -301.7012089019423797 ) ) ;
#13577 = CARTESIAN_POINT ( 'NONE',  ( -13.27690408578824410, -289.0640583405504458, -339.3029273451480208 ) ) ;
#13578 = PLANE ( 'NONE',  #58088 ) ;
#13579 = FACE_OUTER_BOUND ( 'NONE', #9602, .T. ) ;
#13580 = CARTESIAN_POINT ( 'NONE',  ( 64.89032082630019715, 46.31952104162717632, -315.2875490666531277 ) ) ;
#13581 = CARTESIAN_POINT ( 'NONE',  ( -110.4683760289727132, -287.8380690714490129, -287.0191576251351080 ) ) ;
#13582 = ORIENTED_EDGE ( 'NONE', *, *, #62145, .F. ) ;
#13583 = CARTESIAN_POINT ( 'NONE',  ( 11.52204353826855332, -279.6695816220120037, -215.7116840629992396 ) ) ;
#13584 = CARTESIAN_POINT ( 'NONE',  ( 21.83732480571998025, -274.5565534830449792, -221.1311748634412879 ) ) ;
#13585 = CARTESIAN_POINT ( 'NONE',  ( -48.86564649644491709, -279.1992999849621810, -344.3544948652295261 ) ) ;
#13586 = CARTESIAN_POINT ( 'NONE',  ( -10.91761978339317452, -93.10046803755994915, -357.6389493721724762 ) ) ;
#13587 = CARTESIAN_POINT ( 'NONE',  ( 29.23949249098504666, -280.6182974651587756, -307.9595883749491350 ) ) ;
#13588 = CARTESIAN_POINT ( 'NONE',  ( 4.287065625126643020, -280.5083902097566124, -332.3824254439375636 ) ) ;
#13589 = CARTESIAN_POINT ( 'NONE',  ( -109.8529884865901636, -298.6035312422611128, -247.4689788413477913 ) ) ;
#13590 = CARTESIAN_POINT ( 'NONE',  ( 17.13063089981426401, -294.7405982199778123, -319.0703672003883185 ) ) ;
#13591 = ORIENTED_EDGE ( 'NONE', *, *, #57795, .F. ) ;
#13592 = CARTESIAN_POINT ( 'NONE',  ( -109.1481313034094853, -289.0311349668756975, -286.0747124883238826 ) ) ;
#13593 = CARTESIAN_POINT ( 'NONE',  ( -41.19597260903686475, -274.6563820257134125, -193.5075125659404875 ) ) ;
#13594 = CARTESIAN_POINT ( 'NONE',  ( -104.3797064758031325, -272.9419661265707191, -241.3382807244666139 ) ) ;
#13595 = VERTEX_POINT ( 'NONE', #6179 ) ;
#13596 = PRESENTATION_STYLE_ASSIGNMENT (( #71358 ) ) ;
#13597 = CARTESIAN_POINT ( 'NONE',  ( 204.6539576904058606, 293.9636489450775230, -7.999911143031724237 ) ) ;
#13598 = TOROIDAL_SURFACE ( 'NONE', #52898, 4.500000000000002665, 0.5000000000000000000 ) ;
#13599 = CARTESIAN_POINT ( 'NONE',  ( 19.06517424551938333, -281.9703343784356662, -223.5176013457259785 ) ) ;
#13600 = CARTESIAN_POINT ( 'NONE',  ( -2.870138647403114085, -282.2615066253839586, -202.6288964700407575 ) ) ;
#13601 = VECTOR ( 'NONE', #61721, 1000.000000000000000 ) ;
#13602 = CARTESIAN_POINT ( 'NONE',  ( -108.2534988450514106, -283.8517119234795132, -252.0601548530923992 ) ) ;
#13603 = CARTESIAN_POINT ( 'NONE',  ( -21.96123867709017574, -282.1115884320992109, -197.6839628719043276 ) ) ;
#13604 = CARTESIAN_POINT ( 'NONE',  ( 33.90762946340650075, -274.2782208065635245, -289.1824034511878381 ) ) ;
#13605 = CARTESIAN_POINT ( 'NONE',  ( 208.3297354249494902, 27.64700571354669734, 12.00000001296664820 ) ) ;
#13606 = CARTESIAN_POINT ( 'NONE',  ( 219.7099725226080977, -147.7221692137691775, -1.978481845683818907 ) ) ;
#13607 = CARTESIAN_POINT ( 'NONE',  ( -59.60842893775332385, -278.1362424746458828, -343.9026138077355768 ) ) ;
#13608 = CARTESIAN_POINT ( 'NONE',  ( 175.2296996224750103, 138.1603916158177583, -24.00000000000001421 ) ) ;
#13609 = VERTEX_POINT ( 'NONE', #63962 ) ;
#13610 = DIRECTION ( 'NONE',  ( -0.000000000000000000, -0.000000000000000000, -1.000000000000000000 ) ) ;
#13611 = CARTESIAN_POINT ( 'NONE',  ( -34.51487717437815661, -284.9966714366802876, -345.6632818113504868 ) ) ;
#13612 = CARTESIAN_POINT ( 'NONE',  ( 34.64389043881742936, -292.5764393517611666, -257.2270819024182060 ) ) ;
#13613 = CARTESIAN_POINT ( 'NONE',  ( -51.67444999180394660, -288.5794835329385251, -345.9116644241893823 ) ) ;
#13614 = CARTESIAN_POINT ( 'NONE',  ( -107.4855755694752446, -283.1033375590394030, -246.5827677832739369 ) ) ;
#13616 = CARTESIAN_POINT ( 'NONE',  ( -59.00686868212586234, -287.5760540205180860, -341.1860850154860145 ) ) ;
#13615 = CARTESIAN_POINT ( 'NONE',  ( -91.94634617264296139, -283.8284699686502677, -220.9536436097992578 ) ) ;
#13617 = CARTESIAN_POINT ( 'NONE',  ( -5.848719225844257963, -283.8337708325140056, -336.6721738225040781 ) ) ;
#13618 = CARTESIAN_POINT ( 'NONE',  ( 30.74831331479195740, -273.1375551194737454, -238.7929471153562417 ) ) ;
#13619 = CARTESIAN_POINT ( 'NONE',  ( -112.2083134290982258, -283.1348102441622245, -255.8943486732702581 ) ) ;
#13620 = CARTESIAN_POINT ( 'NONE',  ( -89.30747421619737736, -297.7833327776335750, -324.5117861945354321 ) ) ;
#13621 = CARTESIAN_POINT ( 'NONE',  ( 0.6183570199544879964, -284.5567248697578293, -205.4688542527828474 ) ) ;
#13622 = CARTESIAN_POINT ( 'NONE',  ( -109.7227936589355721, -279.3467563468761909, -281.5139538366073566 ) ) ;
#13623 = CARTESIAN_POINT ( 'NONE',  ( 10.88142246406368230, -288.7170840258521594, -212.6342301019168701 ) ) ;
#13624 = CARTESIAN_POINT ( 'NONE',  ( 76.08708295871279859, -296.0521521680024080, -472.6442049081569508 ) ) ;
#13625 = EDGE_CURVE ( 'NONE', #81684, #49342, #44460, .T. ) ;
#13626 = ADVANCED_FACE ( 'NONE', ( #35533 ), #3647, .T. ) ;
#13627 = CARTESIAN_POINT ( 'NONE',  ( 60.30156426812556703, -249.1647034777049328, -21.50000000000000000 ) ) ;
#13628 = CARTESIAN_POINT ( 'NONE',  ( 23.73696742204157673, -296.0741533896636497, -314.8656212193303077 ) ) ;
#13629 = CARTESIAN_POINT ( 'NONE',  ( -111.8949662158130280, -276.4411255330553558, -278.9954447842501963 ) ) ;
#13630 = CARTESIAN_POINT ( 'NONE',  ( -99.06875761925890345, -290.3591839925926479, -224.5796092927287191 ) ) ;
#13631 = CARTESIAN_POINT ( 'NONE',  ( 26.47433489965567333, -292.4550618215052395, -307.4280046479551061 ) ) ;
#13632 = CARTESIAN_POINT ( 'NONE',  ( -7.785853932361445295, -279.1325913649729955, -203.0591992792633675 ) ) ;
#13633 = CARTESIAN_POINT ( 'NONE',  ( -77.31733040410809110, -271.5913096368487913, -207.5657106607734761 ) ) ;
#13634 = CARTESIAN_POINT ( 'NONE',  ( -101.5627074419343217, -292.3538836556028286, -234.5227331140128513 ) ) ;
#13635 = CARTESIAN_POINT ( 'NONE',  ( -85.33152481854862970, -281.9090924074130839, -210.2361428286348826 ) ) ;
#13636 = CARTESIAN_POINT ( 'NONE',  ( -19.46863260694070519, -293.3063195641213383, -344.5994749119380458 ) ) ;
#13637 = CARTESIAN_POINT ( 'NONE',  ( 22.62349163323107604, -289.7471043955331993, -313.3799068230014768 ) ) ;
#13638 = CARTESIAN_POINT ( 'NONE',  ( 1.205639248390016460, -290.7989103079572146, -204.8175700132173063 ) ) ;
#13639 = CARTESIAN_POINT ( 'NONE',  ( -107.5693236899448380, -292.2669988261392859, -248.3310058580287034 ) ) ;
#13640 = CARTESIAN_POINT ( 'NONE',  ( 29.33919985515026596, -285.8906705383787994, 25.50000000000000000 ) ) ;
#13641 = CARTESIAN_POINT ( 'NONE',  ( -36.21387402543916068, -292.8694486054196773, -197.1958302686302886 ) ) ;
#13642 = CARTESIAN_POINT ( 'NONE',  ( 196.0143093133015384, 250.0000000000000568, 11.99999999999998757 ) ) ;
#13643 = CARTESIAN_POINT ( 'NONE',  ( -113.2746579064918961, -291.8891979233982852, -259.8630643500327437 ) ) ;
#13645 = CARTESIAN_POINT ( 'NONE',  ( 18.47658724361285820, -292.8837535087899937, -223.3151957906105451 ) ) ;
#13644 = CARTESIAN_POINT ( 'NONE',  ( 20.33448348700062880, -280.2395526681830233, -318.8571451360037941 ) ) ;
#13646 = CARTESIAN_POINT ( 'NONE',  ( 1.373973389439363757, -280.5540929698765353, -203.7414417187063975 ) ) ;
#13647 = CARTESIAN_POINT ( 'NONE',  ( 19.76497235415774156, -281.9207065076909657, -322.0585938682344818 ) ) ;
#13648 = CARTESIAN_POINT ( 'NONE',  ( -1.200860039792204459, -284.5310798962817671, -204.5849545870420059 ) ) ;
#13649 = CARTESIAN_POINT ( 'NONE',  ( 33.15698741160961305, -279.3862654943009147, -246.9438226472128122 ) ) ;
#13650 = CARTESIAN_POINT ( 'NONE',  ( -103.6516099054150288, -283.0178173562750317, -235.2072095585744762 ) ) ;
#13651 = DIRECTION ( 'NONE',  ( 0.5941640067486205767, 0.8043439146810431595, 0.000000000000000000 ) ) ;
#13652 = CARTESIAN_POINT ( 'NONE',  ( 14.70273203987860100, -279.2487375289848615, -214.4848832783396517 ) ) ;
#13653 = CARTESIAN_POINT ( 'NONE',  ( -73.45524823339481202, -284.5052301921081721, -202.6465284059426324 ) ) ;
#13654 = CARTESIAN_POINT ( 'NONE',  ( -1.652774354567535298, -275.3408660899337974, -206.4804892536207603 ) ) ;
#13655 = CARTESIAN_POINT ( 'NONE',  ( 195.7610338615059220, 41.66501297569730156, 14.26493301926425339 ) ) ;
#13656 = CARTESIAN_POINT ( 'NONE',  ( -12.00448043137212295, -293.9874806121997608, -200.9924027580908614 ) ) ;
#13657 = CARTESIAN_POINT ( 'NONE',  ( -15.95977647059763882, -275.7485460722206199, -196.9480469432443215 ) ) ;
#13658 = CARTESIAN_POINT ( 'NONE',  ( -61.80090498741567728, -277.0455669578506672, -339.2177444549793108 ) ) ;
#13659 = CARTESIAN_POINT ( 'NONE',  ( -111.9215034743445898, -290.4785412741468349, -289.5672643941420574 ) ) ;
#13660 = CARTESIAN_POINT ( 'NONE',  ( 35.79177982547468417, -279.8742767763482675, -289.3560728585725315 ) ) ;
#13661 = CARTESIAN_POINT ( 'NONE',  ( -13.86443462074993249, -292.1817741386894909, -196.9715348642621393 ) ) ;
#13663 = CARTESIAN_POINT ( 'NONE',  ( -99.90641824617176781, -290.1334969489502669, -232.2945382229105462 ) ) ;
#13662 = CIRCLE ( 'NONE', #80220, 6.154241149514405151 ) ;
#13664 = CARTESIAN_POINT ( 'NONE',  ( 3.126151351717162186, -292.5088930849533426, -333.5677475182520766 ) ) ;
#13665 = VERTEX_POINT ( 'NONE', #92803 ) ;
#13666 = CARTESIAN_POINT ( 'NONE',  ( 151.9826577741488904, 20.03748314400953134, 9.225496140117414257 ) ) ;
#13667 = CARTESIAN_POINT ( 'NONE',  ( -3.602269449905252774, -292.0177838136859236, -205.5564942329011728 ) ) ;
#13668 = FACE_OUTER_BOUND ( 'NONE', #74197, .T. ) ;
#13669 = AXIS2_PLACEMENT_3D ( 'NONE', #92817, #29371, #43103 ) ;
#13670 = CARTESIAN_POINT ( 'NONE',  ( -37.37352853689063181, -280.5523547857346784, -340.3611179825599606 ) ) ;
#13671 = CARTESIAN_POINT ( 'NONE',  ( -89.43979183231243724, -296.3986071571849834, -213.9099674330401513 ) ) ;
#13672 = CARTESIAN_POINT ( 'NONE',  ( -109.7524993311614878, -285.5541248229128541, -295.0587784193310767 ) ) ;
#13673 = CARTESIAN_POINT ( 'NONE',  ( 16.89203854658096660, -286.6856223635634819, -221.4783421779349055 ) ) ;
#13674 = CARTESIAN_POINT ( 'NONE',  ( 36.29577892867075661, -277.1241564719789494, -274.3308617939764531 ) ) ;
#13675 = CARTESIAN_POINT ( 'NONE',  ( -89.67255134133135641, -293.8142032484376500, -323.6628049503987654 ) ) ;
#13676 = CARTESIAN_POINT ( 'NONE',  ( -68.92973617321707991, -297.2333787808157695, -337.3091103341832877 ) ) ;
#13677 = CARTESIAN_POINT ( 'NONE',  ( 1.066202684958064362, -275.3223662342861076, -332.9665215625577162 ) ) ;
#13678 = ORIENTED_EDGE ( 'NONE', *, *, #65011, .F. ) ;
#13679 = CARTESIAN_POINT ( 'NONE',  ( 194.3488207764574156, 40.17711433623663453, 14.50727004101163864 ) ) ;
#13680 = CARTESIAN_POINT ( 'NONE',  ( -114.3451773695185523, -296.1925527361041759, -272.4649786494220507 ) ) ;
#13681 = CARTESIAN_POINT ( 'NONE',  ( -10.17624887484230811, -290.6150761644905742, -339.7226338035293338 ) ) ;
#13682 = CARTESIAN_POINT ( 'NONE',  ( -38.45329906659297592, -296.0380649664108432, -195.3662034614006870 ) ) ;
#13683 = VERTEX_POINT ( 'NONE', #44001 ) ;
#13684 = CARTESIAN_POINT ( 'NONE',  ( 17.06483578370574605, -279.8632155322168273, -216.1317071792590809 ) ) ;
#13685 = CARTESIAN_POINT ( 'NONE',  ( -58.81489195178848206, -295.9740993578237749, -344.2557291067359415 ) ) ;
#13686 = CARTESIAN_POINT ( 'NONE',  ( -95.45906256776146392, -288.0267678487963963, -318.9886320374207571 ) ) ;
#13687 = CARTESIAN_POINT ( 'NONE',  ( -111.5705032566660577, -296.6299238462630115, -290.7530055282207400 ) ) ;
#13688 = CARTESIAN_POINT ( 'NONE',  ( -0.08381094472334088552, -292.8960675533546123, -207.5603442582150819 ) ) ;
#13689 = CYLINDRICAL_SURFACE ( 'NONE', #29444, 4.999999999999990230 ) ;
#13690 = CARTESIAN_POINT ( 'NONE',  ( -113.5000000000000568, -296.0521521680024080, -537.7509286889328450 ) ) ;
#13691 = DIRECTION ( 'NONE',  ( 0.2916739763039743472, 0.000000000000000000, 0.9565177946839404921 ) ) ;
#13692 = CARTESIAN_POINT ( 'NONE',  ( -67.75955034644672992, -290.9642795826238739, -340.3429880788557966 ) ) ;
#13693 = CARTESIAN_POINT ( 'NONE',  ( 35.65787339142939771, -296.4086741954485547, -190.3901485728259217 ) ) ;
#13694 = ORIENTED_EDGE ( 'NONE', *, *, #1952, .T. ) ;
#13695 = CARTESIAN_POINT ( 'NONE',  ( -8.891102911485702975, -279.7632998165365166, -198.9196992910592030 ) ) ;
#13696 = CARTESIAN_POINT ( 'NONE',  ( -101.9720056611995744, -286.0472506389759815, -308.0831543949820457 ) ) ;
#13697 = CARTESIAN_POINT ( 'NONE',  ( -29.50518370236875754, -284.7242987085503501, -194.3532545561998859 ) ) ;
#13698 = CARTESIAN_POINT ( 'NONE',  ( -7.666487825732072992, -286.7401244687881672, -338.6855036344348946 ) ) ;
#13699 = CARTESIAN_POINT ( 'NONE',  ( 31.42188628798750472, -276.9975103334746223, -238.4262893452703622 ) ) ;
#13700 = ORIENTED_EDGE ( 'NONE', *, *, #60977, .F. ) ;
#13702 = CARTESIAN_POINT ( 'NONE',  ( -107.3223024918708006, -278.1801442563533442, -249.2280169064609368 ) ) ;
#13701 = CARTESIAN_POINT ( 'NONE',  ( -83.00675806506637855, -277.6970129023891900, -327.3796877340411697 ) ) ;
#13703 = CARTESIAN_POINT ( 'NONE',  ( 15.80289339776934021, -275.8635360488769379, -215.0696657665166924 ) ) ;
#13704 = CARTESIAN_POINT ( 'NONE',  ( -67.19349695917806287, -278.4642760872553140, -199.8141198524807294 ) ) ;
#13705 = CARTESIAN_POINT ( 'NONE',  ( -78.63461375671516862, -207.3269539590848751, -354.3927223517632683 ) ) ;
#13706 = CARTESIAN_POINT ( 'NONE',  ( -38.36632987209058854, -274.9808488121906862, -193.6032496701160142 ) ) ;
#13707 = CARTESIAN_POINT ( 'NONE',  ( -80.30880217689754375, -298.9081948954108157, -207.1117779230685301 ) ) ;
#13708 = CARTESIAN_POINT ( 'NONE',  ( -37.30987171927208124, -291.5519495502701943, -345.3611179825600175 ) ) ;
#13709 = ORIENTED_EDGE ( 'NONE', *, *, #1671, .T. ) ;
#13710 = DIRECTION ( 'NONE',  ( 0.000000000000000000, 1.000000000000000000, -1.224646799147353207E-16 ) ) ;
#13711 = CARTESIAN_POINT ( 'NONE',  ( 9.216257597466716689, -287.7890620028209696, -213.7344224665082777 ) ) ;
#13712 = CARTESIAN_POINT ( 'NONE',  ( -82.68934215043969971, -287.2024122755286726, -209.3236482214858540 ) ) ;
#13713 = CARTESIAN_POINT ( 'NONE',  ( -34.58245312017958639, -288.3652924627605785, -343.4606100419794075 ) ) ;
#13714 = CARTESIAN_POINT ( 'NONE',  ( -110.1684554879753932, -283.7468950378806198, -295.1762465721661783 ) ) ;
#13715 = CARTESIAN_POINT ( 'NONE',  ( -35.62397099359790786, -278.4738950980721484, -196.5685699317976116 ) ) ;
#13716 = CARTESIAN_POINT ( 'NONE',  ( -24.95871440880734582, -288.0720333736266525, -197.1138233734441769 ) ) ;
#13717 = CARTESIAN_POINT ( 'NONE',  ( 35.82578007256254438, -280.1522813798314360, -279.5638461576048712 ) ) ;
#13718 = CARTESIAN_POINT ( 'NONE',  ( 7.897045284182422797, -277.7347459944202228, -328.3457433943577257 ) ) ;
#13719 = CARTESIAN_POINT ( 'NONE',  ( 35.70430180562726719, -276.0246438604691548, -268.8544518083155594 ) ) ;
#13720 = CARTESIAN_POINT ( 'NONE',  ( 31.32464673198284544, -286.7870503003185263, -304.4356923307113902 ) ) ;
#13721 =( BOUNDED_SURFACE ( )  B_SPLINE_SURFACE ( 3, 2, ( 
 ( #29592, #88250, #87776 ),
 ( #58471, #44699, #52274 ),
 ( #59872, #81153, #23860 ),
 ( #52726, #67436, #44226 ),
 ( #24320, #30045, #2563 ),
 ( #31442, #53197, #73136 ),
 ( #82075, #67891, #8261 ),
 ( #37142, #26670, #55560 ),
 ( #75454, #47012, #77327 ),
 ( #39437, #32833, #12460 ),
 ( #41307, #83951, #18624 ),
 ( #40368, #54138, #82553 ),
 ( #61723, #60792, #69285 ),
 ( #76859, #4414, #25713 ),
 ( #89630, #10574, #3959 ),
 ( #47490, #68353, #18159 ) ),
 .UNSPECIFIED., .F., .F., .T. ) 
 B_SPLINE_SURFACE_WITH_KNOTS ( ( 4, 2, 2, 2, 2, 2, 2, 4 ),
 ( 3, 3 ),
 ( 1.986477369973030482, 2.275256190877221307, 2.419645601329316609, 2.564035011781411910, 2.708424422233507212, 2.852813832685602513, 2.997203243137697815, 3.141592653589793116 ),
 ( 0.000000000000000000, 1.000000000000000000 ),
 .UNSPECIFIED. ) 
 GEOMETRIC_REPRESENTATION_ITEM ( )  RATIONAL_B_SPLINE_SURFACE ( (
 ( 1.000000000000000000, 0.9583671019093122911, 1.000000000000000000),
 ( 1.000000000000000000, 0.9398658125636130123, 1.000000000000000000),
 ( 1.000000000000000000, 0.9157002655848520689, 1.000000000000000000),
 ( 1.000000000000000000, 0.8756259400452285346, 1.000000000000000000),
 ( 1.000000000000000000, 0.8616433317033627137, 1.000000000000000000),
 ( 1.000000000000000000, 0.8334785261035606574, 1.000000000000000000),
 ( 1.000000000000000000, 0.8192978668689707700, 1.000000000000000000),
 ( 1.000000000000000000, 0.7919708659745015034, 1.000000000000000000),
 ( 1.000000000000000000, 0.7788285231916702855, 1.000000000000000000),
 ( 1.000000000000000000, 0.7549177526733148458, 1.000000000000000000),
 ( 1.000000000000000000, 0.7441566529437350086, 1.000000000000000000),
 ( 1.000000000000000000, 0.7262859251464029997, 1.000000000000000000),
 ( 1.000000000000000000, 0.7191857644035757335, 1.000000000000000000),
 ( 1.000000000000000000, 0.7095926089624606803, 1.000000000000000000),
 ( 1.000000000000000000, 0.7070960980132692253, 1.000000000000000000),
 ( 1.000000000000000000, 0.7071067811865473507, 1.000000000000000000) ) ) 
 REPRESENTATION_ITEM ( '' )  SURFACE ( )  );
#13722 = CARTESIAN_POINT ( 'NONE',  ( -63.84670351252362508, -284.1919843359269748, -342.4835390174972645 ) ) ;
#13723 = CARTESIAN_POINT ( 'NONE',  ( -63.88489860875980497, -283.8815490215756085, -342.5759746091673037 ) ) ;
#13724 = CARTESIAN_POINT ( 'NONE',  ( -34.31545332652866875, -280.2579005600961750, -197.4113285917850646 ) ) ;
#13725 = ORIENTED_EDGE ( 'NONE', *, *, #14175, .T. ) ;
#13726 = VERTEX_POINT ( 'NONE', #49717 ) ;
#13727 = CARTESIAN_POINT ( 'NONE',  ( 195.7261261297331885, 19.57027967189588935, -12.91595659652283423 ) ) ;
#13728 = CARTESIAN_POINT ( 'NONE',  ( -4.841090942817596776, -290.4891506201363995, -338.8152383476980276 ) ) ;
#13729 =( BOUNDED_CURVE ( )  B_SPLINE_CURVE ( 3, ( #52139, #67754, #61136, #68218 ),
 .UNSPECIFIED., .F., .F. ) 
 B_SPLINE_CURVE_WITH_KNOTS ( ( 4, 4 ),
 ( 0.7297276562269648936, 1.570796326794896558 ),
 .UNSPECIFIED. ) 
 CURVE ( )  GEOMETRIC_REPRESENTATION_ITEM ( )  RATIONAL_B_SPLINE_CURVE ( ( 1.000000000000000000, 0.9419139527835176384, 0.9419139527835176384, 1.000000000000000000 ) ) 
 REPRESENTATION_ITEM ( '' )  );
#13730 = CARTESIAN_POINT ( 'NONE',  ( -99.47959105461899298, -288.6413400722894380, -315.0174222178917489 ) ) ;
#13731 = CARTESIAN_POINT ( 'NONE',  ( -104.5910301538779521, -272.0008656080828473, -241.2337538751546617 ) ) ;
#13732 = EDGE_CURVE ( 'NONE', #74948, #9812, #77728, .T. ) ;
#13733 = CARTESIAN_POINT ( 'NONE',  ( 37.96378059450398013, -292.7049623297373273, -254.7274315520643313 ) ) ;
#13734 = TOROIDAL_SURFACE ( 'NONE', #66636, 2.500000000000007994, 0.5000000000000000000 ) ;
#13735 = CARTESIAN_POINT ( 'NONE',  ( -109.3442708911288008, -288.8262202221503117, -286.1149974315113127 ) ) ;
#13736 = CARTESIAN_POINT ( 'NONE',  ( 20.14686314483438423, -291.1413440135990527, -223.7251976090080063 ) ) ;
#13737 = CARTESIAN_POINT ( 'NONE',  ( 34.09105620740524500, -288.9785406157570833, -287.2280035422941182 ) ) ;
#13738 = CARTESIAN_POINT ( 'NONE',  ( -4.829096099716510437, -288.9805209788416391, -202.7746430608542312 ) ) ;
#13739 = CARTESIAN_POINT ( 'NONE',  ( -37.47186702827235649, -291.0539023648515240, -345.3737421144371069 ) ) ;
#13740 = CARTESIAN_POINT ( 'NONE',  ( -111.3621068081675816, -288.7195278116091117, -257.2841220243305997 ) ) ;
#13741 = AXIS2_PLACEMENT_3D ( 'NONE', #80245, #79787, #14477 ) ;
#13742 = CARTESIAN_POINT ( 'NONE',  ( -37.26740574209865287, -294.0532745998751807, -195.3485791444505537 ) ) ;
#13743 = CARTESIAN_POINT ( 'NONE',  ( -109.7290635677364179, -285.3430187533374465, -281.7981982519130497 ) ) ;
#13744 = CARTESIAN_POINT ( 'NONE',  ( -25.33987449247666746, -294.2049700456593087, -196.1587958794362123 ) ) ;
#13745 = CARTESIAN_POINT ( 'NONE',  ( -114.3366298191176895, -272.7563261381201301, -270.3637176062232470 ) ) ;
#13746 = EDGE_CURVE ( 'NONE', #36646, #41846, #72444, .T. ) ;
#13747 = CARTESIAN_POINT ( 'NONE',  ( 194.7510731661265595, -143.7221692137691775, -22.50000000000000000 ) ) ;
#13748 = CARTESIAN_POINT ( 'NONE',  ( -9.790537445922979032, -300.3146391628407628, -194.7921782358073415 ) ) ;
#13749 = CARTESIAN_POINT ( 'NONE',  ( -5.972965751319449623, -281.8261878425273608, -336.4703156422215216 ) ) ;
#13750 = CARTESIAN_POINT ( 'NONE',  ( -1.494546149260095325, -280.5767895270439567, -336.2543377224904475 ) ) ;
#13751 = CARTESIAN_POINT ( 'NONE',  ( -109.2899514968314776, -295.4057083103001560, -297.4854969212216247 ) ) ;
#13752 = CARTESIAN_POINT ( 'NONE',  ( -43.54501353716532464, -272.2127128057708774, -196.5567857530153617 ) ) ;
#13753 = CARTESIAN_POINT ( 'NONE',  ( -111.3382062549010101, -276.5211190551790992, -278.9317982136229261 ) ) ;
#13754 = CARTESIAN_POINT ( 'NONE',  ( -110.2275319208518169, -297.9959224510134277, -260.5473801730598780 ) ) ;
#13755 = CARTESIAN_POINT ( 'NONE',  ( 15.63170791097852685, -273.3589959267579843, -215.2936654122469804 ) ) ;
#13756 = CARTESIAN_POINT ( 'NONE',  ( -75.95188054528840382, -297.0036902640176208, -333.0673772392078718 ) ) ;
#13757 = DIRECTION ( 'NONE',  ( 0.000000000000000000, 1.000000000000000000, 0.000000000000000000 ) ) ;
#13758 = CARTESIAN_POINT ( 'NONE',  ( -106.1355369150969921, -297.0222443726284496, -295.4100190807086506 ) ) ;
#13759 = DIRECTION ( 'NONE',  ( -1.000000000000000000, 0.000000000000000000, 0.000000000000000000 ) ) ;
#13761 = CARTESIAN_POINT ( 'NONE',  ( -78.85332748939212877, -273.3088706031089714, -210.2515292568515690 ) ) ;
#13760 = CARTESIAN_POINT ( 'NONE',  ( 34.80321528886052818, -285.8518676814848618, -292.1663517381721249 ) ) ;
#13762 = CARTESIAN_POINT ( 'NONE',  ( -69.79283926952251704, -285.6365930307589451, -200.5189388990921771 ) ) ;
#13763 = CARTESIAN_POINT ( 'NONE',  ( 34.02113396979854087, -287.5870165811727475, -299.3663821283937523 ) ) ;
#13764 = CARTESIAN_POINT ( 'NONE',  ( -92.47689600519227326, -299.2481988400395494, -218.9184804145422731 ) ) ;
#13765 = CARTESIAN_POINT ( 'NONE',  ( -22.34903732883500993, -290.2444268882245524, -197.0450318511009584 ) ) ;
#13766 = CARTESIAN_POINT ( 'NONE',  ( -64.67530590450131456, -278.9014880006275234, -198.4925261815276656 ) ) ;
#13767 = CARTESIAN_POINT ( 'NONE',  ( -106.6662871844225293, -287.6237833571633473, -303.7098442033569654 ) ) ;
#13768 = CARTESIAN_POINT ( 'NONE',  ( 34.38730498677439584, -286.1429363136008419, -254.8021870629456487 ) ) ;
#13769 = CARTESIAN_POINT ( 'NONE',  ( 197.8754097859456635, 68.08024695722009767, -11.26651182472395085 ) ) ;
#13770 = CARTESIAN_POINT ( 'NONE',  ( -40.05533752652011259, -287.0859725880587803, -345.3629529728368084 ) ) ;
#13771 = CARTESIAN_POINT ( 'NONE',  ( -44.66856687509758217, -299.5581668526814951, -196.8747872970527624 ) ) ;
#13772 = CARTESIAN_POINT ( 'NONE',  ( -7.781824385329735527, -281.8572617504339632, -199.8854468587001350 ) ) ;
#13774 = CARTESIAN_POINT ( 'NONE',  ( 35.56592173907153409, -281.6005831265100028, -274.0324493046078373 ) ) ;
#13773 = CARTESIAN_POINT ( 'NONE',  ( -96.91773870222317555, -295.2019843947819027, -224.1981049282061065 ) ) ;
#13775 = CARTESIAN_POINT ( 'NONE',  ( -110.3450346168987579, -296.4105062578059346, -294.8460757733156470 ) ) ;
#13776 = CARTESIAN_POINT ( 'NONE',  ( -109.1135704158158291, -274.1901189571070745, -254.1077012780311293 ) ) ;
#13777 = CARTESIAN_POINT ( 'NONE',  ( -14.85239196843773612, -282.3435414664533596, -198.7578698140214044 ) ) ;
#13778 = CARTESIAN_POINT ( 'NONE',  ( -101.4146484076270269, -296.0941204872580101, -234.8918954609972616 ) ) ;
#13779 = EDGE_LOOP ( 'NONE', ( #53532, #17751, #83525, #68431 ) ) ;
#13780 = FACE_OUTER_BOUND ( 'NONE', #65492, .T. ) ;
#13781 = CARTESIAN_POINT ( 'NONE',  ( 23.15956195591534694, -284.1303887461084514, -314.1030776364909229 ) ) ;
#13782 = CARTESIAN_POINT ( 'NONE',  ( 189.9243309297870610, 250.0000000000000568, 15.22542485937351664 ) ) ;
#13783 = CARTESIAN_POINT ( 'NONE',  ( -95.95921662488163406, -294.6952119285919025, -223.5744983911110353 ) ) ;
#13784 = CARTESIAN_POINT ( 'NONE',  ( 38.33486201150012107, -274.5815416878353403, -256.9736004814580497 ) ) ;
#13785 = CARTESIAN_POINT ( 'NONE',  ( 22.58914744273794639, -292.8042727447717084, -228.6582391455953029 ) ) ;
#13786 = CARTESIAN_POINT ( 'NONE',  ( 15.74553495893989741, -282.3404799172340063, -219.1760779527031957 ) ) ;
#13787 = CARTESIAN_POINT ( 'NONE',  ( 36.40241823385852626, -277.2041500127876361, -274.3356198848738359 ) ) ;
#13788 = CARTESIAN_POINT ( 'NONE',  ( -108.7458018565789502, -285.6287319254290082, -297.7125166024455325 ) ) ;
#13789 = CARTESIAN_POINT ( 'NONE',  ( 29.33981347029352449, -279.9340937798414188, -239.5683264877759200 ) ) ;
#13790 = CARTESIAN_POINT ( 'NONE',  ( -111.2528157938226485, -280.3878400213831696, -283.1706004541239281 ) ) ;
#13791 = CARTESIAN_POINT ( 'NONE',  ( -34.04695977709405952, -298.0923358081694232, -193.3611179127478863 ) ) ;
#13792 = CARTESIAN_POINT ( 'NONE',  ( 21.72926089983860010, -276.0501701793031089, -319.7536434066195739 ) ) ;
#13793 = CARTESIAN_POINT ( 'NONE',  ( 31.93448154075495538, -295.8312016574400900, -297.7442376404128481 ) ) ;
#13794 = CARTESIAN_POINT ( 'NONE',  ( 222.4306832106270804, -135.2391364535880882, 21.50000000000000000 ) ) ;
#13795 = DIRECTION ( 'NONE',  ( -0.000000000000000000, -1.000000000000000000, -0.000000000000000000 ) ) ;
#13796 = CARTESIAN_POINT ( 'NONE',  ( -99.72003015995909436, -295.2690186796248781, -227.3354281492931648 ) ) ;
#13797 = CARTESIAN_POINT ( 'NONE',  ( 13.54400666820939314, -274.2961896977533911, -217.9337083058065616 ) ) ;
#13798 = CIRCLE ( 'NONE', #66712, 7.910944475430059519 ) ;
#13799 = CARTESIAN_POINT ( 'NONE',  ( 38.74823860038389967, -294.9997442242173520, -264.6140338863293096 ) ) ;
#13800 = CARTESIAN_POINT ( 'NONE',  ( 39.31426275336387732, -294.7563941697390533, -270.2949048963678251 ) ) ;
#13801 = CARTESIAN_POINT ( 'NONE',  ( 2.303917721861872714, -290.5198157394684131, -333.8296409751218903 ) ) ;
#13802 = CARTESIAN_POINT ( 'NONE',  ( -84.17343999460125303, -275.6971742504012468, -328.7957690127227579 ) ) ;
#13803 = CARTESIAN_POINT ( 'NONE',  ( 17.61036962121105631, -278.1788373003473112, -320.5955155483267163 ) ) ;
#13804 = CARTESIAN_POINT ( 'NONE',  ( -104.0696179844612885, -294.1920264653994082, -303.4731203355949560 ) ) ;
#13805 = CARTESIAN_POINT ( 'NONE',  ( 36.77136814797378150, -283.2117914317101395, -254.5651467127682395 ) ) ;
#13806 = CARTESIAN_POINT ( 'NONE',  ( -39.97129539926085329, -284.9386632195789275, -197.0991817329320099 ) ) ;
#13807 = CARTESIAN_POINT ( 'NONE',  ( 86.53115587608755277, 81.67541019969276306, -301.2104785531669791 ) ) ;
#13808 = ORIENTED_EDGE ( 'NONE', *, *, #54472, .F. ) ;
#13809 = CARTESIAN_POINT ( 'NONE',  ( -79.31797053866654323, -285.1350133261153132, -210.5488968255646967 ) ) ;
#13810 = CARTESIAN_POINT ( 'NONE',  ( -6.367867214589843172, -281.5292141867943201, -200.1891237866793460 ) ) ;
#13811 = CARTESIAN_POINT ( 'NONE',  ( -104.0786642346094908, -282.8553706178260541, -308.0742596360763628 ) ) ;
#13812 = CARTESIAN_POINT ( 'NONE',  ( -113.4853041314929101, -279.6207330724033113, -260.2108971320544697 ) ) ;
#13813 =( LENGTH_UNIT ( ) NAMED_UNIT ( * ) SI_UNIT ( .MILLI., .METRE. ) );
#13814 = CARTESIAN_POINT ( 'NONE',  ( -62.16200719779108397, -278.8891471615843898, -342.5741041693481748 ) ) ;
#13815 = CARTESIAN_POINT ( 'NONE',  ( 26.47324843497312585, -301.4082689599840705, -200.3320873922942553 ) ) ;
#13816 = CARTESIAN_POINT ( 'NONE',  ( 169.2043900173948714, 231.8925807357131248, -192.6779440976073090 ) ) ;
#13817 = ORIENTED_EDGE ( 'NONE', *, *, #63823, .T. ) ;
#13818 = CARTESIAN_POINT ( 'NONE',  ( -109.7196847477654273, -274.7995226233286417, -251.1501716192047127 ) ) ;
#13819 = CARTESIAN_POINT ( 'NONE',  ( -84.45682939641071130, -277.4204115232868730, -212.3976785749237877 ) ) ;
#13820 = CARTESIAN_POINT ( 'NONE',  ( -87.99094461473853812, -293.1151726275268175, -213.7163649639146570 ) ) ;
#13821 = CARTESIAN_POINT ( 'NONE',  ( 34.93748526230803719, -293.0491426060059439, -281.6268590439194099 ) ) ;
#13822 = CARTESIAN_POINT ( 'NONE',  ( -112.2042710200168045, -289.8369153488018242, -288.1691947544702543 ) ) ;
#13823 = DIRECTION ( 'NONE',  ( -0.000000000000000000, 1.000000000000000000, -0.000000000000000000 ) ) ;
#13825 = CARTESIAN_POINT ( 'NONE',  ( 9.554378471220637437, -285.1096934725891856, -213.3769252179830573 ) ) ;
#13824 = CARTESIAN_POINT ( 'NONE',  ( 6.262751130153954016, -293.0479373284229609, -333.1731531567143634 ) ) ;
#13826 = CARTESIAN_POINT ( 'NONE',  ( -19.80292938901446576, -294.1402999932092257, -198.1743629054663529 ) ) ;
#13827 = CARTESIAN_POINT ( 'NONE',  ( -7.960900414601150388, -284.9241031374633621, -202.7780109070870083 ) ) ;
#13828 = CARTESIAN_POINT ( 'NONE',  ( 3.679272258087318281, -283.8029257854306593, -331.4023813106707621 ) ) ;
#13829 = VERTEX_POINT ( 'NONE', #36919 ) ;
#13830 = CARTESIAN_POINT ( 'NONE',  ( -13.94959483957682878, -293.2895277274598129, -197.1915042597769911 ) ) ;
#13831 = CARTESIAN_POINT ( 'NONE',  ( 27.83345613268470231, -281.5952272979674831, -237.2309714127197822 ) ) ;
#13832 = CARTESIAN_POINT ( 'NONE',  ( 39.10475045691349294, -292.4182820575210258, -276.0251519761974350 ) ) ;
#13833 = CARTESIAN_POINT ( 'NONE',  ( -67.98007853865773598, -290.2471061334842375, -340.8270571961376163 ) ) ;
#13834 = CARTESIAN_POINT ( 'NONE',  ( -114.1895314914742556, -290.9977705905373000, -274.0944432849754548 ) ) ;
#13835 = CARTESIAN_POINT ( 'NONE',  ( 24.94961695304684923, -287.1944060393321365, -232.2981199294274006 ) ) ;
#13836 = ORIENTED_EDGE ( 'NONE', *, *, #56608, .T. ) ;
#13837 = CARTESIAN_POINT ( 'NONE',  ( 195.2230643128901022, 25.81418032658909567, 13.28579478226901678 ) ) ;
#13838 = CARTESIAN_POINT ( 'NONE',  ( 23.90202860175057609, -296.0144249183804277, -314.9869170896032529 ) ) ;
#13839 = CARTESIAN_POINT ( 'NONE',  ( -99.51098442883292705, -295.8317032346340056, -225.7710029013032909 ) ) ;
#13840 = CARTESIAN_POINT ( 'NONE',  ( -104.4919118862638356, -277.2176632504560985, -299.7159230139587294 ) ) ;
#13841 = ADVANCED_FACE ( 'NONE', ( #17475 ), #9647, .T. ) ;
#13842 = CARTESIAN_POINT ( 'NONE',  ( -105.5514804762074164, -272.5206439725981795, -234.6517084826563462 ) ) ;
#13843 = CARTESIAN_POINT ( 'NONE',  ( -68.83101988011340211, -293.9536470956139169, -337.0017811404400163 ) ) ;
#13844 = CARTESIAN_POINT ( 'NONE',  ( 29.99884081982527562, -276.9024110634111935, -239.5252425068507023 ) ) ;
#13845 = CARTESIAN_POINT ( 'NONE',  ( -51.77887032122603728, -272.0052037540064021, -197.4906445287676320 ) ) ;
#13846 = CARTESIAN_POINT ( 'NONE',  ( 17.38683348229893966, -295.4532116487959001, -319.2873114987274334 ) ) ;
#13847 = CARTESIAN_POINT ( 'NONE',  ( -53.20291669239951204, -296.3398828731852177, -341.9859963003457892 ) ) ;
#13848 = CARTESIAN_POINT ( 'NONE',  ( -43.37481164453355120, -265.5671965738019367, -435.3290497496450371 ) ) ;
#13849 = CARTESIAN_POINT ( 'NONE',  ( -110.8185687409976055, -294.3489524106902309, -286.2097207507188728 ) ) ;
#13850 = CARTESIAN_POINT ( 'NONE',  ( -112.2880544601896702, -273.5673719416994913, -253.4140594250813763 ) ) ;
#13851 = CARTESIAN_POINT ( 'NONE',  ( 23.22462044429903116, -286.7046300548752811, -312.1815962561309448 ) ) ;
#13852 = CARTESIAN_POINT ( 'NONE',  ( -35.36239268324980145, -276.0771255025746882, -195.3743876976912475 ) ) ;
#13853 = CARTESIAN_POINT ( 'NONE',  ( -97.76863161707223071, -273.6819678508643392, -222.7364095383559857 ) ) ;
#13854 = CARTESIAN_POINT ( 'NONE',  ( -106.8881074978329480, -296.5884060691602144, -292.7820167008665067 ) ) ;
#13855 = CARTESIAN_POINT ( 'NONE',  ( -91.90067697950352965, -281.2588173906169686, -218.3084166985720458 ) ) ;
#13856 = CARTESIAN_POINT ( 'NONE',  ( -22.64440197356533346, -278.9211762468011671, -195.2253347856420760 ) ) ;
#13857 = CARTESIAN_POINT ( 'NONE',  ( -18.95082437226056271, -282.1701406969540926, -345.0825166320857988 ) ) ;
#13858 = CARTESIAN_POINT ( 'NONE',  ( 39.45306623616082931, -274.8392956770359206, -265.4545597158873420 ) ) ;
#13859 = CARTESIAN_POINT ( 'NONE',  ( 35.83720117554236850, -279.6823015463204456, -249.0707367076533671 ) ) ;
#13860 = CARTESIAN_POINT ( 'NONE',  ( -35.35825355495023103, -278.0768060958984620, -195.2077966996185694 ) ) ;
#13861 = EDGE_CURVE ( 'NONE', #6353, #34447, #10343, .T. ) ;
#13862 = CARTESIAN_POINT ( 'NONE',  ( 5.534673921256747953, -273.2199133480867772, -210.4901708934459066 ) ) ;
#13863 = CARTESIAN_POINT ( 'NONE',  ( 35.69911773042250047, -277.3329289820165400, -253.2753318245520404 ) ) ;
#13864 = CARTESIAN_POINT ( 'NONE',  ( 154.7659666677267580, 19.56018909072084355, 12.94946946941271193 ) ) ;
#13865 = CARTESIAN_POINT ( 'NONE',  ( -55.76179165756899181, -289.8364141939027832, -197.2381553244462395 ) ) ;
#13866 = CIRCLE ( 'NONE', #66772, 1.000000000000000888 ) ;
#13867 = CARTESIAN_POINT ( 'NONE',  ( -97.46356613883708064, -291.1965560023747344, -222.2533095998791737 ) ) ;
#13868 = EDGE_CURVE ( 'NONE', #10254, #49342, #9407, .T. ) ;
#13869 = CARTESIAN_POINT ( 'NONE',  ( -28.78385074413047917, -278.9441809993283528, -345.0913384605607916 ) ) ;
#13870 = CARTESIAN_POINT ( 'NONE',  ( -35.31133640963481923, -272.0774514690457977, -195.3757535277878503 ) ) ;
#13871 = CARTESIAN_POINT ( 'NONE',  ( -43.18343439339132317, -291.0521521680024080, -430.6442049081568939 ) ) ;
#13872 = AXIS2_PLACEMENT_3D ( 'NONE', #69873, #11171, #24921 ) ;
#13873 = CARTESIAN_POINT ( 'NONE',  ( -63.12829348636812909, -283.7162859271044795, -199.8789987046618535 ) ) ;
#13874 = DIRECTION ( 'NONE',  ( -0.000000000000000000, -0.000000000000000000, -1.000000000000000000 ) ) ;
#13875 = CARTESIAN_POINT ( 'NONE',  ( -9.092159207519776132, -293.4692550630706478, -338.1176480249738461 ) ) ;
#13876 = CARTESIAN_POINT ( 'NONE',  ( 34.89770183830172812, -285.9135452394748427, -287.4589040187652813 ) ) ;
#13877 = CARTESIAN_POINT ( 'NONE',  ( 196.4665495134686353, 24.53799251391352954, 13.19633711769627382 ) ) ;
#13878 = FACE_OUTER_BOUND ( 'NONE', #24335, .T. ) ;
#13879 = CARTESIAN_POINT ( 'NONE',  ( -69.39460006631520628, -293.4736863239355102, -338.1809221109065220 ) ) ;
#13880 = CARTESIAN_POINT ( 'NONE',  ( -112.9155006348995727, -282.8941703488339385, -281.2852848898040747 ) ) ;
#13881 = CARTESIAN_POINT ( 'NONE',  ( -108.3940014747174985, -280.4136804977609927, -250.3640227833301992 ) ) ;
#13882 = CARTESIAN_POINT ( 'NONE',  ( -97.27935688356468802, -286.3991526854563858, -222.6590632746684832 ) ) ;
#13883 = CARTESIAN_POINT ( 'NONE',  ( 37.26409516417955103, -279.6092633698817167, -255.9406698379628153 ) ) ;
#13884 = CARTESIAN_POINT ( 'NONE',  ( 32.66996914282456999, -287.2780763744044066, -249.6441852604225744 ) ) ;
#13885 = CARTESIAN_POINT ( 'NONE',  ( -76.65538895197525449, -279.0144663504079290, -332.6288273084067555 ) ) ;
#13886 = CARTESIAN_POINT ( 'NONE',  ( -94.57297022161840516, -278.7125370842812231, -315.9572539577405337 ) ) ;
#13887 = CARTESIAN_POINT ( 'NONE',  ( -35.22035727339236644, -288.0585190858773785, -195.0229159501386107 ) ) ;
#13888 = ORIENTED_EDGE ( 'NONE', *, *, #77208, .F. ) ;
#13889 = CARTESIAN_POINT ( 'NONE',  ( -35.46978037339534495, -297.9083036264289035, -193.3611691524987179 ) ) ;
#13890 = CARTESIAN_POINT ( 'NONE',  ( -10.10086472495352083, -290.6748046522712912, -339.9132089729552604 ) ) ;
#13891 = CARTESIAN_POINT ( 'NONE',  ( 133.0872704186301405, -299.5541904835127980, -202.0153591320744226 ) ) ;
#13892 = CARTESIAN_POINT ( 'NONE',  ( -19.05039376806008633, -285.3376638359844719, -350.3538533559490702 ) ) ;
#13893 = ORIENTED_EDGE ( 'NONE', *, *, #76503, .F. ) ;
#13894 = CARTESIAN_POINT ( 'NONE',  ( 28.35779963562260875, -273.0658602049711590, -233.7354773566951565 ) ) ;
#13895 = CARTESIAN_POINT ( 'NONE',  ( 20.71430914698659720, -291.2794607579100443, -220.9859322173466580 ) ) ;
#13896 = CARTESIAN_POINT ( 'NONE',  ( -102.8260960304365597, -295.6196035908107547, -302.8758095803309516 ) ) ;
#13897 = CARTESIAN_POINT ( 'NONE',  ( -37.29973151637383211, -287.5727738013668500, -196.6552370485001973 ) ) ;
#13898 = CARTESIAN_POINT ( 'NONE',  ( 22.13002728783479967, -282.7027397504519399, -226.2820191376268326 ) ) ;
#13899 = CARTESIAN_POINT ( 'NONE',  ( -29.02314814989797043, -290.3740885136897418, -346.3708543099326107 ) ) ;
#13900 = CARTESIAN_POINT ( 'NONE',  ( -84.84528372748631853, -291.0064737556717773, -330.4012583873403628 ) ) ;
#13901 = CARTESIAN_POINT ( 'NONE',  ( -100.7075165172649207, -286.0114868524486837, -310.5802809824875226 ) ) ;
#13902 = CARTESIAN_POINT ( 'NONE',  ( -51.31053502479835515, -277.3927069767499916, -346.0834505939782844 ) ) ;
#13903 = ORIENTED_EDGE ( 'NONE', *, *, #36821, .F. ) ;
#13904 = CARTESIAN_POINT ( 'NONE',  ( -61.16125358079393237, -293.4387307106679827, -342.1231647293279252 ) ) ;
#13905 = CARTESIAN_POINT ( 'NONE',  ( 39.18302242493180643, -281.2728021034162680, -261.3520736238132827 ) ) ;
#13906 = CARTESIAN_POINT ( 'NONE',  ( -109.7447831794055588, -274.6251921393022712, -253.9702958932091974 ) ) ;
#13907 = CARTESIAN_POINT ( 'NONE',  ( -85.28047601435908120, -292.1948066931273615, -330.5268031993605859 ) ) ;
#13908 = CARTESIAN_POINT ( 'NONE',  ( 28.21030407220004577, -274.2989388077428998, -308.7916885913560350 ) ) ;
#13909 = CARTESIAN_POINT ( 'NONE',  ( 156.4851178187871312, 0.000000000000000000, 10.00000000000000000 ) ) ;
#13910 = CARTESIAN_POINT ( 'NONE',  ( 11.35149465784171774, -280.2568112751799276, -215.8912986048921994 ) ) ;
#13911 = CARTESIAN_POINT ( 'NONE',  ( -17.44616398114765587, -278.0060325726952328, -344.3352780585476012 ) ) ;
#13912 = CARTESIAN_POINT ( 'NONE',  ( -104.2619236311069102, -298.3884015333197794, -239.6269870349098312 ) ) ;
#13913 = CARTESIAN_POINT ( 'NONE',  ( -63.84206929732978608, -282.4481810269372772, -342.4065942226606580 ) ) ;
#13914 = CARTESIAN_POINT ( 'NONE',  ( -91.31659424574539230, -291.5927785683759339, -321.0786537339303663 ) ) ;
#13915 = CARTESIAN_POINT ( 'NONE',  ( -65.94601730740606627, -275.2842163509899933, -199.7196661012601453 ) ) ;
#13916 = CARTESIAN_POINT ( 'NONE',  ( -111.3456117824015053, -274.1141762646116717, -250.7489374756198686 ) ) ;
#13917 = FACE_OUTER_BOUND ( 'NONE', #47419, .T. ) ;
#13918 = CARTESIAN_POINT ( 'NONE',  ( 31.17870385544242851, -295.9470949751941475, -300.4440477184514293 ) ) ;
#13919 = CARTESIAN_POINT ( 'NONE',  ( -32.04062742820021725, -280.9849457042334393, -345.0064598027554439 ) ) ;
#13920 = CARTESIAN_POINT ( 'NONE',  ( -112.2431038817852880, -289.9959555951043626, -288.1805269029781016 ) ) ;
#13921 = CARTESIAN_POINT ( 'NONE',  ( 34.08306152892657082, -273.8536245856207074, -292.0929357077902750 ) ) ;
#13922 = CARTESIAN_POINT ( 'NONE',  ( 30.69822059083624310, -288.7061592649998829, -236.0535444457762821 ) ) ;
#13923 = CARTESIAN_POINT ( 'NONE',  ( -108.4047378986518595, -289.7097502756898848, -252.3025838715099383 ) ) ;
#13924 = VERTEX_POINT ( 'NONE', #8943 ) ;
#13925 = CARTESIAN_POINT ( 'NONE',  ( -99.40238966083316541, -288.5312595766996537, -314.9601852023115498 ) ) ;
#13926 = CARTESIAN_POINT ( 'NONE',  ( -72.63344644033401210, -291.2382316069362105, -206.3779344886439731 ) ) ;
#13927 = ORIENTED_EDGE ( 'NONE', *, *, #35541, .F. ) ;
#13928 = CARTESIAN_POINT ( 'NONE',  ( 22.17399736623949735, -289.2835070508272111, -318.7488687464811505 ) ) ;
#13929 = CARTESIAN_POINT ( 'NONE',  ( 19.20066113503581917, -276.5396825521901860, -316.5874120009416970 ) ) ;
#13930 = EDGE_CURVE ( 'NONE', #74899, #42552, #73209, .T. ) ;
#13931 = CARTESIAN_POINT ( 'NONE',  ( -71.94690938237734201, -294.4192572883148387, -338.8006679767718197 ) ) ;
#13932 = CARTESIAN_POINT ( 'NONE',  ( -102.8269252101145383, -284.6759829311966996, -310.6723829387304932 ) ) ;
#13933 = CARTESIAN_POINT ( 'NONE',  ( -107.9084469141536715, -285.2791603305217905, -239.4694301635275338 ) ) ;
#13934 = CARTESIAN_POINT ( 'NONE',  ( 34.50701660207009525, -282.0582311665448856, -283.4638320346683713 ) ) ;
#13935 = CARTESIAN_POINT ( 'NONE',  ( 45.02227103420001697, 12.57429608517253961, -332.0372542094538062 ) ) ;
#13936 = AXIS2_PLACEMENT_3D ( 'NONE', #5100, #46753, #75654 ) ;
#13937 = CARTESIAN_POINT ( 'NONE',  ( 192.8964254566477905, 279.1718055284784441, -125.5694871102472376 ) ) ;
#13938 = CARTESIAN_POINT ( 'NONE',  ( -22.61259601301798483, -108.4505377025144242, -359.0006681345822130 ) ) ;
#13939 =( GEOMETRIC_REPRESENTATION_CONTEXT ( 3 ) GLOBAL_UNCERTAINTY_ASSIGNED_CONTEXT ( ( #39591 ) ) GLOBAL_UNIT_ASSIGNED_CONTEXT ( ( #78729, #64089, #43208 ) ) REPRESENTATION_CONTEXT ( 'NONE', 'WORKASPACE' ) );
#13940 = CARTESIAN_POINT ( 'NONE',  ( -92.13232101574408262, -272.4405000909766272, -221.8782386332586043 ) ) ;
#13941 = CARTESIAN_POINT ( 'NONE',  ( -48.91071740801071854, -272.8217788585934613, -197.9192328261104876 ) ) ;
#13942 = CARTESIAN_POINT ( 'NONE',  ( -70.78679458155451698, -294.9891162679484751, -339.6645234084620597 ) ) ;
#13943 = CARTESIAN_POINT ( 'NONE',  ( -87.79732207361467999, -230.1314203361037301, -344.7605846467396304 ) ) ;
#13944 = CARTESIAN_POINT ( 'NONE',  ( -31.28231389223850556, -272.8119750995933259, -194.0814013717944988 ) ) ;
#13945 = CARTESIAN_POINT ( 'NONE',  ( -109.6860279954746602, -298.6285320421354186, -253.7128835571040781 ) ) ;
#13946 = CARTESIAN_POINT ( 'NONE',  ( 12.50248238604651796, -289.6556378521762554, -324.4377017862967705 ) ) ;
#13947 = CARTESIAN_POINT ( 'NONE',  ( -102.6913282385188637, -292.0824498205961959, -237.0274441948036781 ) ) ;
#13948 = ORIENTED_EDGE ( 'NONE', *, *, #55276, .T. ) ;
#13949 = CARTESIAN_POINT ( 'NONE',  ( -102.9083715996914492, -296.9704828890004364, -310.2839410876592297 ) ) ;
#13950 = AXIS2_PLACEMENT_3D ( 'NONE', #53569, #17592, #46442 ) ;
#13951 = CARTESIAN_POINT ( 'NONE',  ( 15.06927833456615851, -287.3091378701336680, -219.4584876160160150 ) ) ;
#13952 = CARTESIAN_POINT ( 'NONE',  ( 29.43940176766727745, -294.8507760003695921, -308.4744588754392680 ) ) ;
#13953 = CARTESIAN_POINT ( 'NONE',  ( -34.85035099077237675, -295.5139837230917692, -347.2592329327564471 ) ) ;
#13954 = CARTESIAN_POINT ( 'NONE',  ( -1.258522564495346163, -292.7117813842300507, -206.8879610891251843 ) ) ;
#13955 = ORIENTED_EDGE ( 'NONE', *, *, #89206, .T. ) ;
#13956 = CARTESIAN_POINT ( 'NONE',  ( -16.20408140379166895, -276.2433481790006908, -197.7636239889024523 ) ) ;
#13957 = EDGE_LOOP ( 'NONE', ( #26923, #89803, #1303, #27076 ) ) ;
#13958 = EDGE_CURVE ( 'NONE', #46065, #29052, #74684, .T. ) ;
#13959 = CARTESIAN_POINT ( 'NONE',  ( -114.3234301369553805, -278.0442852626783292, -271.6011420763450133 ) ) ;
#13960 = CARTESIAN_POINT ( 'NONE',  ( 34.94408123618173789, -274.1460942670458962, -285.2341213691066741 ) ) ;
#13961 = CARTESIAN_POINT ( 'NONE',  ( 24.18856565479102017, -277.0425723235796909, -310.1715809883531847 ) ) ;
#13962 = CARTESIAN_POINT ( 'NONE',  ( -49.57844098909943398, -275.6584560164728259, -195.3131111677384126 ) ) ;
#13963 = CARTESIAN_POINT ( 'NONE',  ( 27.66404565220688738, -274.0792232336564211, -308.4748926090412056 ) ) ;
#13964 = CARTESIAN_POINT ( 'NONE',  ( -44.58743185363938011, -298.6096046369905253, -197.5687104263188587 ) ) ;
#13965 = CARTESIAN_POINT ( 'NONE',  ( -38.36857645374530534, -293.6399992249069442, -343.9431840307071298 ) ) ;
#13966 = CARTESIAN_POINT ( 'NONE',  ( 200.7568414405312467, 39.78480925505071752, 10.50000000000000000 ) ) ;
#13967 = CARTESIAN_POINT ( 'NONE',  ( -98.75051561006894474, -278.4264690647755174, -316.7344837930183417 ) ) ;
#13968 = CARTESIAN_POINT ( 'NONE',  ( 17.43663486931767181, -276.4080388961909307, -318.6327903016679102 ) ) ;
#13969 = CARTESIAN_POINT ( 'NONE',  ( -40.77745235512595912, -284.6947503035688101, -193.8795922955957565 ) ) ;
#13970 = CARTESIAN_POINT ( 'NONE',  ( -56.93693582120787511, -299.8003121437577647, -197.7395603548327756 ) ) ;
#13971 = CARTESIAN_POINT ( 'NONE',  ( 82.63805641362395704, -300.4059824324262422, -197.7175201709814019 ) ) ;
#13972 = CARTESIAN_POINT ( 'NONE',  ( 23.63845033345183566, -287.3092787066311189, -310.8070461044287072 ) ) ;
#13973 = EDGE_CURVE ( 'NONE', #65891, #35945, #89799, .T. ) ;
#13974 = CARTESIAN_POINT ( 'NONE',  ( -72.59287493551462944, -277.8185007445991346, -205.2817150226913725 ) ) ;
#13975 = CARTESIAN_POINT ( 'NONE',  ( -49.21928027160467423, -278.4725296819978553, -197.7367556394873986 ) ) ;
#13976 = CARTESIAN_POINT ( 'NONE',  ( -110.5803792769081042, -286.3441510188929442, -286.5777818089525226 ) ) ;
#13977 = CARTESIAN_POINT ( 'NONE',  ( -21.55272684444882714, -278.0504086211623758, -342.0921152256848359 ) ) ;
#13978 = DIRECTION ( 'NONE',  ( 0.8435586647355767242, 0.000000000000000000, -0.5370370370370473045 ) ) ;
#13979 = CARTESIAN_POINT ( 'NONE',  ( 36.86060554855468041, -273.7323197756792865, -252.9705596984334477 ) ) ;
#13980 = CARTESIAN_POINT ( 'NONE',  ( 32.95574599036767438, -275.9366329000378641, -250.1263459734549599 ) ) ;
#13981 = CARTESIAN_POINT ( 'NONE',  ( 36.86219651193465552, -283.7069798689504978, -282.4337731464697754 ) ) ;
#13982 = CARTESIAN_POINT ( 'NONE',  ( 73.43068321062709458, -178.2391364535880882, 0.000000000000000000 ) ) ;
#13983 = CARTESIAN_POINT ( 'NONE',  ( 19.50596705572998601, -290.1586888761673890, -320.1566857630890013 ) ) ;
#13984 = CARTESIAN_POINT ( 'NONE',  ( 28.68944520935930242, -292.0253808842684862, -306.0345839285895408 ) ) ;
#13985 = DIRECTION ( 'NONE',  ( 0.000000000000000000, 0.000000000000000000, 1.000000000000000000 ) ) ;
#13986 = CARTESIAN_POINT ( 'NONE',  ( -40.78136994951938732, -272.6929447662913049, -196.8984651037467870 ) ) ;
#13987 = CARTESIAN_POINT ( 'NONE',  ( 35.53248676140506745, -291.8752888915151971, -284.5109719674903204 ) ) ;
#13988 = CARTESIAN_POINT ( 'NONE',  ( 121.1498776811041438, 150.0802918209077177, -263.8330885344481658 ) ) ;
#13989 = DIRECTION ( 'NONE',  ( 0.000000000000000000, 0.000000000000000000, 1.000000000000000000 ) ) ;
#13990 = CARTESIAN_POINT ( 'NONE',  ( -43.14901327210228033, -287.6041061774054697, -346.4464836372922036 ) ) ;
#13991 = CARTESIAN_POINT ( 'NONE',  ( -5.182169578036499580, -284.7094993623931600, -201.5153584037910264 ) ) ;
#13992 = CARTESIAN_POINT ( 'NONE',  ( -18.56793586405532182, -284.2309807281924350, -341.5681525110846906 ) ) ;
#13993 = EDGE_CURVE ( 'NONE', #90518, #43675, #64190, .T. ) ;
#13994 = CARTESIAN_POINT ( 'NONE',  ( -101.9089367386394258, -284.8858792272508254, -304.8734732437175694 ) ) ;
#13995 = CARTESIAN_POINT ( 'NONE',  ( -76.34009215513137292, -293.5137774700590398, -205.8220001725522366 ) ) ;
#13996 = CARTESIAN_POINT ( 'NONE',  ( 35.21022174696152263, -273.3601485704849665, -249.0704178336520442 ) ) ;
#13997 = AXIS2_PLACEMENT_3D ( 'NONE', #6390, #21057, #20601 ) ;
#13998 = CARTESIAN_POINT ( 'NONE',  ( 21.83188142953161659, -275.2230080161028241, -221.1246321486615614 ) ) ;
#13999 = CIRCLE ( 'NONE', #75954, 0.9999999999999980016 ) ;
#14000 = CARTESIAN_POINT ( 'NONE',  ( -103.8993110872538495, -288.1607531927754167, -306.1298000775723267 ) ) ;
#14001 = CARTESIAN_POINT ( 'NONE',  ( -70.30101726200295786, -277.4745387684100706, -339.9649469544103795 ) ) ;
#14002 = CARTESIAN_POINT ( 'NONE',  ( 35.94392880358793008, -295.7149761097521150, -284.5408005424354769 ) ) ;
#14003 = CARTESIAN_POINT ( 'NONE',  ( -48.18343439339130896, -259.5409938266968197, -446.9856792133138583 ) ) ;
#14004 = CARTESIAN_POINT ( 'NONE',  ( 209.5276096738287777, 37.00211571918214304, 12.90116063919866995 ) ) ;
#14005 = CARTESIAN_POINT ( 'NONE',  ( -110.8840263982265242, -283.2299583353841399, -270.8962879372326711 ) ) ;
#14006 = CARTESIAN_POINT ( 'NONE',  ( -96.97035648470519220, -277.1748693203211928, -224.8492839413438560 ) ) ;
#14007 = CARTESIAN_POINT ( 'NONE',  ( 52.43474621377098543, -297.5582050755576233, -194.1850537549212561 ) ) ;
#14008 = CARTESIAN_POINT ( 'NONE',  ( -41.87117731851381564, -276.4592829566884689, -343.3352047031388565 ) ) ;
#14009 = AXIS2_PLACEMENT_3D ( 'NONE', #83090, #24404, #81232 ) ;
#14010 = CARTESIAN_POINT ( 'NONE',  ( -19.92691529862905853, -293.8000607818966046, -198.7022591221019070 ) ) ;
#14011 = CARTESIAN_POINT ( 'NONE',  ( 18.64875676080346523, -293.8248532635283254, -223.1543686121119379 ) ) ;
#14012 = CARTESIAN_POINT ( 'NONE',  ( -55.93412788960144866, -296.6019039335914158, -344.5744584367828907 ) ) ;
#14013 = CARTESIAN_POINT ( 'NONE',  ( -97.18459369217598010, -295.8025314269007708, -312.1681520126081182 ) ) ;
#14014 = CARTESIAN_POINT ( 'NONE',  ( -4.905012468922741675, -290.6251904419686980, -337.9840574882693431 ) ) ;
#14015 = CARTESIAN_POINT ( 'NONE',  ( -107.0047416322343992, -284.2986503617667040, -303.1644814210063714 ) ) ;
#14016 = CARTESIAN_POINT ( 'NONE',  ( -16.10057293618129748, -272.4633867731518535, -197.5803246476255026 ) ) ;
#14017 = CARTESIAN_POINT ( 'NONE',  ( 31.42274725833685878, -286.9396351998213959, -235.7135959914429861 ) ) ;
#14018 = CARTESIAN_POINT ( 'NONE',  ( -110.0835700105092627, -280.3152574682040381, -287.1648363960576376 ) ) ;
#14019 = CARTESIAN_POINT ( 'NONE',  ( -79.43475759041217543, -284.5271403797784728, -210.3690505390151486 ) ) ;
#14020 = CARTESIAN_POINT ( 'NONE',  ( -86.10395804379319884, -287.7276120369754722, -327.4139369828311033 ) ) ;
#14021 = CARTESIAN_POINT ( 'NONE',  ( 201.7648208617462728, 289.3015991269851384, -82.29596988341933184 ) ) ;
#14022 = CARTESIAN_POINT ( 'NONE',  ( -19.79501048500039673, -285.7915498532761376, -199.4379051109754641 ) ) ;
#14023 = CARTESIAN_POINT ( 'NONE',  ( -21.76199643385749027, -283.7984002363313607, -345.5282187985935707 ) ) ;
#14024 = CARTESIAN_POINT ( 'NONE',  ( -95.47486193030424317, -290.2901610347151404, -220.2076508610878989 ) ) ;
#14025 = CARTESIAN_POINT ( 'NONE',  ( -72.15963582219853834, -281.1995835920613445, -202.5664448791465588 ) ) ;
#14026 = CARTESIAN_POINT ( 'NONE',  ( -113.8912042552325374, -279.8515156087285050, -271.6171234615896424 ) ) ;
#14027 = CARTESIAN_POINT ( 'NONE',  ( 30.33373449885391793, -281.7519745318558080, -297.7296318724862658 ) ) ;
#14028 = CARTESIAN_POINT ( 'NONE',  ( -63.91532113618128363, -275.6838174916088633, -200.5928241190977985 ) ) ;
#14029 = CARTESIAN_POINT ( 'NONE',  ( -3.228783570963782878, -294.6141346856778682, -339.4069389610562553 ) ) ;
#14030 = CARTESIAN_POINT ( 'NONE',  ( -51.07834888656000061, -287.2485352606307174, -343.7839262310250774 ) ) ;
#14031 = CARTESIAN_POINT ( 'NONE',  ( -86.01782091859632828, -292.9909627607779612, -211.6660119433807949 ) ) ;
#14032 = CARTESIAN_POINT ( 'NONE',  ( -95.85934710826388994, -294.8545690630814988, -314.5395992957853650 ) ) ;
#14033 = ORIENTED_EDGE ( 'NONE', *, *, #22733, .F. ) ;
#14034 = CARTESIAN_POINT ( 'NONE',  ( 16.89142717854064557, -284.1928122744155871, -321.4265136511351102 ) ) ;
#14035 = CARTESIAN_POINT ( 'NONE',  ( -92.20936670838629823, -295.5312630572193484, -318.5443790890765285 ) ) ;
#14036 = CARTESIAN_POINT ( 'NONE',  ( -3.470313686029046885, -293.5684616275291319, -201.5409595524095892 ) ) ;
#14037 = CARTESIAN_POINT ( 'NONE',  ( -3.108692801777531045, -281.1683720528533286, -205.7559474921650065 ) ) ;
#14038 = CARTESIAN_POINT ( 'NONE',  ( -67.43233360154476941, -272.7257408847764850, -199.7397756663388009 ) ) ;
#14039 = CARTESIAN_POINT ( 'NONE',  ( -85.09487544735820563, -290.3428197588968942, -330.7029841899748703 ) ) ;
#14040 = CARTESIAN_POINT ( 'NONE',  ( 1.441180044896873902, -280.6792731409850035, -335.4471663006981998 ) ) ;
#14041 = CARTESIAN_POINT ( 'NONE',  ( -100.0163013263131973, -291.4775725279130256, -225.6661668560507792 ) ) ;
#14042 = CARTESIAN_POINT ( 'NONE',  ( -0.9772292964629729628, -288.8887809096349315, -333.7416143040517795 ) ) ;
#14043 = DIRECTION ( 'NONE',  ( 0.000000000000000000, -0.000000000000000000, 1.000000000000000000 ) ) ;
#14044 = CARTESIAN_POINT ( 'NONE',  ( 154.7659666677267580, 20.47222690886501439, -12.53936336329525858 ) ) ;
#14045 = CARTESIAN_POINT ( 'NONE',  ( 45.42119675738224061, 10.99673322031138412, -328.3769721457455830 ) ) ;
#14046 = CARTESIAN_POINT ( 'NONE',  ( 90.38368222445549804, -297.2649936051623740, -200.4191791630918829 ) ) ;
#14047 = CARTESIAN_POINT ( 'NONE',  ( -108.6459449522204466, -277.5329834346950975, -286.7967320428482481 ) ) ;
#14048 = ORIENTED_EDGE ( 'NONE', *, *, #22221, .T. ) ;
#14049 = CARTESIAN_POINT ( 'NONE',  ( -24.81008966536818861, -279.1361170996223677, -198.1310355237392002 ) ) ;
#14050 = CARTESIAN_POINT ( 'NONE',  ( 39.60208087879163941, -275.2649837109509008, -274.0471857123279165 ) ) ;
#14051 = CARTESIAN_POINT ( 'NONE',  ( 204.1739257889963426, 292.3637011233957992, -68.35704339179807221 ) ) ;
#14052 = CARTESIAN_POINT ( 'NONE',  ( -48.01835787157568802, -278.4937470192833757, -194.6464996853970604 ) ) ;
#14053 = CARTESIAN_POINT ( 'NONE',  ( -6.598580490294386536, -280.6666100292207489, -338.3950424086135058 ) ) ;
#14054 = CARTESIAN_POINT ( 'NONE',  ( -113.2978551945238195, -298.3573562008087379, -266.8053500766753814 ) ) ;
#14055 = CARTESIAN_POINT ( 'NONE',  ( 22.63486968089157259, -293.4631935817392900, -228.6161875331386568 ) ) ;
#14056 = ORIENTED_EDGE ( 'NONE', *, *, #92749, .F. ) ;
#14057 = CARTESIAN_POINT ( 'NONE',  ( -58.84933899805359658, -288.0209495837702889, -340.6899185866644757 ) ) ;
#14058 = CARTESIAN_POINT ( 'NONE',  ( 38.62561297402739058, -276.0531253393550060, -258.3481752850842668 ) ) ;
#14059 = CARTESIAN_POINT ( 'NONE',  ( -34.48206726786463605, -298.2556126639216245, -197.3610342856659372 ) ) ;
#14060 = ORIENTED_EDGE ( 'NONE', *, *, #65309, .F. ) ;
#14061 = LINE ( 'NONE', #34435, #20515 ) ;
#14062 = LINE ( 'NONE', #13597, #27962 ) ;
#14063 = AXIS2_PLACEMENT_3D ( 'NONE', #92083, #70802, #20130 ) ;
#14064 = CARTESIAN_POINT ( 'NONE',  ( 154.9307753191124846, 19.94580804509840277, 10.40578999957047479 ) ) ;
#14065 = AXIS2_PLACEMENT_3D ( 'NONE', #61468, #82283, #60994 ) ;
#14066 = CARTESIAN_POINT ( 'NONE',  ( -74.67499940345929588, -280.6227553722633843, -207.2119506859932017 ) ) ;
#14067 = CARTESIAN_POINT ( 'NONE',  ( -7.949922215315155860, -282.1920765836794089, -200.2749179418074732 ) ) ;
#14068 = CARTESIAN_POINT ( 'NONE',  ( -104.3333517805514816, -283.2139805525881115, -299.9504244342596735 ) ) ;
#14069 = CARTESIAN_POINT ( 'NONE',  ( -52.09564324425033277, -281.7218604765699865, -197.5542197944056966 ) ) ;
#14070 = CARTESIAN_POINT ( 'NONE',  ( 19.70614025917264556, -274.6865793893451269, -317.0313084605385257 ) ) ;
#14072 = DIRECTION ( 'NONE',  ( 0.000000000000000000, -0.000000000000000000, 1.000000000000000000 ) ) ;
#14071 = VECTOR ( 'NONE', #11875, 1000.000000000000114 ) ;
#14073 = DIRECTION ( 'NONE',  ( -0.000000000000000000, -0.000000000000000000, -1.000000000000000000 ) ) ;
#14074 = VECTOR ( 'NONE', #31465, 1000.000000000000000 ) ;
#14075 = CARTESIAN_POINT ( 'NONE',  ( -11.90996338542509037, -277.5323247366557666, -342.9247617639934447 ) ) ;
#14076 = DIRECTION ( 'NONE',  ( -0.000000000000000000, -1.000000000000000000, -0.000000000000000000 ) ) ;
#14077 = CARTESIAN_POINT ( 'NONE',  ( -28.68594959952024226, -275.5193002513117335, -346.3332146333099217 ) ) ;
#14078 = ORIENTED_EDGE ( 'NONE', *, *, #37019, .F. ) ;
#14079 = DIRECTION ( 'NONE',  ( -0.000000000000000000, -1.000000000000000000, -0.000000000000000000 ) ) ;
#14080 = CARTESIAN_POINT ( 'NONE',  ( -109.9007486375338374, -286.2716373934872536, -290.6980618046380869 ) ) ;
#14081 = AXIS2_PLACEMENT_3D ( 'NONE', #56497, #62182, #83462 ) ;
#14082 = CARTESIAN_POINT ( 'NONE',  ( 21.45014514778553405, -293.3585230118524692, -313.9055855579143213 ) ) ;
#14083 = CARTESIAN_POINT ( 'NONE',  ( 39.24518048515181334, -286.9872872705570899, -277.2721601839047594 ) ) ;
#14084 = CARTESIAN_POINT ( 'NONE',  ( -111.0005955772205510, -282.8926971637777115, -262.6221195037292659 ) ) ;
#14086 = CARTESIAN_POINT ( 'NONE',  ( -70.44555980785480642, -287.7345165263075160, -336.5726681701117968 ) ) ;
#14085 = CARTESIAN_POINT ( 'NONE',  ( -54.87931107184501656, -284.3971077231576032, -198.8394768870798828 ) ) ;
#14087 = CARTESIAN_POINT ( 'NONE',  ( -7.075795367499152277, -283.8510627892477487, -337.2412334445056672 ) ) ;
#14088 = CARTESIAN_POINT ( 'NONE',  ( -34.16181914077959192, -272.0919910481815123, -195.4285549145483856 ) ) ;
#14089 = CARTESIAN_POINT ( 'NONE',  ( -113.4111493182427779, -282.8852889598923639, -275.6418252806089981 ) ) ;
#14090 = CARTESIAN_POINT ( 'NONE',  ( -68.66870370198434159, -297.4640084013508954, -338.5192818797780774 ) ) ;
#14091 = CARTESIAN_POINT ( 'NONE',  ( -8.033873317821269566, -284.4348554751310871, -201.0881757254733770 ) ) ;
#14092 = AXIS2_PLACEMENT_3D ( 'NONE', #60454, #30626, #67554 ) ;
#14093 = CARTESIAN_POINT ( 'NONE',  ( -107.8480839875027613, -279.7549105419758462, -250.5090994207240271 ) ) ;
#14094 = CARTESIAN_POINT ( 'NONE',  ( 31.03349445238320214, -289.1419799829599810, -239.0131447072785704 ) ) ;
#14095 = CARTESIAN_POINT ( 'NONE',  ( 198.3066790443433263, 289.7462787566917655, -6.801086121950744356 ) ) ;
#14096 = FACE_OUTER_BOUND ( 'NONE', #76110, .T. ) ;
#14097 = CARTESIAN_POINT ( 'NONE',  ( 26.81647790735256009, -294.9390734718807039, -230.3493690000086644 ) ) ;
#14098 = AXIS2_PLACEMENT_3D ( 'NONE', #54040, #26089, #47388 ) ;
#14099 = CARTESIAN_POINT ( 'NONE',  ( -103.6363538570313096, -276.0870243308464183, -305.4327522875097429 ) ) ;
#14100 = CARTESIAN_POINT ( 'NONE',  ( -112.4097825472989882, -289.5437952340702168, -286.7605638025282246 ) ) ;
#14101 = CARTESIAN_POINT ( 'NONE',  ( -50.63509169451015168, -293.6246332432737631, -342.9539974811273737 ) ) ;
#14102 = CARTESIAN_POINT ( 'NONE',  ( -14.13739735806126596, -279.0442022216946611, -200.5735064241824546 ) ) ;
#14103 = CARTESIAN_POINT ( 'NONE',  ( -106.7502204742301615, -270.9861988575748342, -243.3160498892666226 ) ) ;
#14104 = CARTESIAN_POINT ( 'NONE',  ( -75.24822797616758407, -292.8510157606232269, -207.3387023714448958 ) ) ;
#14105 = CARTESIAN_POINT ( 'NONE',  ( -110.4683760289727132, -275.2662352645559167, -253.7030783399848985 ) ) ;
#14106 = CARTESIAN_POINT ( 'NONE',  ( -81.48651210148868529, -294.1202050282088862, -332.6666750782173381 ) ) ;
#14107 = CARTESIAN_POINT ( 'NONE',  ( -69.08380399028303032, -291.0769227756809414, -336.9860326926581138 ) ) ;
#14108 = CARTESIAN_POINT ( 'NONE',  ( -11.47681702660815439, -290.6242242308686059, -198.8566549883668984 ) ) ;
#14109 = CARTESIAN_POINT ( 'NONE',  ( 8.359956293620339096, -289.8375919047977050, -328.0389604849112857 ) ) ;
#14110 = EDGE_CURVE ( 'NONE', #26503, #90054, #8170, .T. ) ;
#14111 = CARTESIAN_POINT ( 'NONE',  ( 184.7149167944524493, 8.542400036368780647, 10.00000000000000000 ) ) ;
#14112 = CARTESIAN_POINT ( 'NONE',  ( -102.9858247835699956, -290.9182363022114828, -302.6636043362885857 ) ) ;
#14113 = DIRECTION ( 'NONE',  ( 1.000000000000000000, 0.000000000000000000, 0.000000000000000000 ) ) ;
#14114 = CARTESIAN_POINT ( 'NONE',  ( -91.30784694221851794, -291.0037857385912616, -324.8017373036926188 ) ) ;
#14116 = CARTESIAN_POINT ( 'NONE',  ( -110.3370467479457488, -290.5412790711283719, -271.1853581452883759 ) ) ;
#14115 = CARTESIAN_POINT ( 'NONE',  ( 14.05824733944782778, -278.7890413343747582, -215.1857518931317088 ) ) ;
#14117 = CARTESIAN_POINT ( 'NONE',  ( -64.73877283943173211, -280.0374185052302778, -198.3664239154715574 ) ) ;
#14118 = CARTESIAN_POINT ( 'NONE',  ( -4.176790403371398064, -282.2935211286444996, -339.8438188120722430 ) ) ;
#14119 = CARTESIAN_POINT ( 'NONE',  ( 21.05512804257926973, -286.1996689679367023, -317.4228977309759898 ) ) ;
#14120 = CARTESIAN_POINT ( 'NONE',  ( 152.4536156746142410, 275.0000000000000568, 12.49999999999999289 ) ) ;
#14121 = CARTESIAN_POINT ( 'NONE',  ( -8.027927935568946793, -280.8035908748170755, -338.5635244063798268 ) ) ;
#14122 = CARTESIAN_POINT ( 'NONE',  ( -111.8302403431622025, -282.6642618400067022, -261.6170900516407301 ) ) ;
#14123 = DIRECTION ( 'NONE',  ( 0.000000000000000000, 0.000000000000000000, 1.000000000000000000 ) ) ;
#14124 = CARTESIAN_POINT ( 'NONE',  ( -111.5059496475745817, -276.8047578784135112, -288.3706192000817055 ) ) ;
#14125 = CARTESIAN_POINT ( 'NONE',  ( -33.72808386111950085, -285.0169607894292767, -193.7554113558723259 ) ) ;
#14126 = CARTESIAN_POINT ( 'NONE',  ( -68.36032304801969417, -274.4368127803882089, -204.0869427637954061 ) ) ;
#14127 = CARTESIAN_POINT ( 'NONE',  ( 151.9300335927204912, 130.8340072618044303, -11.50000000000000178 ) ) ;
#14128 = CARTESIAN_POINT ( 'NONE',  ( -70.59928159606376141, -293.2061292531759022, -204.4796054605857023 ) ) ;
#14129 = CARTESIAN_POINT ( 'NONE',  ( 38.55455174618943914, -277.0945893176096320, -279.6580517081864059 ) ) ;
#14130 = CARTESIAN_POINT ( 'NONE',  ( 25.39156730972660370, -275.7325225945671150, -307.7325595295143330 ) ) ;
#14131 = CARTESIAN_POINT ( 'NONE',  ( 2.657451776626097661, -296.5163127450852585, -333.8660656586477558 ) ) ;
#14132 = CARTESIAN_POINT ( 'NONE',  ( -68.33071209181052552, -291.8229079404740105, -199.8578784062778197 ) ) ;
#14133 = CIRCLE ( 'NONE', #50404, 4.999999999999990230 ) ;
#14134 = CARTESIAN_POINT ( 'NONE',  ( 32.23030895388706796, -280.0158895914046866, -299.9742829114971983 ) ) ;
#14135 = CARTESIAN_POINT ( 'NONE',  ( -36.37623622077202867, -291.8972643645329299, -193.3541384934607663 ) ) ;
#14136 = CARTESIAN_POINT ( 'NONE',  ( -105.9267909436664894, -289.9541152488866942, -244.5366736721687460 ) ) ;
#14137 = AXIS2_PLACEMENT_3D ( 'NONE', #65588, #30978, #58466 ) ;
#14138 = CARTESIAN_POINT ( 'NONE',  ( -55.60847405587371384, -293.2871030211031780, -343.1026165646071036 ) ) ;
#14139 = EDGE_LOOP ( 'NONE', ( #77161, #78539, #70260, #22433, #72188 ) ) ;
#14140 = CARTESIAN_POINT ( 'NONE',  ( 139.6925840978351516, -0.9999999999999991118, 22.50000000000000000 ) ) ;
#14141 = AXIS2_PLACEMENT_3D ( 'NONE', #90872, #5228, #33148 ) ;
#14142 = CARTESIAN_POINT ( 'NONE',  ( -52.37631430583841308, -291.3621718976091870, -198.8112805608855069 ) ) ;
#14143 = DIRECTION ( 'NONE',  ( 0.000000000000000000, 0.000000000000000000, 1.000000000000000000 ) ) ;
#14144 = CARTESIAN_POINT ( 'NONE',  ( -82.13390479932374433, -275.1952119285919025, -326.4764044574609443 ) ) ;
#14145 = CARTESIAN_POINT ( 'NONE',  ( -98.89656482883303568, -296.2230954529638325, -224.4717785838974464 ) ) ;
#14146 = CARTESIAN_POINT ( 'NONE',  ( -71.50341313313676039, -284.8091233526311044, -338.8174956199817984 ) ) ;
#14147 = CARTESIAN_POINT ( 'NONE',  ( 32.67057204759569089, -287.1114232466391627, -249.6462226227446877 ) ) ;
#14148 = CARTESIAN_POINT ( 'NONE',  ( 25.98113282014890757, -277.5856271784311957, -308.0562977641989164 ) ) ;
#14149 = CARTESIAN_POINT ( 'NONE',  ( -48.05344700721762052, -293.2090495897617188, -344.2857781626071301 ) ) ;
#14150 = CARTESIAN_POINT ( 'NONE',  ( -109.4695407548448571, -298.5282735630041770, -253.7614606591411359 ) ) ;
#14151 = CARTESIAN_POINT ( 'NONE',  ( 35.49818444309396881, -274.4708135002339873, -279.7924967494021757 ) ) ;
#14152 = VERTEX_POINT ( 'NONE', #80453 ) ;
#14153 = CARTESIAN_POINT ( 'NONE',  ( 194.3870867008919561, 40.37665348939776777, 14.45687834341487665 ) ) ;
#14154 = CARTESIAN_POINT ( 'NONE',  ( -113.1175540203705623, -296.3884551442629345, -256.8051503496591295 ) ) ;
#14155 = CARTESIAN_POINT ( 'NONE',  ( -37.24201843854251592, -290.9710475411726520, -344.8010552855283777 ) ) ;
#14156 = CARTESIAN_POINT ( 'NONE',  ( 201.9705131854365447, 295.6986650756944073, -54.00000000004518341 ) ) ;
#14157 = AXIS2_PLACEMENT_3D ( 'NONE', #86737, #58358, #7671 ) ;
#14158 = CARTESIAN_POINT ( 'NONE',  ( -34.78611012348081033, -299.1631092010823636, -193.6697713408974835 ) ) ;
#14159 = CARTESIAN_POINT ( 'NONE',  ( 35.75718393720510591, -288.2123652740634725, -271.0288127003307181 ) ) ;
#14160 = ORIENTED_EDGE ( 'NONE', *, *, #2612, .T. ) ;
#14161 = CARTESIAN_POINT ( 'NONE',  ( -35.33014468717838241, -279.1355433263214536, -193.6096747170174410 ) ) ;
#14162 = CARTESIAN_POINT ( 'NONE',  ( 23.09671377799005398, -294.8404175330675798, -317.9270776544768751 ) ) ;
#14163 = CARTESIAN_POINT ( 'NONE',  ( -48.70747715547289403, -287.3348507612859635, -345.3216393609402530 ) ) ;
#14164 = CARTESIAN_POINT ( 'NONE',  ( -56.06103340487253206, -295.6201691311474065, -345.0292561213195768 ) ) ;
#14165 = CARTESIAN_POINT ( 'NONE',  ( 28.75585337935925168, -293.4648975184543929, -239.2063186195713627 ) ) ;
#14166 = CARTESIAN_POINT ( 'NONE',  ( 196.4522879415759462, 72.01292343121092188, -11.25823195237581054 ) ) ;
#14167 = AXIS2_PLACEMENT_3D ( 'NONE', #29712, #74650, #38650 ) ;
#14168 = CARTESIAN_POINT ( 'NONE',  ( 184.7149167944524493, 8.542400036368780647, 10.00000000000000000 ) ) ;
#14169 = CARTESIAN_POINT ( 'NONE',  ( -1.314154478590634278, -288.0413204921113106, -203.0950514380840843 ) ) ;
#14170 = CARTESIAN_POINT ( 'NONE',  ( -37.37352853689063181, -286.5523547857346784, -350.3611179825600175 ) ) ;
#14171 = ORIENTED_EDGE ( 'NONE', *, *, #20803, .F. ) ;
#14172 = EDGE_CURVE ( 'NONE', #17445, #8997, #88492, .T. ) ;
#14173 = CARTESIAN_POINT ( 'NONE',  ( -48.09630881610384279, -279.2674814716438050, -194.1650367415545020 ) ) ;
#14174 = CARTESIAN_POINT ( 'NONE',  ( -38.89830137828109002, -285.0718496014401921, -345.1910694533187893 ) ) ;
#14175 = EDGE_CURVE ( 'NONE', #90412, #22436, #59633, .T. ) ;
#14176 = CARTESIAN_POINT ( 'NONE',  ( -113.7661462205223586, -283.0959919291440769, -272.8120843317425397 ) ) ;
#14177 = CARTESIAN_POINT ( 'NONE',  ( -61.74980847409231899, -287.4516782703860827, -340.6857825303348477 ) ) ;
#14178 = CARTESIAN_POINT ( 'NONE',  ( -2.022198592863591049, -278.4499099738467294, -337.3897558477009966 ) ) ;
#14179 = AXIS2_PLACEMENT_3D ( 'NONE', #87575, #60132, #38787 ) ;
#14180 = CARTESIAN_POINT ( 'NONE',  ( 94.54345169680405547, -300.2393862463458731, -197.2883153065869806 ) ) ;
#14181 = VERTEX_POINT ( 'NONE', #60104 ) ;
#14183 = CARTESIAN_POINT ( 'NONE',  ( -98.07367298108675868, -278.4661649640432870, -229.5831649437682245 ) ) ;
#14182 = CARTESIAN_POINT ( 'NONE',  ( -90.96785078138927361, -277.8401073496189611, -319.9647979423762649 ) ) ;
#14184 = CARTESIAN_POINT ( 'NONE',  ( -7.822324366002685103, -275.5095474325788700, -199.5227006182154810 ) ) ;
#14185 = CARTESIAN_POINT ( 'NONE',  ( -39.56030281678912530, -278.8198367648004705, -193.7773402192825927 ) ) ;
#14186 = CARTESIAN_POINT ( 'NONE',  ( -95.74932028542542639, -238.2749555927843232, -339.3703418869641837 ) ) ;
#14187 = CARTESIAN_POINT ( 'NONE',  ( -26.33373882931265797, -299.6126883303970203, -193.9477346639631890 ) ) ;
#14188 = CARTESIAN_POINT ( 'NONE',  ( -106.6379572354042296, -280.6233781216988064, -303.7686719486574702 ) ) ;
#14189 = ORIENTED_EDGE ( 'NONE', *, *, #52236, .T. ) ;
#14190 = CARTESIAN_POINT ( 'NONE',  ( 82.65773576150654378, -298.8603700640330203, -192.9535473779746724 ) ) ;
#14191 = CARTESIAN_POINT ( 'NONE',  ( -5.677535348280483340, -287.5582457579403126, -204.2291493985908346 ) ) ;
#14192 = CARTESIAN_POINT ( 'NONE',  ( -49.20887793360314078, -287.6631892535194197, -195.2538132873395966 ) ) ;
#14193 = CARTESIAN_POINT ( 'NONE',  ( 34.38255800710944499, -287.0876648124894928, -284.5510676103588139 ) ) ;
#14194 = CARTESIAN_POINT ( 'NONE',  ( -109.9171261506474053, -284.3822664810689957, -244.8202792964235073 ) ) ;
#14195 = CARTESIAN_POINT ( 'NONE',  ( -19.31968362216153423, -278.6876171533806428, -198.7425653684849181 ) ) ;
#14196 = CARTESIAN_POINT ( 'NONE',  ( -4.061699936632904517, -288.3562535035087535, -204.0036988748265969 ) ) ;
#14197 = CARTESIAN_POINT ( 'NONE',  ( 13.83034686957175907, -279.2650493483789091, -217.2604729213304608 ) ) ;
#14198 = CARTESIAN_POINT ( 'NONE',  ( -104.7168326204546958, -279.4737261488638751, -299.8455967829389692 ) ) ;
#14199 = CARTESIAN_POINT ( 'NONE',  ( 20.88976132196879476, -276.6640622060129999, -314.4869079384255883 ) ) ;
#14200 = CARTESIAN_POINT ( 'NONE',  ( -65.31639146576048915, -288.2045816540982628, -341.7293442114217896 ) ) ;
#14201 = CARTESIAN_POINT ( 'NONE',  ( -16.17648113013402167, -283.5882415294979637, -344.2823333714444516 ) ) ;
#14202 = CARTESIAN_POINT ( 'NONE',  ( -16.15276157233750709, -283.2778061240057355, -344.3795666996779801 ) ) ;
#14203 = CARTESIAN_POINT ( 'NONE',  ( -51.82943686677517547, -280.0283971227688653, -198.7614627879414968 ) ) ;
#14204 = ORIENTED_EDGE ( 'NONE', *, *, #72721, .T. ) ;
#14205 = ORIENTED_EDGE ( 'NONE', *, *, #66684, .T. ) ;
#14206 = DIRECTION ( 'NONE',  ( -0.000000000000000000, 1.000000000000000000, -0.000000000000000000 ) ) ;
#14207 = CARTESIAN_POINT ( 'NONE',  ( -38.87110185356192460, -290.9315582267295213, -346.1104837494446542 ) ) ;
#14208 = CARTESIAN_POINT ( 'NONE',  ( -112.6834480584939513, -289.4044036098612196, -257.0600168155260121 ) ) ;
#14209 = CARTESIAN_POINT ( 'NONE',  ( -69.58378455677630825, -272.6756725679842930, -204.6050806885176030 ) ) ;
#14210 = CARTESIAN_POINT ( 'NONE',  ( 36.98619770398142492, -292.6530194230733741, -250.5954167111473794 ) ) ;
#14211 = CARTESIAN_POINT ( 'NONE',  ( -70.29977354516110211, -287.9744968870369348, -336.2877284964466185 ) ) ;
#14212 = CARTESIAN_POINT ( 'NONE',  ( 11.61768635659905335, -290.9820608666790349, -214.7863818383469550 ) ) ;
#14213 = CARTESIAN_POINT ( 'NONE',  ( 6.091885390431315273, -289.6533626928944614, -329.5907933993488541 ) ) ;
#14214 = CARTESIAN_POINT ( 'NONE',  ( -85.28047601435908120, -298.1948066931273615, -330.5268031993605859 ) ) ;
#14215 = AXIS2_PLACEMENT_3D ( 'NONE', #20708, #78929, #13154 ) ;
#14216 = CARTESIAN_POINT ( 'NONE',  ( 35.56638046930439145, -289.7788260828892817, -288.0055735061279165 ) ) ;
#14217 = CARTESIAN_POINT ( 'NONE',  ( -110.1526799126705640, -288.3120511529845658, -289.0832344735468382 ) ) ;
#14218 = CARTESIAN_POINT ( 'NONE',  ( -97.86266170161671596, -293.1564090492837522, -226.0427848314624555 ) ) ;
#14219 = CARTESIAN_POINT ( 'NONE',  ( -101.2023494514472759, -285.9835899968436479, -234.4071123281624409 ) ) ;
#14220 = CARTESIAN_POINT ( 'NONE',  ( -37.80979746801674679, -294.0464577434153739, -195.1959045114138860 ) ) ;
#14221 = CYLINDRICAL_SURFACE ( 'NONE', #92737, 2.000000000000000000 ) ;
#14222 = CARTESIAN_POINT ( 'NONE',  ( 160.5350683151633291, 275.5000000000000568, 25.22542485937379553 ) ) ;
#14223 = CARTESIAN_POINT ( 'NONE',  ( -111.4553565240433528, -274.7096953083733979, -256.4595232962145133 ) ) ;
#14224 = CARTESIAN_POINT ( 'NONE',  ( 35.29883792459870762, -280.8694551212503825, -279.4885035443959964 ) ) ;
#14225 = CARTESIAN_POINT ( 'NONE',  ( -36.18762025512417324, -281.0375223380966645, -345.3522424731692695 ) ) ;
#14226 = CARTESIAN_POINT ( 'NONE',  ( -58.81601623219235364, -294.5200876741650973, -344.1933509878840027 ) ) ;
#14227 = CARTESIAN_POINT ( 'NONE',  ( 34.49809583749038921, -273.5602740460585665, -252.5561262191338017 ) ) ;
#14228 = CARTESIAN_POINT ( 'NONE',  ( -110.9190242024540822, -276.4858121540642060, -281.6611879185322778 ) ) ;
#14229 = CARTESIAN_POINT ( 'NONE',  ( -94.84759697801591471, -298.5092289026271146, -224.5974281484274400 ) ) ;
#14230 = AXIS2_PLACEMENT_3D ( 'NONE', #31675, #81847, #15601 ) ;
#14231 = AXIS2_PLACEMENT_3D ( 'NONE', #82257, #69925, #25885 ) ;
#14232 = CARTESIAN_POINT ( 'NONE',  ( 36.20968394733429108, -294.9465510372061772, -268.0012840673191477 ) ) ;
#14233 = DIRECTION ( 'NONE',  ( 0.000000000000000000, 0.000000000000000000, 1.000000000000000000 ) ) ;
#14234 = CARTESIAN_POINT ( 'NONE',  ( -15.53497142895008842, -295.5655699014115498, -340.2504194071890424 ) ) ;
#14235 = DIRECTION ( 'NONE',  ( 1.124465274301078034E-16, 1.000000000000000000, 0.000000000000000000 ) ) ;
#14237 = CARTESIAN_POINT ( 'NONE',  ( -109.3629154386667039, -296.3949860817008357, -282.2751662108620394 ) ) ;
#14236 = CARTESIAN_POINT ( 'NONE',  ( 37.04705901611494312, -285.7300419957728081, -282.7076432368932615 ) ) ;
#14238 = AXIS2_PLACEMENT_3D ( 'NONE', #44823, #73726, #72790 ) ;
#14239 = CARTESIAN_POINT ( 'NONE',  ( -89.88624419584542125, -285.3349789301513511, -214.0029802891857571 ) ) ;
#14240 = CARTESIAN_POINT ( 'NONE',  ( 10.21155089039267772, -288.0835995478629457, -330.9634850495824594 ) ) ;
#14241 = CARTESIAN_POINT ( 'NONE',  ( -80.89994843296568661, -297.6196557704391239, -331.9153697411414896 ) ) ;
#14242 = CARTESIAN_POINT ( 'NONE',  ( 36.29157792888948109, -291.3793049198741869, -256.9417436737648472 ) ) ;
#14243 = CARTESIAN_POINT ( 'NONE',  ( -53.71607589525477522, -279.0444812739403915, -195.2331100209836450 ) ) ;
#14244 = CARTESIAN_POINT ( 'NONE',  ( -106.6379572354042153, -288.4809262143061801, -236.9535640164627068 ) ) ;
#14245 = CARTESIAN_POINT ( 'NONE',  ( 153.4133700136260927, 129.9709486557057119, 11.65454253063697543 ) ) ;
#14246 = CARTESIAN_POINT ( 'NONE',  ( 35.67094816608467056, -286.2486388854542270, -262.8588720900862654 ) ) ;
#14247 = CARTESIAN_POINT ( 'NONE',  ( 198.9431409017138606, 67.99513008803216962, -10.39089755774709189 ) ) ;
#14248 = DIRECTION ( 'NONE',  ( -1.000000000000000000, -0.000000000000000000, -0.000000000000000000 ) ) ;
#14249 = CARTESIAN_POINT ( 'NONE',  ( -110.1488601851401086, -297.9948560709354979, -282.4258542162618255 ) ) ;
#14250 = CARTESIAN_POINT ( 'NONE',  ( -5.208420572980950070, -281.8921039473032124, -201.0353749997505304 ) ) ;
#14252 = CARTESIAN_POINT ( 'NONE',  ( -3.621382056685119366, -282.5941510114553807, -335.1203171167811661 ) ) ;
#14251 = CARTESIAN_POINT ( 'NONE',  ( -112.3094908349356587, -294.4747353692621346, -277.9924453798475952 ) ) ;
#14253 = CARTESIAN_POINT ( 'NONE',  ( -90.71054468357515077, -295.9501476676332459, -325.9391764204722222 ) ) ;
#14254 = CARTESIAN_POINT ( 'NONE',  ( -72.00811300848877750, -299.1051974635101942, -205.3164247607639652 ) ) ;
#14255 = CARTESIAN_POINT ( 'NONE',  ( 35.31350075570422575, -285.3648001298708436, -249.4257557264824641 ) ) ;
#14256 = CARTESIAN_POINT ( 'NONE',  ( -103.0538490769798727, -281.0330144581539003, -234.2098506933050430 ) ) ;
#14257 = CARTESIAN_POINT ( 'NONE',  ( -72.95083854761396935, -296.6266206054201575, -206.3658235504279617 ) ) ;
#14258 = ORIENTED_EDGE ( 'NONE', *, *, #3543, .T. ) ;
#14259 = CARTESIAN_POINT ( 'NONE',  ( 138.6539576904058606, 132.0000000000000568, -10.49999999999999822 ) ) ;
#14260 = CARTESIAN_POINT ( 'NONE',  ( -51.30131951584609595, -285.2112569108211346, -343.7417190541564196 ) ) ;
#14261 = CYLINDRICAL_SURFACE ( 'NONE', #29226, 35.00000000000002842 ) ;
#14262 = CARTESIAN_POINT ( 'NONE',  ( -95.95921662488163406, -288.6952119285919025, -223.5744983911110353 ) ) ;
#14263 = CARTESIAN_POINT ( 'NONE',  ( 28.95146154147641226, -275.2560932590581046, -309.2118005502748588 ) ) ;
#14264 = CARTESIAN_POINT ( 'NONE',  ( -49.68663578538645709, -291.7237682209976128, -198.3611819217205721 ) ) ;
#14265 = CARTESIAN_POINT ( 'NONE',  ( 20.73926454629947003, -283.7055555390929271, -315.7186895342273374 ) ) ;
#14266 = CARTESIAN_POINT ( 'NONE',  ( 8.088727632410259716, -278.0196545135936503, -328.5856570530591512 ) ) ;
#14267 = CARTESIAN_POINT ( 'NONE',  ( -71.36308232692036313, -285.0940316092591615, -338.5445908440448193 ) ) ;
#14268 = CARTESIAN_POINT ( 'NONE',  ( 15.55614868350091484, -279.6157216648200574, -219.4067886766206641 ) ) ;
#14269 = CARTESIAN_POINT ( 'NONE',  ( -111.9585651631078349, -280.6559419411130420, -262.2904363817988838 ) ) ;
#14270 = CARTESIAN_POINT ( 'NONE',  ( -51.80061419763302411, -297.8721966428390715, -194.6764950348952823 ) ) ;
#14271 = CARTESIAN_POINT ( 'NONE',  ( 34.72250017151666412, -275.0423065454774019, -243.2363868378625966 ) ) ;
#14272 = CARTESIAN_POINT ( 'NONE',  ( 30.81819672352433059, -295.8671014372986292, -300.2867367104673235 ) ) ;
#14273 = DIRECTION ( 'NONE',  ( -1.000000000000000000, -0.000000000000000000, -0.000000000000000000 ) ) ;
#14274 = DIRECTION ( 'NONE',  ( 0.000000000000000000, 0.5150380749100522682, 0.8571673007021134438 ) ) ;
#14275 = CARTESIAN_POINT ( 'NONE',  ( -37.70718656255608892, -293.1962375127823748, -346.1379083971611408 ) ) ;
#14276 = CARTESIAN_POINT ( 'NONE',  ( -1.687124038305205964, -274.0458954562907365, -206.5757981471153357 ) ) ;
#14277 = CARTESIAN_POINT ( 'NONE',  ( 25.90726562454861792, -294.5035958607532507, -227.5800757360402145 ) ) ;
#14278 = CARTESIAN_POINT ( 'NONE',  ( -61.57757895080220578, -292.9493389620859034, -197.6372970451216702 ) ) ;
#14279 = ADVANCED_FACE ( 'NONE', ( #30272 ), #23639, .F. ) ;
#14280 = CARTESIAN_POINT ( 'NONE',  ( -53.78724688457625547, -291.2638794748968962, -343.3650385295980527 ) ) ;
#14281 = CARTESIAN_POINT ( 'NONE',  ( -94.13420992225614725, -275.8752571882094458, -319.0913884559705025 ) ) ;
#14282 = AXIS2_PLACEMENT_3D ( 'NONE', #89880, #3247, #47729 ) ;
#14283 = CARTESIAN_POINT ( 'NONE',  ( -39.16907858581424762, -278.9954182093110830, -344.7786890849434940 ) ) ;
#14284 = CARTESIAN_POINT ( 'NONE',  ( 34.01635981290764477, -291.3548121382031582, -248.9856146860099955 ) ) ;
#14285 = CARTESIAN_POINT ( 'NONE',  ( 29.99044357938772620, -283.8676159804514327, -305.0985315538025588 ) ) ;
#14286 = CARTESIAN_POINT ( 'NONE',  ( -108.9639664917576170, -283.6786396429121169, -254.6667992937428551 ) ) ;
#14287 = EDGE_LOOP ( 'NONE', ( #86540, #7193, #73675, #10545 ) ) ;
#14288 = CARTESIAN_POINT ( 'NONE',  ( -84.87875752425213705, -283.3961050905382422, -325.7895913585948620 ) ) ;
#14289 = CARTESIAN_POINT ( 'NONE',  ( -86.61667922215481497, -280.4658425669377380, -211.5256669765586821 ) ) ;
#14290 = VECTOR ( 'NONE', #6067, 1000.000000000000000 ) ;
#14291 = CARTESIAN_POINT ( 'NONE',  ( -89.60407103446807753, -284.1300972530459603, -214.2831545936875557 ) ) ;
#14292 = AXIS2_PLACEMENT_3D ( 'NONE', #82028, #17186, #18112 ) ;
#14293 = CARTESIAN_POINT ( 'NONE',  ( -114.1426543907955846, -279.5135989684816877, -268.7511795043266716 ) ) ;
#14294 = CARTESIAN_POINT ( 'NONE',  ( -31.48399781683347598, -278.4997139785344871, -346.4947700724522974 ) ) ;
#14295 = CARTESIAN_POINT ( 'NONE',  ( 7.399455738971494334, -295.1948066931273615, -214.2051214447836571 ) ) ;
#14296 = VERTEX_POINT ( 'NONE', #24557 ) ;
#14297 = CARTESIAN_POINT ( 'NONE',  ( -37.86125051787408324, -300.0458004373203380, -195.3629131990695100 ) ) ;
#14298 = VECTOR ( 'NONE', #64062, 1000.000000000000000 ) ;
#14299 = CARTESIAN_POINT ( 'NONE',  ( -84.05530198637387684, -275.7174392797251130, -328.6486712496747487 ) ) ;
#14300 = CARTESIAN_POINT ( 'NONE',  ( -93.97127794204811835, -293.0086743298103329, -219.6949070399757034 ) ) ;
#14301 = CARTESIAN_POINT ( 'NONE',  ( 33.54287338358038539, -293.1362273302929680, -288.2292434180315013 ) ) ;
#14302 = CARTESIAN_POINT ( 'NONE',  ( -98.98359706906708766, -289.4465440357764692, -316.4242299082336558 ) ) ;
#14303 = DIRECTION ( 'NONE',  ( -0.000000000000000000, -1.000000000000000000, -0.000000000000000000 ) ) ;
#14305 = CARTESIAN_POINT ( 'NONE',  ( -39.98235887477027006, -284.4182903699092435, -196.6083733684679373 ) ) ;
#14304 = CARTESIAN_POINT ( 'NONE',  ( 33.89555699529996247, -292.4797392001759135, -297.9991260371943440 ) ) ;
#14306 = CARTESIAN_POINT ( 'NONE',  ( -82.49888445813341775, -293.2888127168125720, -211.3749697095003341 ) ) ;
#14307 = CARTESIAN_POINT ( 'NONE',  ( -37.52504634485897128, -284.3697058703475591, -343.8665548960725573 ) ) ;
#14308 = CARTESIAN_POINT ( 'NONE',  ( -67.94901620420786514, -290.3855031714980441, -340.7600697937497216 ) ) ;
#14309 = CARTESIAN_POINT ( 'NONE',  ( 15.29937166111044178, -281.3128708793848887, -219.6242090191550176 ) ) ;
#14310 = CARTESIAN_POINT ( 'NONE',  ( 37.67859556694827461, -292.5418195981741292, -285.8518879379860778 ) ) ;
#14311 = AXIS2_PLACEMENT_3D ( 'NONE', #64945, #71563, #35087 ) ;
#14312 = CARTESIAN_POINT ( 'NONE',  ( -57.23920504870751103, -290.1052557830640808, -344.6336781534574243 ) ) ;
#14313 = CARTESIAN_POINT ( 'NONE',  ( -114.0505846474586633, -290.9619720733787176, -276.9545647009172171 ) ) ;
#14314 = CARTESIAN_POINT ( 'NONE',  ( -99.61042734543107713, -285.2449734497383815, -232.1648608034618348 ) ) ;
#14315 = VERTEX_POINT ( 'NONE', #24091 ) ;
#14316 = CARTESIAN_POINT ( 'NONE',  ( 195.7548334368592862, 25.47820008840974282, 12.44451950854168132 ) ) ;
#14317 = CARTESIAN_POINT ( 'NONE',  ( 35.90853383186513526, -295.6588484749536292, -289.7185121165886130 ) ) ;
#14318 = CARTESIAN_POINT ( 'NONE',  ( -69.33704263861280026, -294.1492102889079661, -339.8707575857851566 ) ) ;
#14319 = CARTESIAN_POINT ( 'NONE',  ( -85.63036447662732087, -278.4230117712170909, -215.3010295072877796 ) ) ;
#14320 = CARTESIAN_POINT ( 'NONE',  ( -111.7571421343270828, -272.3069483100372281, -250.6158138224584491 ) ) ;
#14321 = CARTESIAN_POINT ( 'NONE',  ( -53.31837622300675861, -293.7405077996714908, -342.3542243935117426 ) ) ;
#14322 = CARTESIAN_POINT ( 'NONE',  ( 28.94793848021655336, -277.7538982752317338, -303.3956843138654449 ) ) ;
#14323 = CARTESIAN_POINT ( 'NONE',  ( -88.16193199841627859, -271.4716836609904362, -216.1781961916792341 ) ) ;
#14324 = CARTESIAN_POINT ( 'NONE',  ( 23.66279123890370784, -294.1935082302219371, -229.5495689064723877 ) ) ;
#14325 = CARTESIAN_POINT ( 'NONE',  ( -38.33273780458437585, -296.1445374993913333, -343.6635321238021561 ) ) ;
#14326 = PLANE ( 'NONE',  #6724 ) ;
#14327 = CARTESIAN_POINT ( 'NONE',  ( -98.41669451788361300, -295.1468274297305925, -226.5447570133376871 ) ) ;
#14328 = CARTESIAN_POINT ( 'NONE',  ( -110.8855674913601916, -273.6370343332343964, -247.9202626443962174 ) ) ;
#14329 = CARTESIAN_POINT ( 'NONE',  ( -71.46195304328433906, -288.0867280163058126, -335.5764546452123227 ) ) ;
#14330 = CARTESIAN_POINT ( 'NONE',  ( -70.39471015352404493, -275.6166088412659292, -203.0372798450532059 ) ) ;
#14331 = CARTESIAN_POINT ( 'NONE',  ( -80.53665008232570699, -290.5949559425654911, -329.5647661375521125 ) ) ;
#14332 = CARTESIAN_POINT ( 'NONE',  ( -102.6700982655681145, -273.5766017732141222, -229.7196699284725980 ) ) ;
#14333 = CARTESIAN_POINT ( 'NONE',  ( -36.99118546351476056, -295.3808934616963029, -343.3938486620118056 ) ) ;
#14334 = CARTESIAN_POINT ( 'NONE',  ( -100.7000855771482719, -279.9839943951257055, -311.2499353221423348 ) ) ;
#14335 = CARTESIAN_POINT ( 'NONE',  ( 36.85710487862867524, -280.0021296299444202, -251.7107665126004861 ) ) ;
#14336 = EDGE_LOOP ( 'NONE', ( #86677, #8205, #46946, #61353 ) ) ;
#14337 = CARTESIAN_POINT ( 'NONE',  ( -83.82819128536965536, -283.0199325487519104, -331.6841877645991303 ) ) ;
#14338 = CARTESIAN_POINT ( 'NONE',  ( 28.41968782960035966, -274.3786126869667896, -230.4001445614988768 ) ) ;
#14339 = CARTESIAN_POINT ( 'NONE',  ( -95.28408749624401253, -277.6267714759453611, -220.8524973914401528 ) ) ;
#14340 = CARTESIAN_POINT ( 'NONE',  ( -6.947759595097298124, -278.4498802102265245, -201.5995516875902354 ) ) ;
#14341 = CARTESIAN_POINT ( 'NONE',  ( -93.10774604524576148, -295.9140532030214672, -222.4732841039282221 ) ) ;
#14342 = CARTESIAN_POINT ( 'NONE',  ( 10.71227879108921677, -278.3885824922330698, -328.0110159857105714 ) ) ;
#14343 = DIRECTION ( 'NONE',  ( -0.000000000000000000, 1.000000000000000000, -0.000000000000000000 ) ) ;
#14344 = CARTESIAN_POINT ( 'NONE',  ( -67.64371597904676037, -289.6766827145651746, -201.3528966301584830 ) ) ;
#14345 = CARTESIAN_POINT ( 'NONE',  ( -34.96041325354462259, -292.0812526684684940, -193.3847983342242856 ) ) ;
#14346 = CARTESIAN_POINT ( 'NONE',  ( -62.95685507476765963, -275.7195489670623374, -199.6936412841522497 ) ) ;
#14347 = CARTESIAN_POINT ( 'NONE',  ( -33.67497888491850233, -296.0979968831556448, -195.5290295220289636 ) ) ;
#14348 = CARTESIAN_POINT ( 'NONE',  ( -57.70328141361187591, -284.9930276645395679, -196.2142869132435692 ) ) ;
#14349 = DIRECTION ( 'NONE',  ( 0.000000000000000000, -1.000000000000000000, 0.000000000000000000 ) ) ;
#14350 = CARTESIAN_POINT ( 'NONE',  ( -105.2991944055074640, -282.1335462649419696, -302.2120066413933159 ) ) ;
#14351 = DIRECTION ( 'NONE',  ( 0.000000000000000000, 1.000000000000000000, 0.000000000000000000 ) ) ;
#14352 = CARTESIAN_POINT ( 'NONE',  ( -7.092655917093349416, -291.2530438912422710, -203.4871631851719087 ) ) ;
#14353 = CARTESIAN_POINT ( 'NONE',  ( -33.14553820353298619, -284.2449980680555655, -196.1939413430673085 ) ) ;
#14354 = CARTESIAN_POINT ( 'NONE',  ( 196.6744398476651554, 24.45234771250604666, 12.85662037485453268 ) ) ;
#14355 = CARTESIAN_POINT ( 'NONE',  ( 159.4851178187817879, 15.28877977928778975, -9.000000000000001776 ) ) ;
#14356 = CARTESIAN_POINT ( 'NONE',  ( 9.456786886954839488, -292.4090604644089240, -329.0358840124710014 ) ) ;
#14357 = CARTESIAN_POINT ( 'NONE',  ( -110.2577045908584097, -283.3191233880940558, -247.6897766699752310 ) ) ;
#14358 = CARTESIAN_POINT ( 'NONE',  ( -109.3921927708529154, -280.3614092548899634, -254.3292481511692529 ) ) ;
#14359 = CARTESIAN_POINT ( 'NONE',  ( -111.4867405742397608, -285.5144640518292931, -289.6620207348321969 ) ) ;
#14360 = CARTESIAN_POINT ( 'NONE',  ( 9.030491218528814201, -286.7095643496063531, -213.9818676353500564 ) ) ;
#14361 = AXIS2_PLACEMENT_3D ( 'NONE', #64919, #30290, #14709 ) ;
#14362 = CARTESIAN_POINT ( 'NONE',  ( -108.3844002298262552, -279.7259553979386624, -289.5525139859456090 ) ) ;
#14363 = CARTESIAN_POINT ( 'NONE',  ( -109.2927588218234973, -279.5294332073900705, -257.1079342077688352 ) ) ;
#14364 = CARTESIAN_POINT ( 'NONE',  ( -2.995578734438594459, -288.4835234001902791, -203.2739552042093862 ) ) ;
#14365 = ORIENTED_EDGE ( 'NONE', *, *, #75740, .T. ) ;
#14366 = CARTESIAN_POINT ( 'NONE',  ( -106.5123895386246602, -296.8198847725601013, -236.5319038185529621 ) ) ;
#14367 = CARTESIAN_POINT ( 'NONE',  ( 28.49276693186321197, -290.0023076678758684, -305.6517272371286822 ) ) ;
#14368 = CARTESIAN_POINT ( 'NONE',  ( 197.2116943569230330, 275.5000000000000568, -12.92446933126074882 ) ) ;
#14369 = CARTESIAN_POINT ( 'NONE',  ( -111.2586520408596868, -280.6233781216988064, -305.9938812882205070 ) ) ;
#14370 = VERTEX_POINT ( 'NONE', #44472 ) ;
#14371 = CARTESIAN_POINT ( 'NONE',  ( -69.32790274241071415, -271.6322069536284971, -202.3256464850647092 ) ) ;
#14372 = CARTESIAN_POINT ( 'NONE',  ( 24.18072300293407650, -291.3488767565308422, -225.4007813636752076 ) ) ;
#14373 = CARTESIAN_POINT ( 'NONE',  ( 35.96210039831592553, -288.9733974347189474, -262.7940458914929991 ) ) ;
#14374 = AXIS2_PLACEMENT_3D ( 'NONE', #35915, #57701, #42533 ) ;
#14375 = CARTESIAN_POINT ( 'NONE',  ( -5.137559053294268985, -282.2421465115551200, -203.7212851917494447 ) ) ;
#14376 = CARTESIAN_POINT ( 'NONE',  ( 19.20054947509118648, -289.6814480229082847, -321.7769188502545035 ) ) ;
#14377 = CARTESIAN_POINT ( 'NONE',  ( 12.10990499644116447, -289.6959510529090380, -328.7378001602225481 ) ) ;
#14378 = CARTESIAN_POINT ( 'NONE',  ( -102.1159769201279914, -286.0472506377767559, -308.1671189971334002 ) ) ;
#14379 = CARTESIAN_POINT ( 'NONE',  ( -106.1765300566876249, -279.1640474096077469, -235.7348802015663409 ) ) ;
#14380 = EDGE_LOOP ( 'NONE', ( #51085, #20821, #59087, #49404 ) ) ;
#14381 = CARTESIAN_POINT ( 'NONE',  ( -53.01488439969033806, -293.3312470911025684, -344.3312566764533358 ) ) ;
#14382 = CARTESIAN_POINT ( 'NONE',  ( 21.97206431031955987, -280.7254256191153559, -221.2604321148812687 ) ) ;
#14383 = CARTESIAN_POINT ( 'NONE',  ( -95.59651220086031742, -275.0510408405118596, -224.3476161127082094 ) ) ;
#14384 = EDGE_CURVE ( 'NONE', #64179, #82136, #52033, .T. ) ;
#14385 = CARTESIAN_POINT ( 'NONE',  ( 39.58706461736021254, -284.0519495502703080, -270.3284710469133074 ) ) ;
#14386 = CARTESIAN_POINT ( 'NONE',  ( -0.5166361833813898352, -272.7744315635289922, -203.8791200527144838 ) ) ;
#14387 = CARTESIAN_POINT ( 'NONE',  ( 184.7149167944524493, -12.49482340714361506, 10.00000000000000000 ) ) ;
#14388 = CARTESIAN_POINT ( 'NONE',  ( -83.47174265841594831, -278.9077171624493303, -213.6387119751212538 ) ) ;
#14389 = CARTESIAN_POINT ( 'NONE',  ( 39.23352203135741689, -276.7313282288343999, -268.3010042182835377 ) ) ;
#14390 = CARTESIAN_POINT ( 'NONE',  ( -88.54869008841748723, -298.7424631669939572, -217.4390427315784962 ) ) ;
#14391 = CARTESIAN_POINT ( 'NONE',  ( -105.5804996657635115, -283.1550370772400242, -305.6379988849880078 ) ) ;
#14392 = CARTESIAN_POINT ( 'NONE',  ( -111.3500630253088133, -292.3011370378496849, -271.2191577044074506 ) ) ;
#14393 = CARTESIAN_POINT ( 'NONE',  ( -5.467654576524973997, -276.0646365443609511, -201.1477837311212795 ) ) ;
#14394 = CARTESIAN_POINT ( 'NONE',  ( 19.00999114233902532, -299.9479996367310832, -193.7469286884922042 ) ) ;
#14395 = CARTESIAN_POINT ( 'NONE',  ( 37.11684435756603051, -295.4496335706466539, -262.3817342449729040 ) ) ;
#14396 = CARTESIAN_POINT ( 'NONE',  ( -23.75706508060757116, -280.8779958869529878, -343.9511044907413293 ) ) ;
#14397 = CARTESIAN_POINT ( 'NONE',  ( -69.61042414466034245, -291.3056377119316949, -200.4577705646783841 ) ) ;
#14398 = CARTESIAN_POINT ( 'NONE',  ( 3.858336639969510262, -272.6295016965917171, -208.0546229927558670 ) ) ;
#14399 = CARTESIAN_POINT ( 'NONE',  ( 1.100306331594340881, -288.1564328317358559, -204.5534449166346178 ) ) ;
#14400 = CARTESIAN_POINT ( 'NONE',  ( -67.91763419731228169, -290.5614137982711327, -203.7189671608931292 ) ) ;
#14401 = ORIENTED_EDGE ( 'NONE', *, *, #77244, .T. ) ;
#14402 = CARTESIAN_POINT ( 'NONE',  ( -98.56797433984831969, -288.5137697662556775, -316.0987284368306973 ) ) ;
#14403 = CARTESIAN_POINT ( 'NONE',  ( -72.37273330338734922, -289.1961088348058411, -334.4307223319834748 ) ) ;
#14404 = ORIENTED_EDGE ( 'NONE', *, *, #7520, .T. ) ;
#14405 = CARTESIAN_POINT ( 'NONE',  ( -26.67774481461488989, -287.2643021460505679, -194.3619817108954919 ) ) ;
#14406 = CARTESIAN_POINT ( 'NONE',  ( -21.64434047212760603, -277.1787543336715771, -341.7270826073668673 ) ) ;
#14407 = EDGE_CURVE ( 'NONE', #57485, #87117, #76237, .T. ) ;
#14408 = CARTESIAN_POINT ( 'NONE',  ( 17.27914756733905222, -291.7295190458441425, -216.4527339613252650 ) ) ;
#14409 = CARTESIAN_POINT ( 'NONE',  ( -106.9098968270767784, -284.7833055188969524, -303.1266302526114487 ) ) ;
#14410 = CARTESIAN_POINT ( 'NONE',  ( -105.4153796666955998, -285.3508834839694259, -234.3064888435326054 ) ) ;
#14411 = CARTESIAN_POINT ( 'NONE',  ( -57.12301384900006695, -280.1230906920644088, -200.0703852067081812 ) ) ;
#14412 = CARTESIAN_POINT ( 'NONE',  ( -30.89368022450710427, -124.4715039767320945, -364.4326362608330214 ) ) ;
#14413 = B_SPLINE_CURVE_WITH_KNOTS ( 'NONE', 3,
 ( #44914, #74752, #1843, #16982, #31659, #75216, #88478, #52492, #36903, #1377, #38278, #73817, #60091, #88930, #80441, #65820, #52954, #928, #15586, #80916, #58689, #2778, #81832, #22680, #29808, #16061, #67652, #81367 ),
 .UNSPECIFIED., .F., .F.,
 ( 4, 2, 2, 2, 2, 2, 2, 2, 2, 2, 2, 2, 2, 4 ),
 ( 0.0002500661914413574642, 0.001032049840278917571, 0.001423041664697730991, 0.001814033489116544410, 0.002205025313535357613, 0.002596017137954171033, 0.002987008962372984452, 0.003378000786791797872, 0.003768992611210611292, 0.004159984435629425145, 0.004550976260048238999, 0.004941968084467051985, 0.005723951733304678824, 0.006505935382142305663 ),
 .UNSPECIFIED. ) ;
#14414 = CARTESIAN_POINT ( 'NONE',  ( -110.7704075034332334, -265.7311065234434295, -306.6539985541684814 ) ) ;
#14415 = CARTESIAN_POINT ( 'NONE',  ( -78.21339102487489470, -207.4003955205593286, -353.8744156467298581 ) ) ;
#14416 = CARTESIAN_POINT ( 'NONE',  ( -76.64237422815001821, -272.7084510478538846, -208.6516475419634844 ) ) ;
#14417 = CARTESIAN_POINT ( 'NONE',  ( 28.14355019523062751, -274.0271315257626270, -237.4079988169975763 ) ) ;
#14418 = CARTESIAN_POINT ( 'NONE',  ( -86.36093546960420042, -295.2195732113673330, -329.6623951154217593 ) ) ;
#14419 = CARTESIAN_POINT ( 'NONE',  ( 122.4157943089394536, 147.2165473011896495, -260.6027802525132415 ) ) ;
#14420 = CARTESIAN_POINT ( 'NONE',  ( -68.62698462865486704, -272.3343739459812127, -200.5289876915827563 ) ) ;
#14421 = CARTESIAN_POINT ( 'NONE',  ( -97.90392683170983901, -299.0020315989928577, -227.4299850107997543 ) ) ;
#14422 = CARTESIAN_POINT ( 'NONE',  ( -45.39999920894819496, -290.4715657419280888, -343.4111507927168532 ) ) ;
#14423 = ORIENTED_EDGE ( 'NONE', *, *, #1254, .T. ) ;
#14424 = CARTESIAN_POINT ( 'NONE',  ( -113.4177797433905539, -297.3598249662886133, -281.0091380986908121 ) ) ;
#14425 = CARTESIAN_POINT ( 'NONE',  ( -8.236189382415831872, -286.9362470003823660, -203.3472560879000355 ) ) ;
#14426 = CARTESIAN_POINT ( 'NONE',  ( -113.2363566762648190, -271.6154328043098758, -258.9769401050100441 ) ) ;
#14427 = CARTESIAN_POINT ( 'NONE',  ( -5.854503303691197758, -295.4514383460938234, -340.4518824039713536 ) ) ;
#14428 = CARTESIAN_POINT ( 'NONE',  ( -69.49648416890707381, -295.9564390758707759, -340.2725829551996526 ) ) ;
#14429 = EDGE_CURVE ( 'NONE', #21926, #45777, #1855, .T. ) ;
#14430 = CARTESIAN_POINT ( 'NONE',  ( -107.7524471625724232, -290.9734253673448166, -251.0912786846745632 ) ) ;
#14431 = VERTEX_POINT ( 'NONE', #23162 ) ;
#14432 = CARTESIAN_POINT ( 'NONE',  ( -64.40754221795538115, -275.6218271742444017, -199.8010802476034655 ) ) ;
#14433 = CARTESIAN_POINT ( 'NONE',  ( 38.74132893143520562, -274.4646653277582686, -279.7147224443534128 ) ) ;
#14434 = ORIENTED_EDGE ( 'NONE', *, *, #13331, .F. ) ;
#14435 = CARTESIAN_POINT ( 'NONE',  ( -113.6552355532110141, -278.1873650746439353, -260.1697941800567264 ) ) ;
#14436 = CARTESIAN_POINT ( 'NONE',  ( 34.29055085857213925, -273.7202609980390662, -252.6055263040511534 ) ) ;
#14437 = CARTESIAN_POINT ( 'NONE',  ( -99.55002201677775986, -274.1648812949173362, -231.5751571062340872 ) ) ;
#14438 = CARTESIAN_POINT ( 'NONE',  ( 29.37353015692898595, -276.8992233874094495, -300.5685093861888504 ) ) ;
#14439 = CARTESIAN_POINT ( 'NONE',  ( 27.62439283027330816, -276.7897786167992535, -230.8476234467975132 ) ) ;
#14440 = CARTESIAN_POINT ( 'NONE',  ( 22.20251835274090269, -274.2026633635754820, -316.5652897589919803 ) ) ;
#14441 = CARTESIAN_POINT ( 'NONE',  ( -9.183961762373082038, -295.3254441350799198, -337.8360987497922565 ) ) ;
#14442 = CARTESIAN_POINT ( 'NONE',  ( 18.04659286505167870, -300.6605412952987990, -194.7831514931514505 ) ) ;
#14443 = CARTESIAN_POINT ( 'NONE',  ( 20.14275556054300154, -292.7709200658823647, -316.3258645102907849 ) ) ;
#14444 = CARTESIAN_POINT ( 'NONE',  ( 200.6103193995254230, 276.0000000000000568, -2.464576988612312114 ) ) ;
#14445 = CARTESIAN_POINT ( 'NONE',  ( -112.4229776781453580, -278.8341882431408862, -287.1637566155142736 ) ) ;
#14446 = CARTESIAN_POINT ( 'NONE',  ( -69.24949975702652694, -277.6506388362375901, -336.0323408013662174 ) ) ;
#14447 = CIRCLE ( 'NONE', #6870, 6.151811579824029153 ) ;
#14448 = CARTESIAN_POINT ( 'NONE',  ( -30.90852138100013491, -284.8166476387335706, -194.1120080189415376 ) ) ;
#14449 = CARTESIAN_POINT ( 'NONE',  ( -78.45245292563932082, -297.6042968919602458, -333.2891278769662904 ) ) ;
#14450 = CARTESIAN_POINT ( 'NONE',  ( 175.2296996224750103, 215.0000000000000568, 0.000000000000000000 ) ) ;
#14451 = CARTESIAN_POINT ( 'NONE',  ( 34.91709743725075299, -286.9011723239887601, -281.8981062075125692 ) ) ;
#14452 = CARTESIAN_POINT ( 'NONE',  ( -72.15030934911615645, -275.7589682696256546, -335.6926008550572078 ) ) ;
#14453 = CARTESIAN_POINT ( 'NONE',  ( -32.39896772593964869, -275.5634787360673386, -343.8345382929208540 ) ) ;
#14454 = CARTESIAN_POINT ( 'NONE',  ( -94.86477220922611764, -285.8871905615400806, -318.5065006035287070 ) ) ;
#14455 = CARTESIAN_POINT ( 'NONE',  ( -69.41112767921349302, -278.6888663787347014, -336.3953466727637078 ) ) ;
#14456 = DIRECTION ( 'NONE',  ( 0.000000000000000000, 0.000000000000000000, 1.000000000000000000 ) ) ;
#14457 = CARTESIAN_POINT ( 'NONE',  ( 19.26906676728643930, -274.6518835703760146, -321.3871235923590461 ) ) ;
#14458 = CARTESIAN_POINT ( 'NONE',  ( 34.26608482253153909, -276.3972716120188693, -285.0654643800544932 ) ) ;
#14459 = CARTESIAN_POINT ( 'NONE',  ( 37.87572481208437125, -283.5466024402552421, -269.9151042571986636 ) ) ;
#14460 = DIRECTION ( 'NONE',  ( -0.000000000000000000, 0.000000000000000000, -1.000000000000000000 ) ) ;
#14461 = CARTESIAN_POINT ( 'NONE',  ( 35.29991974877142269, -289.2044881254864208, -249.3786929451851506 ) ) ;
#14462 = CARTESIAN_POINT ( 'NONE',  ( 35.88369702992221733, -291.7609199512125997, -286.6376608965923651 ) ) ;
#14463 = DIRECTION ( 'NONE',  ( 0.000000000000000000, -0.000000000000000000, 1.000000000000000000 ) ) ;
#14464 = CARTESIAN_POINT ( 'NONE',  ( -109.6115687996755668, -271.4155068255307128, -256.7359658464415588 ) ) ;
#14465 = CARTESIAN_POINT ( 'NONE',  ( -6.739775739704214175, -290.5978096821435770, -202.7268980437074219 ) ) ;
#14466 = CARTESIAN_POINT ( 'NONE',  ( -45.58595926748305516, -157.7977398304416283, -369.2266198007532125 ) ) ;
#14467 = FACE_OUTER_BOUND ( 'NONE', #66572, .T. ) ;
#14468 = CARTESIAN_POINT ( 'NONE',  ( -110.8790282293439873, -288.7745052077437435, -290.7319090694129500 ) ) ;
#14469 = CARTESIAN_POINT ( 'NONE',  ( -111.2390156027235832, -282.5670511337223161, -288.1126141131154554 ) ) ;
#14470 = CARTESIAN_POINT ( 'NONE',  ( -48.39945455645703731, -284.6209385630046427, -343.1148188022164049 ) ) ;
#14471 = CARTESIAN_POINT ( 'NONE',  ( -110.3901388725797545, -285.4194407378547567, -265.4645607995058754 ) ) ;
#14472 = CARTESIAN_POINT ( 'NONE',  ( -108.8776233533928774, -292.8385630391066456, -246.5118268269977762 ) ) ;
#14473 = CARTESIAN_POINT ( 'NONE',  ( 1.181162909312186704, -274.8851213153484423, -203.6995074189279649 ) ) ;
#14474 = CARTESIAN_POINT ( 'NONE',  ( -110.5924412669333066, -288.8689748160747968, -251.7714571291788559 ) ) ;
#14475 = CARTESIAN_POINT ( 'NONE',  ( -1.467729270677221587, -276.5897947753927610, -338.4937695889823885 ) ) ;
#14476 = CARTESIAN_POINT ( 'NONE',  ( 33.92449846294908156, -295.8197783759478057, -292.5641750120211100 ) ) ;
#14477 = DIRECTION ( 'NONE',  ( 0.000000000000000000, 0.000000000000000000, -1.000000000000000000 ) ) ;
#14478 = CARTESIAN_POINT ( 'NONE',  ( -69.91165696735023971, -300.1233781216987495, -202.8022627189028810 ) ) ;
#14479 = CARTESIAN_POINT ( 'NONE',  ( -109.4666706674200043, -283.0520246209561606, -284.4760782690611904 ) ) ;
#14480 = CARTESIAN_POINT ( 'NONE',  ( -40.88767294294499521, -278.0074011142497170, -195.4321337789455697 ) ) ;
#14481 = CARTESIAN_POINT ( 'NONE',  ( -83.14828806871129530, -271.9179320463293266, -209.2666095534543160 ) ) ;
#14482 = CARTESIAN_POINT ( 'NONE',  ( 20.09741051231208431, -275.5379207833321971, -315.5989837358765726 ) ) ;
#14483 = CARTESIAN_POINT ( 'NONE',  ( 32.45148768063754119, -294.7590373082715018, -246.5461308311271011 ) ) ;
#14484 = CARTESIAN_POINT ( 'NONE',  ( 31.04383635395285168, -294.1445138563373689, -244.1537364318259904 ) ) ;
#14485 = CARTESIAN_POINT ( 'NONE',  ( 21.00250380493349667, -295.5386938346554757, -319.8510375773423107 ) ) ;
#14486 = CARTESIAN_POINT ( 'NONE',  ( -109.7359493454813872, -296.5143073771769195, -260.5946354563778300 ) ) ;
#14487 = CARTESIAN_POINT ( 'NONE',  ( -67.09976804096399405, -291.4422528946016655, -339.2603257240036214 ) ) ;
#14488 = CARTESIAN_POINT ( 'NONE',  ( -44.41710106374254252, -283.3058588170700887, -347.0887129046465134 ) ) ;
#14489 = CARTESIAN_POINT ( 'NONE',  ( -0.6229824058376443041, -272.6741730467479101, -204.0738858503770530 ) ) ;
#14490 = CARTESIAN_POINT ( 'NONE',  ( 28.69963864912850582, -286.8679842640183892, -230.6660903507437581 ) ) ;
#14491 = CARTESIAN_POINT ( 'NONE',  ( -100.5548726351711792, -279.9947660874887561, -310.1557495517070038 ) ) ;
#14492 = ADVANCED_FACE ( 'NONE', ( #8488 ), #71742, .T. ) ;
#14493 = CARTESIAN_POINT ( 'NONE',  ( -11.92913331271559763, -285.4499891673439151, -201.6762586907419745 ) ) ;
#14494 = CARTESIAN_POINT ( 'NONE',  ( -38.90471179144449820, -287.0716063474030193, -345.3448338609537700 ) ) ;
#14495 = CARTESIAN_POINT ( 'NONE',  ( -111.2639016180397959, -258.5489101121608542, -316.4159311957783984 ) ) ;
#14496 = CARTESIAN_POINT ( 'NONE',  ( -109.9346344960164572, -283.9451533273092423, -279.0594627419676499 ) ) ;
#14497 = CARTESIAN_POINT ( 'NONE',  ( 25.94386595009920526, -282.1839297177074286, -227.1067327960679165 ) ) ;
#14498 = LINE ( 'NONE', #79543, #33699 ) ;
#14499 = CARTESIAN_POINT ( 'NONE',  ( -91.44124123220973388, -288.8578038866108386, -324.8974508624912687 ) ) ;
#14500 = CARTESIAN_POINT ( 'NONE',  ( -112.9696262617293598, -280.0292301366362722, -280.0977042042364360 ) ) ;
#14501 = CARTESIAN_POINT ( 'NONE',  ( -88.61344510260813934, -280.6655455610133458, -213.5763802541279404 ) ) ;
#14502 = CARTESIAN_POINT ( 'NONE',  ( -30.26027235691184458, -279.9774076899155943, -197.6550446580477853 ) ) ;
#14503 = CARTESIAN_POINT ( 'NONE',  ( -0.9421106629741500260, -276.5177356394447088, -205.1781124975804289 ) ) ;
#14504 = CARTESIAN_POINT ( 'NONE',  ( 39.65600365699447138, -293.5155770713311654, -267.4366029175038761 ) ) ;
#14505 = CARTESIAN_POINT ( 'NONE',  ( 33.87545233411397305, -285.8640835243630818, -292.8928352280831291 ) ) ;
#14506 = VECTOR ( 'NONE', #22539, 1000.000000000000000 ) ;
#14507 = CARTESIAN_POINT ( 'NONE',  ( -22.37111331057360530, -293.8407550719356323, -195.5924208132926196 ) ) ;
#14508 = CARTESIAN_POINT ( 'NONE',  ( -95.02514531090415062, -294.8372273175374403, -315.6032026661418968 ) ) ;
#14509 = CARTESIAN_POINT ( 'NONE',  ( -43.01880810896771123, -285.0443870198723175, -344.6354010910411034 ) ) ;
#14510 = CARTESIAN_POINT ( 'NONE',  ( -58.41839577875898470, -294.9989764767250904, -340.2743526892491559 ) ) ;
#14511 = CARTESIAN_POINT ( 'NONE',  ( -98.96445349272538294, -292.2413836795672637, -224.6868547161107017 ) ) ;
#14512 = CARTESIAN_POINT ( 'NONE',  ( 31.16292369346579960, -281.8619956701181195, -244.7010563432375250 ) ) ;
#14513 = EDGE_CURVE ( 'NONE', #84890, #40555, #2164, .T. ) ;
#14514 = CARTESIAN_POINT ( 'NONE',  ( -78.70465440538337987, -272.5681629685304301, -205.6933035302457995 ) ) ;
#14515 = CARTESIAN_POINT ( 'NONE',  ( -82.78572066212326774, -290.3070029441332167, -332.3946071959687742 ) ) ;
#14516 = CARTESIAN_POINT ( 'NONE',  ( -91.56651892380735092, -281.9541073794486579, -323.2759033108702624 ) ) ;
#14517 = CARTESIAN_POINT ( 'NONE',  ( -98.33411376711671892, -291.5125114057701126, -223.3752286448122391 ) ) ;
#14518 = CARTESIAN_POINT ( 'NONE',  ( 22.00628498951112633, -287.2899505504071271, -227.7329077464494844 ) ) ;
#14519 = CARTESIAN_POINT ( 'NONE',  ( 128.9467878515196162, -299.5541904835127980, -189.1116627405232578 ) ) ;
#14520 = CARTESIAN_POINT ( 'NONE',  ( -49.41460023398800416, -154.1821796365580894, -362.9324954162679546 ) ) ;
#14521 = CARTESIAN_POINT ( 'NONE',  ( -88.81474777452721980, -229.3358420801235695, -344.3332919790561277 ) ) ;
#14522 = CARTESIAN_POINT ( 'NONE',  ( -109.7802148314754760, -277.8889832527767112, -259.7501468087731382 ) ) ;
#14523 = CARTESIAN_POINT ( 'NONE',  ( -101.0737859873117941, -277.9665651670258626, -234.1334033853535175 ) ) ;
#14524 = CARTESIAN_POINT ( 'NONE',  ( 11.77546588010454798, -274.3792707720593285, -211.0191881301796286 ) ) ;
#14525 = CARTESIAN_POINT ( 'NONE',  ( -104.5657734472104181, -261.9804595554911657, -316.2884981726831484 ) ) ;
#14526 = CARTESIAN_POINT ( 'NONE',  ( -111.5095649910323203, -277.3591769470508552, -251.9299453443525465 ) ) ;
#14527 = CARTESIAN_POINT ( 'NONE',  ( -92.90589819667893323, -281.8744731503331877, -320.2247838378879692 ) ) ;
#14528 = CARTESIAN_POINT ( 'NONE',  ( -113.2204528967522918, -298.2497500708282701, -275.2961954638095676 ) ) ;
#14529 = CARTESIAN_POINT ( 'NONE',  ( -104.7622770194931690, -291.4233665442075676, -242.0788721421332639 ) ) ;
#14530 = CARTESIAN_POINT ( 'NONE',  ( -56.20823887814563591, -287.9850105642919402, -341.4442886955926610 ) ) ;
#14531 = CARTESIAN_POINT ( 'NONE',  ( 9.441750169202579812, -275.3279548545359603, -209.3314402466088495 ) ) ;
#14532 = CARTESIAN_POINT ( 'NONE',  ( -62.02969541815978971, -273.7220155636430832, -201.6624797969521126 ) ) ;
#14533 = ORIENTED_EDGE ( 'NONE', *, *, #65821, .T. ) ;
#14534 = DIRECTION ( 'NONE',  ( -1.000000000000000000, 0.000000000000000000, 0.000000000000000000 ) ) ;
#14535 = DIRECTION ( 'NONE',  ( -0.000000000000000000, -0.000000000000000000, -1.000000000000000000 ) ) ;
#14536 = CARTESIAN_POINT ( 'NONE',  ( -100.6974140603196304, -281.0244191217836374, -229.0915537689155030 ) ) ;
#14537 = CARTESIAN_POINT ( 'NONE',  ( -6.652513635218989307, -281.5444808028910870, -203.7711441255180773 ) ) ;
#14538 = CARTESIAN_POINT ( 'NONE',  ( 16.48920718330317214, -282.5641733604166461, -216.6570758301816682 ) ) ;
#14539 = CARTESIAN_POINT ( 'NONE',  ( -64.15263536178552783, -282.4694777003194872, -338.5122896539165822 ) ) ;
#14540 = CARTESIAN_POINT ( 'NONE',  ( -100.2087378817642644, -279.8753090915332677, -309.9362131319967943 ) ) ;
#14541 = CARTESIAN_POINT ( 'NONE',  ( -32.62752405860703675, -272.5924860293567917, -196.8060748556924864 ) ) ;
#14542 = CARTESIAN_POINT ( 'NONE',  ( 209.2607772797596226, 29.59979094061341343, 14.77866956795157094 ) ) ;
#14543 = CARTESIAN_POINT ( 'NONE',  ( 164.2231345125756263, 275.5000000000000568, 22.80382896337009058 ) ) ;
#14544 = CARTESIAN_POINT ( 'NONE',  ( -111.2823407084260907, -279.0924499792002393, -291.2642395510175106 ) ) ;
#14545 = CARTESIAN_POINT ( 'NONE',  ( 199.6150009768959990, 250.0000000000000568, -2.367926910627516257 ) ) ;
#14546 = CARTESIAN_POINT ( 'NONE',  ( -20.27550205217131563, -275.4119303759320019, -344.8959571593156284 ) ) ;
#14547 = ORIENTED_EDGE ( 'NONE', *, *, #89262, .T. ) ;
#14548 = CARTESIAN_POINT ( 'NONE',  ( 209.2561782394521686, 27.88178916653710715, 12.07126757350762603 ) ) ;
#14549 = CARTESIAN_POINT ( 'NONE',  ( -63.32079117999034423, -285.3688541233674982, -341.0964954846953674 ) ) ;
#14550 = CARTESIAN_POINT ( 'NONE',  ( 33.80719320609994583, -292.5243391545574241, -253.2653617537477544 ) ) ;
#14551 = CARTESIAN_POINT ( 'NONE',  ( -54.48697109193350485, -288.6153082511057164, -345.3780989725769928 ) ) ;
#14552 = CARTESIAN_POINT ( 'NONE',  ( -110.5034815241817796, -282.6420615652609172, -281.8855572341871607 ) ) ;
#14554 = CARTESIAN_POINT ( 'NONE',  ( 24.74842285157107824, -285.0722433439945007, -229.2052258075054283 ) ) ;
#14553 = CARTESIAN_POINT ( 'NONE',  ( -110.5789524541091282, -283.2275121335682684, -262.6705760848790305 ) ) ;
#14555 = CARTESIAN_POINT ( 'NONE',  ( -3.424320888788228601, -283.7990318890963408, -335.4654600628635990 ) ) ;
#14556 = CARTESIAN_POINT ( 'NONE',  ( -27.24000820384891952, -272.1802448852197358, -195.9924783395721590 ) ) ;
#14557 = CARTESIAN_POINT ( 'NONE',  ( -75.68634411076639879, -283.9496400395147475, -204.4510765533989343 ) ) ;
#14558 = CARTESIAN_POINT ( 'NONE',  ( -34.89372829054680381, -297.0215532170644224, -345.3211612423731367 ) ) ;
#14559 = CARTESIAN_POINT ( 'NONE',  ( -94.40760799030290684, -283.2289695933618532, -221.3595619813672783 ) ) ;
#14560 = CARTESIAN_POINT ( 'NONE',  ( -79.19913533188103827, -280.4129184538163599, -210.2664962121950794 ) ) ;
#14561 = CARTESIAN_POINT ( 'NONE',  ( 35.72838499098572385, -289.7788260859461502, -288.0448388335037748 ) ) ;
#14562 = DIRECTION ( 'NONE',  ( 0.9531768234071952284, -0.3024135303179549261, 0.000000000000000000 ) ) ;
#14563 = CARTESIAN_POINT ( 'NONE',  ( 139.1539576904058606, 275.5000000000000568, 20.22542485937379908 ) ) ;
#14564 = CARTESIAN_POINT ( 'NONE',  ( 10.30950500425925576, -296.3211470108273602, -329.0687937420232174 ) ) ;
#14565 = VECTOR ( 'NONE', #30208, 1000.000000000000000 ) ;
#14566 = CARTESIAN_POINT ( 'NONE',  ( -59.81798225130545887, -275.3431944377480249, -341.9140172150532635 ) ) ;
#14567 = CARTESIAN_POINT ( 'NONE',  ( -108.6524110473766598, -289.3853857308030229, -298.9782689285400465 ) ) ;
#14568 = CARTESIAN_POINT ( 'NONE',  ( -58.65857752850371298, -293.7323332621447776, -341.0154253634128168 ) ) ;
#14569 = CARTESIAN_POINT ( 'NONE',  ( -105.9688156012415590, -277.5875196206615101, -243.9210882132089182 ) ) ;
#14570 = CARTESIAN_POINT ( 'NONE',  ( 9.937728193903602403, -296.7896868835665600, -196.1410897974839713 ) ) ;
#14571 = CARTESIAN_POINT ( 'NONE',  ( -52.48764953243479425, -293.1694022785607672, -198.3933322377198181 ) ) ;
#14572 = CARTESIAN_POINT ( 'NONE',  ( -106.6379572354042153, -286.6233781216988064, -303.7686719486574134 ) ) ;
#14573 = CARTESIAN_POINT ( 'NONE',  ( -47.55807765510908780, -293.6596596604184697, -345.9807806486943491 ) ) ;
#14574 = CARTESIAN_POINT ( 'NONE',  ( -89.20899527712366250, -291.3971638969904916, -322.8608713941123369 ) ) ;
#14575 = CARTESIAN_POINT ( 'NONE',  ( -98.23076809806080689, -288.1789549828755526, -315.8413649475575653 ) ) ;
#14576 = EDGE_CURVE ( 'NONE', #50286, #92859, #16075, .T. ) ;
#14577 = CARTESIAN_POINT ( 'NONE',  ( 28.76497199245203618, -289.4118459033713293, -302.6919518190782696 ) ) ;
#14578 = CARTESIAN_POINT ( 'NONE',  ( -95.89141555491156055, -290.7402959891028331, -314.2515159380465661 ) ) ;
#14579 = CARTESIAN_POINT ( 'NONE',  ( 196.0722908565159344, 20.74697382034803894, 13.80893104049734177 ) ) ;
#14580 = CARTESIAN_POINT ( 'NONE',  ( -26.18714110429508679, -290.1182313084445923, -346.1475582652686853 ) ) ;
#14581 = CARTESIAN_POINT ( 'NONE',  ( -108.0538028949382294, -276.9103282117731055, -244.1682332639914250 ) ) ;
#14582 = CARTESIAN_POINT ( 'NONE',  ( -72.50094124074007595, -279.9329412640670398, -201.8660201664554279 ) ) ;
#14583 = CARTESIAN_POINT ( 'NONE',  ( 22.50414704806151178, -281.8684927939851832, -318.7990479371065931 ) ) ;
#14584 = CARTESIAN_POINT ( 'NONE',  ( 34.59533163545942358, -285.2782388284990702, -249.1010454784302510 ) ) ;
#14585 = CARTESIAN_POINT ( 'NONE',  ( 29.33919985515026596, -280.8906705383787994, 22.50000000000000000 ) ) ;
#14586 = CARTESIAN_POINT ( 'NONE',  ( 32.23617289961259758, -279.3505710967674531, -244.3333083263952688 ) ) ;
#14587 = CARTESIAN_POINT ( 'NONE',  ( -111.1728559817797333, -282.3789735861350323, -283.8362288018965387 ) ) ;
#14588 = CARTESIAN_POINT ( 'NONE',  ( 201.7602898350666294, 289.7935801615433320, -82.39453394557040156 ) ) ;
#14589 = CARTESIAN_POINT ( 'NONE',  ( -113.6837404213119811, -277.0526210999673253, -268.7295763606512651 ) ) ;
#14590 = CARTESIAN_POINT ( 'NONE',  ( -110.3953052805852764, -283.1774024616702263, -293.7424718663654630 ) ) ;
#14591 = CARTESIAN_POINT ( 'NONE',  ( -102.1782790309612921, -273.8165335113363881, -236.3571181942858743 ) ) ;
#14592 = CARTESIAN_POINT ( 'NONE',  ( -110.4958876469581242, -292.2843612492586090, -260.2393685241858066 ) ) ;
#14593 = CARTESIAN_POINT ( 'NONE',  ( -41.18146184613213734, -275.4301161149136874, -193.9950234166425957 ) ) ;
#14594 = CARTESIAN_POINT ( 'NONE',  ( 33.60606453054442966, -275.4473897365221546, -287.6909929420282879 ) ) ;
#14595 = CARTESIAN_POINT ( 'NONE',  ( -39.72783100643441401, -297.0822525087519921, -345.3359265764544830 ) ) ;
#14596 = CARTESIAN_POINT ( 'NONE',  ( -12.22172293336124405, -288.9009801473249013, -343.2042606928760620 ) ) ;
#14597 = CARTESIAN_POINT ( 'NONE',  ( 32.99314433328827789, -279.2736798469460382, -242.6079808221576570 ) ) ;
#14598 = CARTESIAN_POINT ( 'NONE',  ( 4.143321927639485480, -292.4276496689330997, -205.4288719333016218 ) ) ;
#14599 = CARTESIAN_POINT ( 'NONE',  ( -106.7906319551526337, -289.9186093409297769, -247.1177465376811426 ) ) ;
#14600 = CARTESIAN_POINT ( 'NONE',  ( -73.66077835339257263, -293.5336571079670875, -336.0388376058859308 ) ) ;
#14601 = ORIENTED_EDGE ( 'NONE', *, *, #87556, .F. ) ;
#14602 = DIRECTION ( 'NONE',  ( 0.000000000000000000, 1.000000000000000000, -0.000000000000000000 ) ) ;
#14603 = CARTESIAN_POINT ( 'NONE',  ( -69.03863095940953087, -291.1313927356917475, -204.5195509894005852 ) ) ;
#14604 = CARTESIAN_POINT ( 'NONE',  ( 207.7755975652985114, 28.53818587417392649, 12.98477611641283858 ) ) ;
#14605 = CARTESIAN_POINT ( 'NONE',  ( 32.49297727881272380, -288.0832418733486975, -238.3594161485135032 ) ) ;
#14606 = CARTESIAN_POINT ( 'NONE',  ( 30.89617123739170168, -279.2666405000204009, -285.9686137636504668 ) ) ;
#14607 = CARTESIAN_POINT ( 'NONE',  ( -16.58206775401803768, -293.8491766759644293, -344.3205625401920997 ) ) ;
#14608 = CARTESIAN_POINT ( 'NONE',  ( -105.0038316043518449, -286.3326182936935993, -234.5386166278920257 ) ) ;
#14609 = CARTESIAN_POINT ( 'NONE',  ( -108.3650178957309294, -284.6087072466704626, -253.4345796551743035 ) ) ;
#14610 = B_SPLINE_CURVE_WITH_KNOTS ( 'NONE', 3,
 ( #93631, #81631, #14127, #60353, #79457, #64352 ),
 .UNSPECIFIED., .F., .F.,
 ( 4, 2, 4 ),
 ( 0.000000000000000000, 0.0008511423910808053710, 0.001702284782161610742 ),
 .UNSPECIFIED. ) ;
#14611 = CARTESIAN_POINT ( 'NONE',  ( 34.79610212069702868, -276.8746571627081039, -255.2382075643229769 ) ) ;
#14612 = CARTESIAN_POINT ( 'NONE',  ( 37.26609728160536861, -291.5419346069503490, -268.0109338623844906 ) ) ;
#14613 = CARTESIAN_POINT ( 'NONE',  ( 35.47616161325443329, -295.1389989878197184, -257.0418718988964883 ) ) ;
#14614 = CARTESIAN_POINT ( 'NONE',  ( -3.699060005711096721, -275.3927422740687803, -335.5938035892796165 ) ) ;
#14615 = VERTEX_POINT ( 'NONE', #84179 ) ;
#14616 = FACE_BOUND ( 'NONE', #27456, .T. ) ;
#14617 = CARTESIAN_POINT ( 'NONE',  ( 39.48073370224899747, -293.2899362352617345, -276.0418147363309345 ) ) ;
#14618 = CARTESIAN_POINT ( 'NONE',  ( -0.2531660325689735203, -290.4753977054880920, -334.9631199203266192 ) ) ;
#14619 = CARTESIAN_POINT ( 'NONE',  ( 202.4544974499246450, 295.8994530942177335, -54.00000000005819345 ) ) ;
#14620 = CARTESIAN_POINT ( 'NONE',  ( -103.8922123153729729, -274.2536656754602973, -232.3199749452595597 ) ) ;
#14621 = CARTESIAN_POINT ( 'NONE',  ( -62.60587658726665694, -286.3660555146923912, -201.7096536215012179 ) ) ;
#14622 = ORIENTED_EDGE ( 'NONE', *, *, #32885, .F. ) ;
#14623 = CARTESIAN_POINT ( 'NONE',  ( -98.38194974759099409, -278.2336065095286131, -223.7896486949875339 ) ) ;
#14624 = CARTESIAN_POINT ( 'NONE',  ( 25.63594620929465506, -294.7880718475470303, -314.5103847847877887 ) ) ;
#14625 = CARTESIAN_POINT ( 'NONE',  ( -59.68596496909783156, -287.4781480073875741, -342.7561406511053974 ) ) ;
#14626 = CARTESIAN_POINT ( 'NONE',  ( -90.69436026410672014, -296.1167219692090953, -325.9253834831050654 ) ) ;
#14627 = CARTESIAN_POINT ( 'NONE',  ( 2.248400320746489989, -292.9314914033633386, -208.9439779899522023 ) ) ;
#14628 = CARTESIAN_POINT ( 'NONE',  ( 156.4851178187871312, 3.000000000000000000, -7.000000000000000888 ) ) ;
#14629 = LINE ( 'NONE', #23576, #14565 ) ;
#14630 = DIRECTION ( 'NONE',  ( 0.000000000000000000, -1.000000000000000000, 0.000000000000000000 ) ) ;
#14631 = CARTESIAN_POINT ( 'NONE',  ( 7.124056261922285138, -288.1654102198533565, -208.2839207440228790 ) ) ;
#14632 = CARTESIAN_POINT ( 'NONE',  ( -19.11405058567864046, -292.3380690714489560, -350.3683826091709648 ) ) ;
#14633 = ORIENTED_EDGE ( 'NONE', *, *, #27345, .F. ) ;
#14634 = CARTESIAN_POINT ( 'NONE',  ( -90.98111492513071141, -278.6635134398146079, -215.1858400577562520 ) ) ;
#14635 = CARTESIAN_POINT ( 'NONE',  ( -20.96274796952394937, -284.8417872618542219, -343.4333311103478081 ) ) ;
#14636 = CARTESIAN_POINT ( 'NONE',  ( -111.9536967999439412, -282.9191668208275132, -286.8431156798611141 ) ) ;
#14637 = CARTESIAN_POINT ( 'NONE',  ( -64.36603136489249266, -287.4872895920181577, -339.7777504543332157 ) ) ;
#14638 = CARTESIAN_POINT ( 'NONE',  ( 36.70365276891058670, -277.6173291475838028, -286.4714669451807936 ) ) ;
#14639 = CARTESIAN_POINT ( 'NONE',  ( -55.31486126426177208, -298.3071144370772458, -199.4924226413671136 ) ) ;
#14641 = VERTEX_POINT ( 'NONE', #69062 ) ;
#14640 = EDGE_CURVE ( 'NONE', #7049, #77260, #693, .T. ) ;
#14642 = CARTESIAN_POINT ( 'NONE',  ( 33.92016462287811152, -292.4725739042638111, -288.3330436326261292 ) ) ;
#14644 = CARTESIAN_POINT ( 'NONE',  ( -62.33601441295277823, -279.0669760907175601, -201.6114231959803931 ) ) ;
#14643 = CARTESIAN_POINT ( 'NONE',  ( -107.9725817296657056, -278.7962843390746457, -251.8653763962713867 ) ) ;
#14645 = CARTESIAN_POINT ( 'NONE',  ( -52.49804125370265240, -274.9422038608369689, -195.1285865851194501 ) ) ;
#14646 = CARTESIAN_POINT ( 'NONE',  ( -54.07724161490514803, -276.1823704047750994, -345.2581368141795224 ) ) ;
#14647 = CARTESIAN_POINT ( 'NONE',  ( -64.53298115293586079, -181.9126970062073951, -359.6014539951557367 ) ) ;
#14648 = EDGE_CURVE ( 'NONE', #83649, #16441, #62679, .T. ) ;
#14649 = CARTESIAN_POINT ( 'NONE',  ( -110.2322170070427632, -297.6866161885311044, -293.3303853515508308 ) ) ;
#14650 = CARTESIAN_POINT ( 'NONE',  ( -110.4683760289727132, -275.2662352645559167, -253.7030783399848985 ) ) ;
#14651 = VERTEX_POINT ( 'NONE', #18873 ) ;
#14652 = LINE ( 'NONE', #43508, #60503 ) ;
#14653 = CARTESIAN_POINT ( 'NONE',  ( 2.603983725294459095, -287.6814839605490306, -208.8910568579802316 ) ) ;
#14654 = CARTESIAN_POINT ( 'NONE',  ( -91.20075834010039273, -287.0593250282994973, -216.7591043892576010 ) ) ;
#14655 = CARTESIAN_POINT ( 'NONE',  ( 1.358523951712914846, -287.8686694867816982, -332.3787390613808270 ) ) ;
#14656 = CARTESIAN_POINT ( 'NONE',  ( 34.52778608834048413, -281.4077939202252878, -297.8257107174369480 ) ) ;
#14657 = VECTOR ( 'NONE', #16929, 999.9999999999998863 ) ;
#14658 = CARTESIAN_POINT ( 'NONE',  ( -81.75323389522249329, -277.8361285208745244, -211.3558378910683757 ) ) ;
#14659 = CARTESIAN_POINT ( 'NONE',  ( -98.38491818626364704, -286.9915617413628297, -228.0942186496788509 ) ) ;
#14660 = CARTESIAN_POINT ( 'NONE',  ( -107.0947715153733242, -277.3468587693894847, -246.4302481829213320 ) ) ;
#14661 = CARTESIAN_POINT ( 'NONE',  ( -98.04679154264975693, -279.2948238815476998, -311.7873820508854692 ) ) ;
#14662 = CARTESIAN_POINT ( 'NONE',  ( 32.57710391074181189, -276.3254649268246794, -291.6023598868629279 ) ) ;
#14663 = CARTESIAN_POINT ( 'NONE',  ( 19.32014905679930195, -287.0515246351829433, -321.9310498614780158 ) ) ;
#14664 = CARTESIAN_POINT ( 'NONE',  ( -35.89196866455500867, -283.8372655698961466, -347.1990541950656848 ) ) ;
#14665 = CARTESIAN_POINT ( 'NONE',  ( 39.64882686370275877, -282.0390317623076726, -269.9243541454740125 ) ) ;
#14666 = ORIENTED_EDGE ( 'NONE', *, *, #51127, .F. ) ;
#14667 = EDGE_LOOP ( 'NONE', ( #40791, #86707, #33545 ) ) ;
#14668 = DIRECTION ( 'NONE',  ( 0.000000000000000000, 0.000000000000000000, 1.000000000000000000 ) ) ;
#14669 = CARTESIAN_POINT ( 'NONE',  ( -31.89159190179160319, -290.8446213608816038, -345.9813543484453362 ) ) ;
#14670 = CARTESIAN_POINT ( 'NONE',  ( -110.7542129672360858, -289.5088822208843453, -248.8227514750625176 ) ) ;
#14671 = CARTESIAN_POINT ( 'NONE',  ( -106.5247456105528840, -271.9293649090562326, -246.3379070041839043 ) ) ;
#14672 = CARTESIAN_POINT ( 'NONE',  ( 29.39130356909437580, -292.4036454861914649, -232.1509229570749540 ) ) ;
#14673 = CARTESIAN_POINT ( 'NONE',  ( -110.3121900072888337, -288.8962913654746103, -280.7481921873157944 ) ) ;
#14674 = CARTESIAN_POINT ( 'NONE',  ( 29.66533389325711667, -291.3718119426521298, -238.8071165447032058 ) ) ;
#14675 = CARTESIAN_POINT ( 'NONE',  ( 8.238464385818897284, -289.6174307781887478, -327.8900594511158602 ) ) ;
#14676 = CARTESIAN_POINT ( 'NONE',  ( -20.19161114001083490, -291.3376638359845856, -345.3538533559490702 ) ) ;
#14677 = CARTESIAN_POINT ( 'NONE',  ( 13.27326456308053970, -290.3449888223296398, -325.7770311679109909 ) ) ;
#14678 = CARTESIAN_POINT ( 'NONE',  ( -44.69180684110243362, -289.9593064400704634, -195.5030100218429254 ) ) ;
#14679 = CARTESIAN_POINT ( 'NONE',  ( -112.0355377871429567, -292.6462531215783542, -263.0450503807348355 ) ) ;
#14680 = CARTESIAN_POINT ( 'NONE',  ( -110.1051012436151808, -285.3785214281243725, -279.0982878643101230 ) ) ;
#14681 = CARTESIAN_POINT ( 'NONE',  ( 0.7485623503338053597, -294.5586054161193488, -205.5007167355416300 ) ) ;
#14682 = CARTESIAN_POINT ( 'NONE',  ( 201.2509219214787777, 65.09645894983574976, -2.633798379906725273 ) ) ;
#14683 = CARTESIAN_POINT ( 'NONE',  ( 138.6539576904058606, 249.5000000000000568, -10.49999999999999822 ) ) ;
#14684 = CARTESIAN_POINT ( 'NONE',  ( 6.911740759338740325, -300.5221789476098024, -194.7867625352656091 ) ) ;
#14685 = CARTESIAN_POINT ( 'NONE',  ( 34.86127483211399181, -280.9046857088136449, -282.1650213229119117 ) ) ;
#14686 = CARTESIAN_POINT ( 'NONE',  ( -105.9529299669932669, -282.1552425056159450, -300.6513769083413763 ) ) ;
#14687 = CARTESIAN_POINT ( 'NONE',  ( -94.53822927535699705, -295.0515271794511136, -321.6907221965095687 ) ) ;
#14688 = CARTESIAN_POINT ( 'NONE',  ( 21.50061224621594747, -273.1690913463195329, -225.4453017140346844 ) ) ;
#14689 = CARTESIAN_POINT ( 'NONE',  ( -110.0071900377795231, -276.8416971055762019, -254.1460980003063526 ) ) ;
#14690 = CARTESIAN_POINT ( 'NONE',  ( -86.44211597670678771, -298.6682237016093495, -215.6766353540418208 ) ) ;
#14691 = CARTESIAN_POINT ( 'NONE',  ( -31.28850420442002545, -272.7018945833042380, -194.1773066328008213 ) ) ;
#14692 = CARTESIAN_POINT ( 'NONE',  ( 34.79048186211772986, -294.7867466033989672, -255.7898023258425724 ) ) ;
#14693 = CARTESIAN_POINT ( 'NONE',  ( 41.08708295871279859, -293.9068999365417199, -430.6442049081568939 ) ) ;
#14694 = CARTESIAN_POINT ( 'NONE',  ( 16.28444113704671281, -295.0687007466637510, -320.1289660382206534 ) ) ;
#14695 = CARTESIAN_POINT ( 'NONE',  ( 198.6884013828325521, 64.61450673763175701, 9.555809373750797420 ) ) ;
#14697 = CARTESIAN_POINT ( 'NONE',  ( -102.5323343252196366, -296.9993750490144748, -237.3976725173052387 ) ) ;
#14696 = CARTESIAN_POINT ( 'NONE',  ( -26.82516625758425732, -284.2052313124946750, -195.6910057279293369 ) ) ;
#14698 = CARTESIAN_POINT ( 'NONE',  ( -114.3266410319141357, -284.5927567678380115, -267.1144071126789754 ) ) ;
#14699 = CARTESIAN_POINT ( 'NONE',  ( 25.53028977124331078, -286.6306813682153347, -225.9215329488652912 ) ) ;
#14700 = CARTESIAN_POINT ( 'NONE',  ( 7.801986856872882292, -290.6701741160864003, -210.6779884661212634 ) ) ;
#14701 = ADVANCED_FACE ( 'NONE', ( #32614 ), #83712, .T. ) ;
#14702 = CARTESIAN_POINT ( 'NONE',  ( -42.40917472496116147, -279.1869394266634004, -193.6898748610606447 ) ) ;
#14703 = EDGE_CURVE ( 'NONE', #11375, #13609, #26358, .T. ) ;
#14704 = CARTESIAN_POINT ( 'NONE',  ( -114.2704648735229114, -276.0523547857347353, -270.3284710469133074 ) ) ;
#14705 = CARTESIAN_POINT ( 'NONE',  ( 140.6539576904058606, 131.0000000000000568, 12.50000000000000000 ) ) ;
#14706 = CARTESIAN_POINT ( 'NONE',  ( 34.90987780542751295, -286.5165429661380472, -283.2777735735420492 ) ) ;
#14708 = DIRECTION ( 'NONE',  ( 0.000000000000000000, 0.000000000000000000, 1.000000000000000000 ) ) ;
#14707 = CARTESIAN_POINT ( 'NONE',  ( -71.78003240611128888, -288.4169604927631099, -338.8847911248911373 ) ) ;
#14709 = DIRECTION ( 'NONE',  ( 0.000000000000000000, 0.000000000000000000, 1.000000000000000000 ) ) ;
#14710 = CARTESIAN_POINT ( 'NONE',  ( -102.1603456800654470, -297.6758759337017182, -305.6454431441087536 ) ) ;
#14711 = CARTESIAN_POINT ( 'NONE',  ( -36.77529057724611050, -281.4844069552212886, -193.9394985469993742 ) ) ;
#14713 = CARTESIAN_POINT ( 'NONE',  ( 25.57509289597656021, -281.7289783874593923, -307.5226576701639942 ) ) ;
#14712 = CARTESIAN_POINT ( 'NONE',  ( -103.7910480535068700, -295.0428250785489581, -234.7133177948825278 ) ) ;
#14714 = CARTESIAN_POINT ( 'NONE',  ( 15.48022856860141871, -294.4963516356596074, -326.3865037755567187 ) ) ;
#14715 = CARTESIAN_POINT ( 'NONE',  ( 32.53720705406479397, -285.2582028480800886, -241.4797112760513471 ) ) ;
#14716 = CARTESIAN_POINT ( 'NONE',  ( -53.35885485968260866, -281.8470233110237473, -197.0382460943236254 ) ) ;
#14717 = CARTESIAN_POINT ( 'NONE',  ( -66.90336041185956617, -296.7137356709977780, -203.3435394562554279 ) ) ;
#14718 = ORIENTED_EDGE ( 'NONE', *, *, #54121, .F. ) ;
#14719 = DIRECTION ( 'NONE',  ( -1.000000000000000000, 0.000000000000000000, 0.000000000000000000 ) ) ;
#14720 = CARTESIAN_POINT ( 'NONE',  ( -7.821063966410090273, -284.6432783730629694, -338.9204269455259464 ) ) ;
#14721 = LINE ( 'NONE', #28914, #50446 ) ;
#14722 = CARTESIAN_POINT ( 'NONE',  ( -54.49178911615187104, -286.7666405000204009, -345.3538533559490702 ) ) ;
#14723 = CARTESIAN_POINT ( 'NONE',  ( 39.46152690502968596, -274.7955078877226924, -274.0464369994128901 ) ) ;
#14724 = CARTESIAN_POINT ( 'NONE',  ( -79.52897508416512551, -291.2980185364006047, -210.7237132508768127 ) ) ;
#14725 = CARTESIAN_POINT ( 'NONE',  ( 22.38512852578466195, -283.6706928002748782, -313.5500070594430895 ) ) ;
#14726 = CARTESIAN_POINT ( 'NONE',  ( 1.011003716962067145, -276.1734422399819096, -207.3094683400648535 ) ) ;
#14727 = CARTESIAN_POINT ( 'NONE',  ( 23.62739151063188814, -283.7669727043859211, -316.0689978515228518 ) ) ;
#14728 = CARTESIAN_POINT ( 'NONE',  ( 34.61694634458199005, -280.5376183216969821, -284.8840297448066394 ) ) ;
#14729 = CARTESIAN_POINT ( 'NONE',  ( -92.41974689240720409, -279.8399450613550243, -321.3425179418276798 ) ) ;
#14730 = CARTESIAN_POINT ( 'NONE',  ( -34.75943534448137484, -298.0836462427581637, -193.3611179409975591 ) ) ;
#14731 = CARTESIAN_POINT ( 'NONE',  ( 28.50364904711516800, -274.8632677669531290, -230.3418931644260681 ) ) ;
#14732 = CARTESIAN_POINT ( 'NONE',  ( 36.13136501124787969, -295.3165694703349118, -258.3223507771058394 ) ) ;
#14733 = DIRECTION ( 'NONE',  ( 0.000000000000000000, 0.000000000000000000, 1.000000000000000000 ) ) ;
#14734 = DIRECTION ( 'NONE',  ( 0.000000000000000000, 1.000000000000000000, 0.000000000000000000 ) ) ;
#14735 = CARTESIAN_POINT ( 'NONE',  ( -36.31533462420337344, -293.1790403635137636, -346.1318633065986887 ) ) ;
#14736 = CARTESIAN_POINT ( 'NONE',  ( -16.61720812348815812, -273.8347603314010144, -200.2477907273416804 ) ) ;
#14737 = CARTESIAN_POINT ( 'NONE',  ( -4.916502636190464237, -293.9915233032718334, -201.2864169476227403 ) ) ;
#14739 = CARTESIAN_POINT ( 'NONE',  ( -42.04499282550026606, -293.1991759095635075, -193.9027125799210012 ) ) ;
#14738 = CARTESIAN_POINT ( 'NONE',  ( -54.42813229853333468, -279.7662352645560304, -345.3683826091709648 ) ) ;
#14740 = CARTESIAN_POINT ( 'NONE',  ( -73.21590917287862510, -291.5291735430358244, -336.0350820297179553 ) ) ;
#14741 = CARTESIAN_POINT ( 'NONE',  ( -92.33193978249501299, -275.8402696384227966, -321.1918373651718639 ) ) ;
#14742 = CARTESIAN_POINT ( 'NONE',  ( -6.896772956942379906, -278.5695899812970424, -338.2906447746437948 ) ) ;
#14743 = CARTESIAN_POINT ( 'NONE',  ( 13.31729013591951549, -292.4172663218649291, -324.9751306684927386 ) ) ;
#14744 = CARTESIAN_POINT ( 'NONE',  ( 36.12758844938015557, -283.1772059113966407, -251.8524951396767335 ) ) ;
#14745 = ORIENTED_EDGE ( 'NONE', *, *, #8476, .T. ) ;
#14746 = CARTESIAN_POINT ( 'NONE',  ( 15.83834964011666990, -281.9397405518457163, -320.4737450861345565 ) ) ;
#14747 = CARTESIAN_POINT ( 'NONE',  ( -7.669334412943259238, -281.5117166814559937, -199.6288191039427602 ) ) ;
#14748 = CARTESIAN_POINT ( 'NONE',  ( -93.15281200929155148, -282.6270664633530032, -322.8506155782857263 ) ) ;
#14749 = CARTESIAN_POINT ( 'NONE',  ( -104.7631951829051076, -279.0169628438342215, -307.0648264724873115 ) ) ;
#14750 =( NAMED_UNIT ( * ) SI_UNIT ( $, .STERADIAN. ) SOLID_ANGLE_UNIT ( ) );
#14751 = CARTESIAN_POINT ( 'NONE',  ( 35.06585357261640468, -276.7644866612782266, -246.1145303415782735 ) ) ;
#14752 = CARTESIAN_POINT ( 'NONE',  ( -37.37352853689063181, -288.5519495502701375, -200.3611179825600459 ) ) ;
#14753 = ORIENTED_EDGE ( 'NONE', *, *, #59618, .F. ) ;
#14754 = CARTESIAN_POINT ( 'NONE',  ( -42.01780419505228537, -299.9933605374345689, -195.5070285774019112 ) ) ;
#14755 = B_SPLINE_CURVE_WITH_KNOTS ( 'NONE', 3,
 ( #22546, #51885, #29674, #58555, #18598, #2181 ),
 .UNSPECIFIED., .F., .F.,
 ( 4, 2, 4 ),
 ( 0.0006758717013506051769, 0.002293237004444498642, 0.003910602307538392323 ),
 .UNSPECIFIED. ) ;
#14756 = CARTESIAN_POINT ( 'NONE',  ( -111.8112106427697228, -276.4971519770018062, -276.1826063638703204 ) ) ;
#14757 = CARTESIAN_POINT ( 'NONE',  ( -79.05709251131023052, -293.2584519606065214, -206.7860050813560235 ) ) ;
#14758 = CARTESIAN_POINT ( 'NONE',  ( 16.81927857615029964, -292.1975518639670781, -221.1902152464070639 ) ) ;
#14759 = CARTESIAN_POINT ( 'NONE',  ( -113.1103257176929446, -290.2270975042544592, -256.9954051471577259 ) ) ;
#14760 = CARTESIAN_POINT ( 'NONE',  ( 209.1119202906403984, 36.79962757498938686, 13.15430387672353163 ) ) ;
#14762 = CARTESIAN_POINT ( 'NONE',  ( -100.2810557584299715, -283.4784496777049299, -231.7270852882678867 ) ) ;
#14761 = CARTESIAN_POINT ( 'NONE',  ( -1.002512906155358596, -293.1542530978201171, -337.5924762793551963 ) ) ;
#14763 = CARTESIAN_POINT ( 'NONE',  ( -84.63385005270421857, -293.2528883724849038, -213.1394609550296479 ) ) ;
#14764 = CARTESIAN_POINT ( 'NONE',  ( -44.06857364976190183, -284.4454302669668664, -196.9754455050674267 ) ) ;
#14765 = CARTESIAN_POINT ( 'NONE',  ( -13.35267622803792165, -284.0493021278487049, -339.8828531023201549 ) ) ;
#14766 = CARTESIAN_POINT ( 'NONE',  ( -69.24853949100405259, -290.4029732288698256, -340.1950767248400780 ) ) ;
#14767 = CARTESIAN_POINT ( 'NONE',  ( -3.125819734950805895, -281.0093317473082948, -205.7925953410922091 ) ) ;
#14768 = CARTESIAN_POINT ( 'NONE',  ( 37.67619781785987243, -292.1513893729710389, -254.7943891658774760 ) ) ;
#14769 = CARTESIAN_POINT ( 'NONE',  ( -41.74107220276406593, -289.9090497843407093, -347.0867908904371006 ) ) ;
#14770 = CARTESIAN_POINT ( 'NONE',  ( 39.03027521805085343, -288.1665080889038677, -280.1091622905239547 ) ) ;
#14771 = CARTESIAN_POINT ( 'NONE',  ( -67.54963498449838255, -285.8111233478732061, -203.9045105139182965 ) ) ;
#14772 = VERTEX_POINT ( 'NONE', #55790 ) ;
#14773 = CARTESIAN_POINT ( 'NONE',  ( 175.2296996224750103, 275.0000000000000568, 0.000000000000000000 ) ) ;
#14774 = CARTESIAN_POINT ( 'NONE',  ( 38.37337241005804600, -295.4474545257387490, -273.1057980142564361 ) ) ;
#14775 = CARTESIAN_POINT ( 'NONE',  ( -64.10943491397799221, -294.0790027931365671, -342.0324975348340786 ) ) ;
#14776 = CARTESIAN_POINT ( 'NONE',  ( -102.3592740409991961, -278.0691540720724788, -236.5443515814337729 ) ) ;
#14777 = CARTESIAN_POINT ( 'NONE',  ( -114.2799287340801158, -272.0957458231548571, -267.4896894357692076 ) ) ;
#14778 = CARTESIAN_POINT ( 'NONE',  ( -66.34365821927771378, -293.9188012278380597, -338.1076616619154720 ) ) ;
#14779 = CARTESIAN_POINT ( 'NONE',  ( 19.09544620236716028, -277.9837771567024447, -318.2445444438492359 ) ) ;
#14780 = CARTESIAN_POINT ( 'NONE',  ( -109.7342660377521497, -270.9049628485799985, -253.9239076013647320 ) ) ;
#14781 = CARTESIAN_POINT ( 'NONE',  ( 18.77028751652482441, -294.0886343375929073, -223.0475327406124393 ) ) ;
#14782 = CARTESIAN_POINT ( 'NONE',  ( -100.4254895946988455, -297.1196362108358358, -307.8062092200646589 ) ) ;
#14783 = DIRECTION ( 'NONE',  ( -0.000000000000000000, -1.000000000000000000, -0.000000000000000000 ) ) ;
#14784 = CARTESIAN_POINT ( 'NONE',  ( -112.2906034502529167, -294.6334884781005599, -263.9996424628623117 ) ) ;
#14785 = CARTESIAN_POINT ( 'NONE',  ( -70.69234694344012837, -298.2751821990243570, -201.0715289794235900 ) ) ;
#14786 = CARTESIAN_POINT ( 'NONE',  ( -84.46649122563921708, -275.4034827066340085, -212.0151266066184235 ) ) ;
#14787 = CARTESIAN_POINT ( 'NONE',  ( -106.2499222435548489, -291.1641629305350989, -295.1616295242016577 ) ) ;
#14788 = CARTESIAN_POINT ( 'NONE',  ( -82.36951343899568201, -296.0193558748632086, -327.9110894352050991 ) ) ;
#14789 = CARTESIAN_POINT ( 'NONE',  ( -112.4078610844074717, -280.6236121945696596, -263.1959479991191415 ) ) ;
#14790 = CARTESIAN_POINT ( 'NONE',  ( -111.6031672020957473, -277.4692574168315673, -251.9081571855818993 ) ) ;
#14791 = CARTESIAN_POINT ( 'NONE',  ( 9.140588080326475406, -281.7810914984025885, -331.6204819131916679 ) ) ;
#14792 = CARTESIAN_POINT ( 'NONE',  ( 18.82308612344793985, -275.6180919769613524, -322.8856795886061946 ) ) ;
#14793 = CARTESIAN_POINT ( 'NONE',  ( -72.10256061430081331, -281.5954978469592902, -336.1866204754747400 ) ) ;
#14794 = CARTESIAN_POINT ( 'NONE',  ( -47.98665536977560464, -278.3189190905283681, -194.8550325238680330 ) ) ;
#14795 = CARTESIAN_POINT ( 'NONE',  ( 7.474386834444151972, -278.6611978139957273, -209.9511716035584072 ) ) ;
#14796 = CARTESIAN_POINT ( 'NONE',  ( -97.27526463676956325, -295.8269545473135054, -227.8262931449855273 ) ) ;
#14797 = CARTESIAN_POINT ( 'NONE',  ( 20.43589238840171873, -278.2124272923527997, -318.2007428124951502 ) ) ;
#14798 = CARTESIAN_POINT ( 'NONE',  ( 197.7953982265470927, 19.09807621135326272, -10.91506350946106885 ) ) ;
#14799 = CARTESIAN_POINT ( 'NONE',  ( 33.90591496058647181, -291.2543755690602438, -245.6635697208846523 ) ) ;
#14800 = CARTESIAN_POINT ( 'NONE',  ( -113.1333019889379443, -290.3812843703086060, -284.0235685012721092 ) ) ;
#14801 = CARTESIAN_POINT ( 'NONE',  ( 23.81996640873066085, -276.9591021996823201, -226.6438118749740624 ) ) ;
#14802 = CARTESIAN_POINT ( 'NONE',  ( -91.35184219392029092, -295.2819183494752906, -218.4899523001131172 ) ) ;
#14803 = ADVANCED_FACE ( 'NONE', ( #39671 ), #48662, .T. ) ;
#14804 = CARTESIAN_POINT ( 'NONE',  ( -113.4409205647635446, -283.6113440162257575, -281.3706060883149007 ) ) ;
#14805 = CARTESIAN_POINT ( 'NONE',  ( 204.6539576904058606, 293.9636489450775230, 0.000000000000000000 ) ) ;
#14806 = CARTESIAN_POINT ( 'NONE',  ( -96.61789992795272042, -281.9218930005891934, -316.3308250677001183 ) ) ;
#14807 = FACE_OUTER_BOUND ( 'NONE', #30810, .T. ) ;
#14808 = CARTESIAN_POINT ( 'NONE',  ( 4.743815059678500035, -291.4292168696130716, -210.1661205989241807 ) ) ;
#14809 = CARTESIAN_POINT ( 'NONE',  ( -107.6954548529433708, -283.0030790125842373, -246.5103426102602384 ) ) ;
#14810 = DIRECTION ( 'NONE',  ( 0.8786741093294601068, 0.000000000000000000, 0.4774220455677345987 ) ) ;
#14811 = CARTESIAN_POINT ( 'NONE',  ( 157.3397966316789507, 16.44589409474725272, -9.145321187104729077 ) ) ;
#14812 = CARTESIAN_POINT ( 'NONE',  ( -30.60257476703284496, -290.1372171987408706, -195.6644993311574581 ) ) ;
#14813 = CARTESIAN_POINT ( 'NONE',  ( -65.01892186425033060, -281.8871162181939098, -341.4855263138263126 ) ) ;
#14814 = CARTESIAN_POINT ( 'NONE',  ( -83.49132363877386354, -279.2968838335467012, -328.0172618089705452 ) ) ;
#14815 = CARTESIAN_POINT ( 'NONE',  ( -111.9763485445742077, -285.9741187170923240, -253.1077711664929666 ) ) ;
#14816 = CARTESIAN_POINT ( 'NONE',  ( -71.17822123322197569, -285.5923384798751954, -205.6765770202761701 ) ) ;
#14817 = CARTESIAN_POINT ( 'NONE',  ( -102.3691914221685693, -279.5119057565265734, -304.8110859297080992 ) ) ;
#14818 = CARTESIAN_POINT ( 'NONE',  ( -108.6413301881170526, -279.1383884904341812, -286.8167415670671971 ) ) ;
#14819 = CARTESIAN_POINT ( 'NONE',  ( -109.5586269592996871, -286.2919024084290527, -290.6025638230204891 ) ) ;
#14820 = AXIS2_PLACEMENT_3D ( 'NONE', #10486, #1536, #38446 ) ;
#14821 = ORIENTED_EDGE ( 'NONE', *, *, #679, .F. ) ;
#14822 = CARTESIAN_POINT ( 'NONE',  ( -113.6014641939272281, -296.5198734781723715, -259.6145429405056007 ) ) ;
#14823 = CARTESIAN_POINT ( 'NONE',  ( 23.31260991251044246, -290.1268068552267891, -313.8686055902316525 ) ) ;
#14824 = CYLINDRICAL_SURFACE ( 'NONE', #24617, 1.000000000000000888 ) ;
#14825 = CARTESIAN_POINT ( 'NONE',  ( 36.60358173371528068, -278.4805209788416391, -305.9350535429201159 ) ) ;
#14826 = ORIENTED_EDGE ( 'NONE', *, *, #63185, .T. ) ;
#14827 = CARTESIAN_POINT ( 'NONE',  ( 22.49270005178255616, -291.3141389837169868, -223.1567353524231407 ) ) ;
#14828 = CARTESIAN_POINT ( 'NONE',  ( 25.53227725579910157, -288.5476298815528935, -231.9219358955942596 ) ) ;
#14829 = CARTESIAN_POINT ( 'NONE',  ( -109.2798108946321918, -280.5387685725110600, -252.9576058188420689 ) ) ;
#14830 = CARTESIAN_POINT ( 'NONE',  ( 37.25370945427000891, -289.1868351347378621, -286.9778211760788054 ) ) ;
#14831 = CARTESIAN_POINT ( 'NONE',  ( -3.265240683244684305, -289.9268033375313962, -338.8745095060730250 ) ) ;
#14832 = CARTESIAN_POINT ( 'NONE',  ( -79.47984415947874481, -285.6214919268298900, -332.4044694729619778 ) ) ;
#14833 = CARTESIAN_POINT ( 'NONE',  ( -110.5503471914902747, -279.0209539291169563, -246.3278015985067384 ) ) ;
#14834 = VERTEX_POINT ( 'NONE', #18390 ) ;
#14835 = CARTESIAN_POINT ( 'NONE',  ( -22.40654436401687732, -292.9421965613617544, -344.4303782564640528 ) ) ;
#14836 = CARTESIAN_POINT ( 'NONE',  ( 17.22461029268343324, -280.6376626442193469, -215.9584780100617536 ) ) ;
#14837 = CARTESIAN_POINT ( 'NONE',  ( -63.76821030538676638, -275.5643605123421480, -200.9751732569491480 ) ) ;
#14838 = FACE_OUTER_BOUND ( 'NONE', #91034, .T. ) ;
#14839 = CARTESIAN_POINT ( 'NONE',  ( -95.99890600148557951, -293.6948066931273615, -223.6242672951989618 ) ) ;
#14840 = CARTESIAN_POINT ( 'NONE',  ( -52.32360105921783600, -272.1028482312019037, -195.8123186308396555 ) ) ;
#14841 = CARTESIAN_POINT ( 'NONE',  ( 208.4306832106270804, -199.2391364535880882, -6.499999999999977796 ) ) ;
#14842 = CARTESIAN_POINT ( 'NONE',  ( -102.2076343630536712, -278.5179866330135496, -236.6296216210916157 ) ) ;
#14843 = CARTESIAN_POINT ( 'NONE',  ( 39.15681735701561195, -276.6954857365176963, -265.4498619058410895 ) ) ;
#14844 = CARTESIAN_POINT ( 'NONE',  ( -97.37384333853346163, -298.5669582364377561, -227.7992019136804345 ) ) ;
#14845 = CARTESIAN_POINT ( 'NONE',  ( -113.9742949977663642, -283.5440592715557386, -275.6894695110132716 ) ) ;
#14846 = CARTESIAN_POINT ( 'NONE',  ( -87.39844968253277102, -291.5215233255315184, -324.9493900710586445 ) ) ;
#14847 = CARTESIAN_POINT ( 'NONE',  ( -34.10323442049305243, -299.6121161593194415, -194.0536266358848820 ) ) ;
#14848 = CARTESIAN_POINT ( 'NONE',  ( -40.43964752190774448, -299.2192245205288259, -193.7690007450092935 ) ) ;
#14849 = CARTESIAN_POINT ( 'NONE',  ( -45.26002190593178653, -297.1527124863017661, -344.8260905709048529 ) ) ;
#14850 = CARTESIAN_POINT ( 'NONE',  ( -66.04179726966926012, -281.4284039956132801, -339.4860786965474517 ) ) ;
#14851 = CARTESIAN_POINT ( 'NONE',  ( -77.15469256056981351, -291.2009771039146244, -204.4158835851181379 ) ) ;
#14852 = CARTESIAN_POINT ( 'NONE',  ( -91.37011123717476835, -271.2988866390000453, -218.8373026335324312 ) ) ;
#14853 = CARTESIAN_POINT ( 'NONE',  ( -30.97125657269966226, -287.7314797219319189, -194.4147152786025003 ) ) ;
#14854 = CARTESIAN_POINT ( 'NONE',  ( -94.35331839890713468, -288.8234033255558302, -316.4469233550374270 ) ) ;
#14855 = CARTESIAN_POINT ( 'NONE',  ( -20.78800910493833953, -109.0397813191330840, -362.5271799116017064 ) ) ;
#14856 = VERTEX_POINT ( 'NONE', #69993 ) ;
#14857 = CARTESIAN_POINT ( 'NONE',  ( -110.9790243079734466, -288.8693395513073483, -290.7608920363040284 ) ) ;
#14858 = CARTESIAN_POINT ( 'NONE',  ( -84.70196802366683642, -289.3924907514538631, -326.0074665535559575 ) ) ;
#14859 = VERTEX_POINT ( 'NONE', #4191 ) ;
#14860 = CARTESIAN_POINT ( 'NONE',  ( -35.17081953721390875, -287.1584438759344380, -193.6878694151492937 ) ) ;
#14861 = CARTESIAN_POINT ( 'NONE',  ( -19.00753910479205544, -277.1428452809773262, -341.0431243650499482 ) ) ;
#14862 = CARTESIAN_POINT ( 'NONE',  ( 37.76506609359885402, -292.6672036442209901, -285.8680899183771658 ) ) ;
#14863 = CARTESIAN_POINT ( 'NONE',  ( -70.41874318633490759, -284.1281262113888033, -339.7961764470020967 ) ) ;
#14864 = CARTESIAN_POINT ( 'NONE',  ( 24.55632322577920590, -283.6695539827626362, -315.0077657658079602 ) ) ;
#14865 = CARTESIAN_POINT ( 'NONE',  ( -47.24943568301077335, -283.5080511325226666, -346.6997128585537666 ) ) ;
#14866 = CARTESIAN_POINT ( 'NONE',  ( -6.764438461699285199, -280.7982115897678455, -204.0366961401643948 ) ) ;
#14867 = CARTESIAN_POINT ( 'NONE',  ( -113.6816706259712220, -273.8610821628187750, -284.1793481324285722 ) ) ;
#14868 = CARTESIAN_POINT ( 'NONE',  ( 198.6360497827117513, 289.4354249690432539, -97.31417216244363999 ) ) ;
#14869 = CARTESIAN_POINT ( 'NONE',  ( -112.7803442879496032, -270.5759482646675451, -270.3359561730730434 ) ) ;
#14870 = CARTESIAN_POINT ( 'NONE',  ( -93.89669983061651237, -272.4055451961618246, -223.9288858873298977 ) ) ;
#14871 = CARTESIAN_POINT ( 'NONE',  ( -39.11271196219436064, -294.5814751962054743, -347.2791940151172412 ) ) ;
#14872 = CARTESIAN_POINT ( 'NONE',  ( 122.2538704333025805, 147.2434944315820644, -260.5076579305660402 ) ) ;
#14873 = CARTESIAN_POINT ( 'NONE',  ( -87.69910126009085616, -272.0511269554788214, -212.6935573124585801 ) ) ;
#14874 = CARTESIAN_POINT ( 'NONE',  ( -111.0275985750256069, -298.2903148450803883, -279.7857737810234084 ) ) ;
#14875 = CARTESIAN_POINT ( 'NONE',  ( 34.47436211061453548, -288.6627780919735073, -254.7503305551154256 ) ) ;
#14876 = ORIENTED_EDGE ( 'NONE', *, *, #69834, .T. ) ;
#14877 = CARTESIAN_POINT ( 'NONE',  ( -8.465390047287353781, -295.6246563919564778, -341.5439308367457443 ) ) ;
#14878 = CARTESIAN_POINT ( 'NONE',  ( -2.162255260902521847, -287.0231850229944826, -206.2700285039655910 ) ) ;
#14879 = CARTESIAN_POINT ( 'NONE',  ( -83.38349125174104870, -272.3583117319657276, -208.9624029320040961 ) ) ;
#14880 = CARTESIAN_POINT ( 'NONE',  ( -24.92381222732600676, -295.7005895693181401, -346.2435282884025582 ) ) ;
#14881 = CARTESIAN_POINT ( 'NONE',  ( 19.48846531651184577, -294.7508599749521636, -322.3025787969735916 ) ) ;
#14882 = CARTESIAN_POINT ( 'NONE',  ( -52.37184258195792097, -292.0210930969362266, -198.8732677104928541 ) ) ;
#14883 = EDGE_LOOP ( 'NONE', ( #16371, #71606, #28625, #60726 ) ) ;
#14884 = CARTESIAN_POINT ( 'NONE',  ( -102.9907636591982794, -274.9686288757571901, -232.8459701381500224 ) ) ;
#14885 = CARTESIAN_POINT ( 'NONE',  ( 19.75024487983085564, -273.6501420795791546, -219.2094889890695413 ) ) ;
#14886 = ORIENTED_EDGE ( 'NONE', *, *, #6237, .F. ) ;
#14887 = CARTESIAN_POINT ( 'NONE',  ( -84.52424538857647462, -278.9300216042117881, -209.5208926071358064 ) ) ;
#14888 = CARTESIAN_POINT ( 'NONE',  ( 5.659244314338219617, -273.0450854044192965, -210.3199547955777007 ) ) ;
#14889 = CARTESIAN_POINT ( 'NONE',  ( -62.14716549262230672, -274.8015128918820551, -201.3762286118088412 ) ) ;
#14890 = CARTESIAN_POINT ( 'NONE',  ( 23.98400156855259269, -275.9404525566801567, -230.3290463462648745 ) ) ;
#14891 = CARTESIAN_POINT ( 'NONE',  ( -29.18694711724390345, -299.7527560072383039, -194.1589351109550705 ) ) ;
#14892 = CARTESIAN_POINT ( 'NONE',  ( 18.63805300244820273, -274.2721810933783217, -320.8251831716453921 ) ) ;
#14893 = CARTESIAN_POINT ( 'NONE',  ( -77.99955609782713850, -296.2656886075365037, -331.1744680234588714 ) ) ;
#14894 = CARTESIAN_POINT ( 'NONE',  ( -37.01098419482438828, -293.6226248903224132, -343.9621299455653798 ) ) ;
#14895 = CARTESIAN_POINT ( 'NONE',  ( -109.6767582881953729, -278.7113859919203378, -296.7307906927459840 ) ) ;
#14896 = CARTESIAN_POINT ( 'NONE',  ( 30.17400937081869827, -275.3451828110256088, -242.4681892881451688 ) ) ;
#14897 = CARTESIAN_POINT ( 'NONE',  ( -107.4673622681433471, -283.6309704386822546, -239.6396735085565695 ) ) ;
#14898 = CARTESIAN_POINT ( 'NONE',  ( -106.6739170244196373, -298.1724354942691093, -299.5314257026497557 ) ) ;
#14899 = DIRECTION ( 'NONE',  ( -0.000000000000000000, -0.000000000000000000, -1.000000000000000000 ) ) ;
#14900 = CARTESIAN_POINT ( 'NONE',  ( -87.79849167931553211, -284.5219912584266240, -217.3826892305910974 ) ) ;
#14901 = EDGE_CURVE ( 'NONE', #89916, #85520, #53589, .T. ) ;
#14902 = CARTESIAN_POINT ( 'NONE',  ( -94.40138141946381722, -276.1327314016297123, -317.5208471865127535 ) ) ;
#14903 = CARTESIAN_POINT ( 'NONE',  ( -36.47731876809259433, -275.6158716797094144, -343.9578404526012037 ) ) ;
#14904 = CARTESIAN_POINT ( 'NONE',  ( -71.18510159373920487, -285.4989856455753738, -337.3051577066497657 ) ) ;
#14905 = CARTESIAN_POINT ( 'NONE',  ( -76.55506268344306875, -278.7943052725789812, -332.4647621242654054 ) ) ;
#14906 = CARTESIAN_POINT ( 'NONE',  ( 155.1244896729743061, 20.04296953158445405, 14.86678859757276427 ) ) ;
#14907 = CARTESIAN_POINT ( 'NONE',  ( 28.39540212061361757, -274.4589258740609807, -308.8977732851108726 ) ) ;
#14908 = CARTESIAN_POINT ( 'NONE',  ( -67.94987770663411197, -281.6514772247853102, -201.6945566625774404 ) ) ;
#14909 = EDGE_CURVE ( 'NONE', #57485, #37428, #50557, .T. ) ;
#14910 = DIRECTION ( 'NONE',  ( -0.000000000000000000, -0.000000000000000000, -1.000000000000000000 ) ) ;
#14911 = CARTESIAN_POINT ( 'NONE',  ( 22.16874578847162169, -290.1066633111701094, -316.9418243979674799 ) ) ;
#14912 = CARTESIAN_POINT ( 'NONE',  ( -20.75435260425014761, -290.2647829228209275, -197.1657367044340674 ) ) ;
#14913 = CARTESIAN_POINT ( 'NONE',  ( 82.16406924513974275, -298.3597564528348016, -196.9763042694495994 ) ) ;
#14914 = CARTESIAN_POINT ( 'NONE',  ( -103.6428112044271614, -271.6629357506310498, -238.6529779140942651 ) ) ;
#14915 = CARTESIAN_POINT ( 'NONE',  ( -80.22525522428877309, -289.6045552778905403, -209.7021980574301949 ) ) ;
#14916 = CARTESIAN_POINT ( 'NONE',  ( 201.9366853066881333, 285.6703355482916322, -112.9373754057687478 ) ) ;
#14917 = CARTESIAN_POINT ( 'NONE',  ( 98.97854452771385070, -297.7583178930348708, -195.4075969279095091 ) ) ;
#14918 = CARTESIAN_POINT ( 'NONE',  ( -72.86839492463008128, -287.9939380051652051, -337.9076741874630443 ) ) ;
#14919 = CARTESIAN_POINT ( 'NONE',  ( -37.52223829737051375, -284.6546140882725240, -344.1734651764551245 ) ) ;
#14920 = CARTESIAN_POINT ( 'NONE',  ( -84.86152418970716838, -283.6468349526077191, -211.0665960397071501 ) ) ;
#14921 = ADVANCED_FACE ( 'NONE', ( #39209 ), #68123, .T. ) ;
#14922 = CARTESIAN_POINT ( 'NONE',  ( -21.24176701983879312, -284.2669915878626625, -342.2200088793306350 ) ) ;
#14923 = CARTESIAN_POINT ( 'NONE',  ( -109.0893247005254665, -285.5433910475724133, -256.0474847739077404 ) ) ;
#14924 = CARTESIAN_POINT ( 'NONE',  ( -111.2497337784899827, -292.3433849835209912, -285.1236716151495330 ) ) ;
#14925 = CARTESIAN_POINT ( 'NONE',  ( -10.35900340810864684, -274.7279552595405789, -198.2094853670780310 ) ) ;
#14926 = CARTESIAN_POINT ( 'NONE',  ( -112.7491741434206602, -288.6931543503907847, -265.5624662647101104 ) ) ;
#14927 = CARTESIAN_POINT ( 'NONE',  ( 3.501501106008682029, -276.5194132478321194, -335.6989378172016245 ) ) ;
#14928 = CARTESIAN_POINT ( 'NONE',  ( 17.38175315535427146, -296.2455703932877782, -321.1271545024767420 ) ) ;
#14929 = CARTESIAN_POINT ( 'NONE',  ( -48.18343439339133027, -266.7963633757954085, -440.4292507799816576 ) ) ;
#14930 = CARTESIAN_POINT ( 'NONE',  ( -85.28047601435908120, -292.1948066931273615, -330.5268031993605859 ) ) ;
#14931 = CARTESIAN_POINT ( 'NONE',  ( 1.346770494103801230, -281.2087452807162435, -332.9060995216835863 ) ) ;
#14932 = CARTESIAN_POINT ( 'NONE',  ( -111.1901092267232798, -276.7324355051349585, -256.2766651246321317 ) ) ;
#14933 = CARTESIAN_POINT ( 'NONE',  ( -63.30285051703177146, -272.1998341367411740, -198.6064914934049739 ) ) ;
#14934 = CARTESIAN_POINT ( 'NONE',  ( 34.94369633539486841, -274.7560950019083634, -259.3812303385336122 ) ) ;
#14935 = CARTESIAN_POINT ( 'NONE',  ( 22.35509582956093055, -294.4732058097428649, -227.1308678496267248 ) ) ;
#14936 = CARTESIAN_POINT ( 'NONE',  ( 34.00737184365192434, -294.7112127627005407, -286.9305922991796933 ) ) ;
#14937 = CARTESIAN_POINT ( 'NONE',  ( 37.48119411981927840, -294.7813119015780217, -254.8005848664153916 ) ) ;
#14938 = CARTESIAN_POINT ( 'NONE',  ( 6.346222210225488602, -295.7879424278364127, -333.2322374880150733 ) ) ;
#14939 = CARTESIAN_POINT ( 'NONE',  ( -53.15144538113155193, -295.0937319614895387, -341.6805706454919118 ) ) ;
#14940 = CARTESIAN_POINT ( 'NONE',  ( -98.97842001112121579, -291.9725364729412149, -313.1144018941114382 ) ) ;
#14941 = CARTESIAN_POINT ( 'NONE',  ( -37.31212119221935808, -283.2184342017803260, -347.3741776089751738 ) ) ;
#14942 = CARTESIAN_POINT ( 'NONE',  ( -87.20533637919137959, -271.5059727849838964, -213.2482149604902304 ) ) ;
#14943 = CARTESIAN_POINT ( 'NONE',  ( 20.28816140619682784, -286.6930171452784748, -219.2157929538252858 ) ) ;
#14944 = CARTESIAN_POINT ( 'NONE',  ( -54.30372325327672911, -279.2508434928289489, -343.1064964808805939 ) ) ;
#14945 = CARTESIAN_POINT ( 'NONE',  ( -79.52501797105988146, -284.2633591061516540, -210.2346145330780871 ) ) ;
#14946 = AXIS2_PLACEMENT_3D ( 'NONE', #47120, #76968, #63261 ) ;
#14947 = CARTESIAN_POINT ( 'NONE',  ( -74.69040791796525980, -287.5491056504151857, -335.4001422358676905 ) ) ;
#14948 = CARTESIAN_POINT ( 'NONE',  ( -100.8428064840771583, -277.2444587217430580, -228.9393001400984247 ) ) ;
#14949 = CARTESIAN_POINT ( 'NONE',  ( 121.1498776811041438, 150.0802918209077177, -263.8330885344481658 ) ) ;
#14950 = CARTESIAN_POINT ( 'NONE',  ( 19.82209492063704204, -282.0620784621206667, -219.3481717810390137 ) ) ;
#14951 = CARTESIAN_POINT ( 'NONE',  ( -104.9544096972042553, -289.1394976908217131, -306.7113823151653378 ) ) ;
#14952 = CARTESIAN_POINT ( 'NONE',  ( -102.9069449596131562, -279.6399374951424193, -309.2928741573435900 ) ) ;
#14953 = CARTESIAN_POINT ( 'NONE',  ( -68.79721314374448582, -278.7722335525762674, -340.1167290000392427 ) ) ;
#14954 = CARTESIAN_POINT ( 'NONE',  ( -41.04906222738272703, -279.8375148345883190, -197.4553193737886261 ) ) ;
#14955 = CARTESIAN_POINT ( 'NONE',  ( -35.37162931937074717, -276.0568604820846303, -195.7295285254807311 ) ) ;
#14956 = CARTESIAN_POINT ( 'NONE',  ( 26.49290192793644039, -292.9837191468247397, -227.2075566129864228 ) ) ;
#14957 = CARTESIAN_POINT ( 'NONE',  ( -79.11532057194287404, -287.6383677775764909, -332.2845840338926564 ) ) ;
#14958 = CARTESIAN_POINT ( 'NONE',  ( -90.24533864937700400, -292.9194083385741010, -215.4458629062697241 ) ) ;
#14959 = CARTESIAN_POINT ( 'NONE',  ( -72.28397215722968383, -294.4462566618455526, -334.8212685081921336 ) ) ;
#14960 = CARTESIAN_POINT ( 'NONE',  ( 35.31681878442596911, -293.1165679105013737, -262.6038851894221011 ) ) ;
#14961 = CARTESIAN_POINT ( 'NONE',  ( -110.9394065383886812, -291.9033409344772281, -248.8002710330150364 ) ) ;
#14962 = CARTESIAN_POINT ( 'NONE',  ( 35.13272348906826892, -282.0727082826430205, -260.4273368241869093 ) ) ;
#14963 = CARTESIAN_POINT ( 'NONE',  ( -114.1064060109667651, -271.6110516640039805, -270.3491600855638239 ) ) ;
#14964 = CARTESIAN_POINT ( 'NONE',  ( -20.51062525802773351, -289.4930302992212887, -345.4492248958403025 ) ) ;
#14965 = CARTESIAN_POINT ( 'NONE',  ( -24.76237100262590829, -281.0330339411779050, -345.1275879789250212 ) ) ;
#14966 = CARTESIAN_POINT ( 'NONE',  ( -26.14344049597411868, -289.2465771672572146, -346.5211027033329287 ) ) ;
#14967 = CARTESIAN_POINT ( 'NONE',  ( -7.011593792237876599, -286.7947134366567070, -203.9232042942724945 ) ) ;
#14968 = DIRECTION ( 'NONE',  ( -1.000000000000000000, 1.124465274301078034E-16, 0.000000000000000000 ) ) ;
#14969 = CARTESIAN_POINT ( 'NONE',  ( -32.49014215546316819, -123.7434641620947957, -362.3882418532662086 ) ) ;
#14970 = CARTESIAN_POINT ( 'NONE',  ( -88.60724157838485837, -229.4615865740312302, -344.3535732501791813 ) ) ;
#14971 = CARTESIAN_POINT ( 'NONE',  ( -93.20689720124428845, -278.4194059840971818, -223.1011745418307726 ) ) ;
#14972 = CARTESIAN_POINT ( 'NONE',  ( -6.627414243512323999, -279.3854880942175214, -203.7827179562788160 ) ) ;
#14973 = CARTESIAN_POINT ( 'NONE',  ( -21.35503853749595038, -273.9185196053519462, -195.0605805168563904 ) ) ;
#14974 = CARTESIAN_POINT ( 'NONE',  ( 86.31154334970720754, 81.21865059938454579, -300.0628701344159026 ) ) ;
#14975 = CARTESIAN_POINT ( 'NONE',  ( -98.09673289820428010, -277.7496644967953330, -223.9994142220614890 ) ) ;
#14976 = CARTESIAN_POINT ( 'NONE',  ( -77.02237623229856922, -281.6063047001998143, -333.6463898800645325 ) ) ;
#14977 = CARTESIAN_POINT ( 'NONE',  ( 21.51614788923746957, -295.9661589534562722, -318.4411793381928533 ) ) ;
#14978 = CARTESIAN_POINT ( 'NONE',  ( 2.268601807664912151, -293.0905317938339749, -208.9089070657932155 ) ) ;
#14979 = CARTESIAN_POINT ( 'NONE',  ( -68.98538526581214114, -288.1620924613305306, -336.6930158191238434 ) ) ;
#14980 = CARTESIAN_POINT ( 'NONE',  ( -0.1020843505969328407, -275.1855965478910093, -203.0666997650090195 ) ) ;
#14981 = CARTESIAN_POINT ( 'NONE',  ( -95.60304813716530248, -296.1007189230272729, -314.3659716367945407 ) ) ;
#14982 = ORIENTED_EDGE ( 'NONE', *, *, #50431, .F. ) ;
#14983 = DIRECTION ( 'NONE',  ( 1.000000000000000000, 0.000000000000000000, 0.000000000000000000 ) ) ;
#14984 = CARTESIAN_POINT ( 'NONE',  ( 196.8928068234201021, 24.78327594025822478, 12.47839767815188061 ) ) ;
#14985 = CARTESIAN_POINT ( 'NONE',  ( -110.6940134173985228, -280.7040620972180136, -252.1764334608224658 ) ) ;
#14986 = CARTESIAN_POINT ( 'NONE',  ( -54.57875233172333651, -280.9052261001969555, -199.0548544606908479 ) ) ;
#14987 = CARTESIAN_POINT ( 'NONE',  ( 12.31284386041327394, -282.4926524108478247, -212.8424229979267182 ) ) ;
#14988 = CARTESIAN_POINT ( 'NONE',  ( 34.16757747435598702, -280.8187364540268049, -286.1671821891202967 ) ) ;
#14989 = CARTESIAN_POINT ( 'NONE',  ( -95.14460582801808641, -271.6710503333297311, -224.6497206361564452 ) ) ;
#14990 = DIRECTION ( 'NONE',  ( -1.000000000000000000, -0.000000000000000000, -0.000000000000000000 ) ) ;
#14991 = DIRECTION ( 'NONE',  ( -1.000000000000000000, 0.000000000000000000, 0.000000000000000000 ) ) ;
#14992 = CARTESIAN_POINT ( 'NONE',  ( 37.78534682813666024, -276.1520850359382848, -254.1717835756720376 ) ) ;
#14993 = FACE_OUTER_BOUND ( 'NONE', #59363, .T. ) ;
#14994 = CARTESIAN_POINT ( 'NONE',  ( 27.38314933737237666, -278.0586348467960534, -308.2516776032041435 ) ) ;
#14995 = CARTESIAN_POINT ( 'NONE',  ( -113.4935322293544715, -277.0399404809643897, -277.2596813832041676 ) ) ;
#14996 = ORIENTED_EDGE ( 'NONE', *, *, #71951, .T. ) ;
#14997 = CYLINDRICAL_SURFACE ( 'NONE', #27789, 3.842139515347647638 ) ;
#14998 = CARTESIAN_POINT ( 'NONE',  ( -110.1389918356320976, -286.7833694054314151, -250.6978230695078196 ) ) ;
#14999 = CARTESIAN_POINT ( 'NONE',  ( -62.84746493801604572, -290.9085685147545064, -201.7895663856133694 ) ) ;
#15000 = CARTESIAN_POINT ( 'NONE',  ( 30.04623942745260123, -286.4191271247048576, -233.2076839432773738 ) ) ;
#15001 = ADVANCED_FACE ( 'NONE', ( #75684 ), #5133, .F. ) ;
#15002 = CARTESIAN_POINT ( 'NONE',  ( -71.90164103808086793, -281.7554848245586641, -335.8102165222308031 ) ) ;
#15004 = CARTESIAN_POINT ( 'NONE',  ( 34.78987223875954982, -285.3933027309886938, -251.9152952440694264 ) ) ;
#15003 = CARTESIAN_POINT ( 'NONE',  ( -85.25908969992632080, -282.3042897298263938, -326.2118000926590753 ) ) ;
#15005 = CARTESIAN_POINT ( 'NONE',  ( 30.70838515815050584, -283.1235094390634686, -297.8623251642928267 ) ) ;
#15006 = CARTESIAN_POINT ( 'NONE',  ( 33.84007599325015292, -273.2447717854151392, -246.5719272808927656 ) ) ;
#15007 = CARTESIAN_POINT ( 'NONE',  ( -82.78230859198515645, -283.8426834486686516, -209.1267822330590889 ) ) ;
#15008 = CARTESIAN_POINT ( 'NONE',  ( -106.5201652567127013, -298.1724354960462051, -299.4667983817611798 ) ) ;
#15009 = CARTESIAN_POINT ( 'NONE',  ( -108.5211794547556394, -279.7200118655020447, -253.1306167810067222 ) ) ;
#15010 = CARTESIAN_POINT ( 'NONE',  ( -18.66283607850124682, -288.2921875825855409, -197.4984832830887456 ) ) ;
#15011 = CARTESIAN_POINT ( 'NONE',  ( 196.1162889029012319, 19.88370459728183448, 13.75220701793647926 ) ) ;
#15012 = LINE ( 'NONE', #34924, #23160 ) ;
#15013 = CARTESIAN_POINT ( 'NONE',  ( 22.81368772070251438, -294.8511037498579412, -224.6162796294288171 ) ) ;
#15014 = CARTESIAN_POINT ( 'NONE',  ( -84.27769824464698445, -275.6971742524810338, -328.9259482955554859 ) ) ;
#15015 = CARTESIAN_POINT ( 'NONE',  ( -31.84855113190473119, -288.1818026388085627, -347.0554853498662169 ) ) ;
#15016 = CARTESIAN_POINT ( 'NONE',  ( 24.01759222698796847, -291.3887566956260002, -229.3552933115682322 ) ) ;
#15017 = CARTESIAN_POINT ( 'NONE',  ( -110.8854857240149556, -277.2335365151951123, -270.6232096094690860 ) ) ;
#15018 = CARTESIAN_POINT ( 'NONE',  ( -97.08045603927816103, -295.2993886052756238, -226.2698743778591677 ) ) ;
#15019 = CARTESIAN_POINT ( 'NONE',  ( -9.556458195699242708, -293.7380232817252477, -202.2685764672799280 ) ) ;
#15020 = CARTESIAN_POINT ( 'NONE',  ( 21.27581636871892101, -283.4090924074130839, -223.5744983911110353 ) ) ;
#15021 = CARTESIAN_POINT ( 'NONE',  ( 24.31453355230742730, -292.6344332744985195, -315.3410633823395415 ) ) ;
#15022 = CARTESIAN_POINT ( 'NONE',  ( 35.92082104460875058, -289.2682972532041958, -279.2517538508241159 ) ) ;
#15023 = CARTESIAN_POINT ( 'NONE',  ( -111.5801897380402607, -288.5866415476621683, -286.5666934985757734 ) ) ;
#15024 = EDGE_CURVE ( 'NONE', #13683, #26669, #33933, .T. ) ;
#15025 = CARTESIAN_POINT ( 'NONE',  ( -50.84189352776427739, -290.6531517491407044, -342.7535163362921367 ) ) ;
#15026 = DIRECTION ( 'NONE',  ( 0.000000000000000000, 0.000000000000000000, 1.000000000000000000 ) ) ;
#15027 = CARTESIAN_POINT ( 'NONE',  ( -107.1029723889671459, -291.0614100677571514, -292.5732546423507188 ) ) ;
#15028 = DIRECTION ( 'NONE',  ( 0.000000000000000000, 0.000000000000000000, 1.000000000000000000 ) ) ;
#15029 = CARTESIAN_POINT ( 'NONE',  ( -29.00506106599234712, -290.1539274419343428, -346.5623112812566546 ) ) ;
#15030 = CARTESIAN_POINT ( 'NONE',  ( -5.613093777918063410, -278.4874904831101503, -202.0112654156020824 ) ) ;
#15031 = EDGE_CURVE ( 'NONE', #44024, #2170, #86844, .T. ) ;
#15032 = CARTESIAN_POINT ( 'NONE',  ( 32.00426472833874669, -280.7886414897344025, -236.8186949681834506 ) ) ;
#15033 = CARTESIAN_POINT ( 'NONE',  ( 25.21597841165944232, -284.9922498285788492, -228.8963127811026652 ) ) ;
#15034 = CARTESIAN_POINT ( 'NONE',  ( 36.36325840924525465, -279.8120422741844777, -279.6356725192413251 ) ) ;
#15035 = CARTESIAN_POINT ( 'NONE',  ( -68.92674225723072823, -283.6367567202963187, -202.3222366353230655 ) ) ;
#15036 = CARTESIAN_POINT ( 'NONE',  ( 139.3042674286450051, 178.0593505315339655, -238.4361928449195602 ) ) ;
#15037 = CARTESIAN_POINT ( 'NONE',  ( -110.7785769561892408, -276.7698706796314809, -291.0911173873932398 ) ) ;
#15038 = CARTESIAN_POINT ( 'NONE',  ( -101.1695466135648189, -282.9095998109747825, -312.9711149987672343 ) ) ;
#15039 = CARTESIAN_POINT ( 'NONE',  ( 94.93239848020441229, -300.6892790076082065, -197.1041445370088354 ) ) ;
#15040 = CARTESIAN_POINT ( 'NONE',  ( -33.48680555501966438, -293.7015803428286631, -196.6492336337761913 ) ) ;
#15041 = CARTESIAN_POINT ( 'NONE',  ( -55.21354456981067926, -275.2518910279451347, -196.0697761752051633 ) ) ;
#15042 = CARTESIAN_POINT ( 'NONE',  ( 5.405729127621107466, -276.1225488142885069, -329.6244407452855967 ) ) ;
#15043 = CARTESIAN_POINT ( 'NONE',  ( -23.11516070898414199, -296.8704908374231195, -344.0524863797014063 ) ) ;
#15044 = CARTESIAN_POINT ( 'NONE',  ( -6.917972340403921727, -288.8304841365395532, -341.1100513044441982 ) ) ;
#15045 = CARTESIAN_POINT ( 'NONE',  ( 30.73491404735966981, -279.2020239408659563, -237.4551676188944782 ) ) ;
#15046 = CARTESIAN_POINT ( 'NONE',  ( -25.01934905682688637, -292.0384784206648874, -194.3534889670114012 ) ) ;
#15047 = CARTESIAN_POINT ( 'NONE',  ( -81.86261354133968382, -290.4875955915459826, -212.1480359353932670 ) ) ;
#15048 = CARTESIAN_POINT ( 'NONE',  ( -64.89313275815500504, -293.4118216278505429, -340.1311137358343331 ) ) ;
#15049 = EDGE_LOOP ( 'NONE', ( #44650, #53933, #77996, #3449 ) ) ;
#15050 = CARTESIAN_POINT ( 'NONE',  ( 197.7152286749091559, 70.58179843880969884, 11.36775530991498506 ) ) ;
#15051 = CARTESIAN_POINT ( 'NONE',  ( -101.1743930792914057, -290.5466534028199135, -234.7132238697029152 ) ) ;
#15052 = CARTESIAN_POINT ( 'NONE',  ( 165.2494399300530290, -11.64849832608277325, 13.00000000000000178 ) ) ;
#15053 = CARTESIAN_POINT ( 'NONE',  ( -46.48938434906518324, -286.8799970140468076, -194.1434029421205878 ) ) ;
#15054 = CARTESIAN_POINT ( 'NONE',  ( -109.1418805571601069, -293.0519495502701943, -270.3937649182068412 ) ) ;
#15055 = CARTESIAN_POINT ( 'NONE',  ( 21.18047541082637508, -293.2826326623358568, -320.0398376101054509 ) ) ;
#15056 = CARTESIAN_POINT ( 'NONE',  ( 35.14725911861896179, -283.1793510136896543, -294.9931703800187961 ) ) ;
#15057 = CARTESIAN_POINT ( 'NONE',  ( -110.3904368893083188, -284.3782675227793106, -270.9071810373341691 ) ) ;
#15058 = CARTESIAN_POINT ( 'NONE',  ( 31.73096269163791661, -277.2013220914643057, -295.6130954307375873 ) ) ;
#15059 = CARTESIAN_POINT ( 'NONE',  ( -8.620803034927837061, -292.6945637510834217, -339.2731911420747792 ) ) ;
#15060 = CARTESIAN_POINT ( 'NONE',  ( 25.70887004303792267, -274.8608684744641550, -307.9344609968768509 ) ) ;
#15061 = ORIENTED_EDGE ( 'NONE', *, *, #67975, .F. ) ;
#15062 = DIRECTION ( 'NONE',  ( 1.000000000000000000, 0.000000000000000000, -0.000000000000000000 ) ) ;
#15063 = CARTESIAN_POINT ( 'NONE',  ( -44.79780244011147516, -294.8106668546647597, -347.0314196467380725 ) ) ;
#15064 = CARTESIAN_POINT ( 'NONE',  ( 34.41089179808677301, -289.2154550940693412, -250.5399234762938363 ) ) ;
#15065 = CARTESIAN_POINT ( 'NONE',  ( -79.29632203766676923, -296.6839561113782224, -334.5584871624771495 ) ) ;
#15066 = CARTESIAN_POINT ( 'NONE',  ( -42.68985327603825652, -286.6343449060184412, -197.4424398264602303 ) ) ;
#15067 = CARTESIAN_POINT ( 'NONE',  ( -70.21118042624624422, -276.5334392491919857, -339.7471019975104127 ) ) ;
#15068 = CARTESIAN_POINT ( 'NONE',  ( 8.851551046606893181, -295.0884493974060661, -331.8387263630948496 ) ) ;
#15069 = CARTESIAN_POINT ( 'NONE',  ( -68.86533399736563865, -287.6017585140245387, -339.2706389777469553 ) ) ;
#15070 = CIRCLE ( 'NONE', #92174, 5.000000000000004441 ) ;
#15071 = CARTESIAN_POINT ( 'NONE',  ( -112.5807388420076194, -297.0897328479682074, -254.0259377198101447 ) ) ;
#15072 = CARTESIAN_POINT ( 'NONE',  ( -34.86081443189331708, -292.4174554811343683, -197.3821299585684699 ) ) ;
#15073 = DIRECTION ( 'NONE',  ( 0.000000000000000000, 0.000000000000000000, -1.000000000000000000 ) ) ;
#15074 = FACE_OUTER_BOUND ( 'NONE', #6233, .T. ) ;
#15075 = CARTESIAN_POINT ( 'NONE',  ( 122.1069166414435188, 147.2784711290201471, -260.4370888796501049 ) ) ;
#15076 = AXIS2_PLACEMENT_3D ( 'NONE', #70242, #12952, #28542 ) ;
#15077 = CARTESIAN_POINT ( 'NONE',  ( 32.07319419917863712, -288.6620186997694191, -238.5436092288638008 ) ) ;
#15078 = CARTESIAN_POINT ( 'NONE',  ( -19.05039376806006857, -289.7666405000204009, -190.3683826091709363 ) ) ;
#15079 = VERTEX_POINT ( 'NONE', #25951 ) ;
#15080 = CARTESIAN_POINT ( 'NONE',  ( -11.53573798968777808, -279.7280760774544319, -197.8665084577066864 ) ) ;
#15081 = CARTESIAN_POINT ( 'NONE',  ( -10.28983966323379207, -284.6985922698972900, -340.1887215999643104 ) ) ;
#15082 = CARTESIAN_POINT ( 'NONE',  ( -78.19201225635383423, -284.0889241552297904, -205.7866780614738786 ) ) ;
#15083 = CARTESIAN_POINT ( 'NONE',  ( 8.854837899617368890, -286.4927039141430782, -328.7322929675459591 ) ) ;
#15084 = CARTESIAN_POINT ( 'NONE',  ( 0.5567041505140671864, -276.4120096259011916, -204.7410773755840410 ) ) ;
#15085 = CARTESIAN_POINT ( 'NONE',  ( -39.17615333602782357, -298.5208969413874911, -197.3101936461422099 ) ) ;
#15086 = CARTESIAN_POINT ( 'NONE',  ( 12.67833886840204194, -293.0221489522724596, -324.2754369872645839 ) ) ;
#15087 = CARTESIAN_POINT ( 'NONE',  ( -35.34699757052139546, -280.7279509746610415, -193.4758061816777115 ) ) ;
#15089 = CARTESIAN_POINT ( 'NONE',  ( -67.34054376307322798, -278.9966276392759141, -203.6844449848367162 ) ) ;
#15088 = CARTESIAN_POINT ( 'NONE',  ( 26.76675462052174836, -276.0300280861304714, -305.3824898953262732 ) ) ;
#15090 = CARTESIAN_POINT ( 'NONE',  ( 33.42299129710904992, -276.2528072928744791, -240.6630493985697115 ) ) ;
#15091 = CARTESIAN_POINT ( 'NONE',  ( -107.2997974446115279, -277.0681046019389555, -301.9126302051150788 ) ) ;
#15092 = CARTESIAN_POINT ( 'NONE',  ( -114.1313154040836650, -273.2851564102892326, -284.1365878591568617 ) ) ;
#15093 = CARTESIAN_POINT ( 'NONE',  ( 8.501874767114017573, -274.4246346221747217, -329.7838799706123041 ) ) ;
#15094 = EDGE_CURVE ( 'NONE', #82861, #24854, #33525, .T. ) ;
#15095 = CARTESIAN_POINT ( 'NONE',  ( -108.3478281756182611, -298.3398420032713148, -241.9923298175449986 ) ) ;
#15096 = CARTESIAN_POINT ( 'NONE',  ( 156.8306019976938046, 250.3431421874260252, 16.89650703080528515 ) ) ;
#15097 = CARTESIAN_POINT ( 'NONE',  ( 181.0595704366054690, 252.2700355933461651, -164.3583243123303532 ) ) ;
#15098 = CARTESIAN_POINT ( 'NONE',  ( 11.32905525087031329, -287.8249880494316244, -215.4715456183801336 ) ) ;
#15099 = CARTESIAN_POINT ( 'NONE',  ( -70.64263240357119855, -287.3791606541255987, -202.0601521967194287 ) ) ;
#15100 = CARTESIAN_POINT ( 'NONE',  ( -5.747091079040602679, -285.8274415608531740, -204.4255927919825240 ) ) ;
#15101 = CARTESIAN_POINT ( 'NONE',  ( -91.87437193537228097, -277.6573801885731427, -220.6355901185366122 ) ) ;
#15102 = CARTESIAN_POINT ( 'NONE',  ( -109.2306541176174051, -286.6529267508993257, -251.8450769067680994 ) ) ;
#15103 = CARTESIAN_POINT ( 'NONE',  ( -109.8104306148581912, -277.2068540914880259, -256.9823715791741847 ) ) ;
#15104 = CARTESIAN_POINT ( 'NONE',  ( -70.66151415100436850, -278.8163666521174378, -335.8670984182563188 ) ) ;
#15105 = CARTESIAN_POINT ( 'NONE',  ( 32.91746112377272482, -275.7775925708898512, -250.1394727498181680 ) ) ;
#15106 = CARTESIAN_POINT ( 'NONE',  ( 38.28046640983761506, -286.5047333481776377, -282.9019149496307364 ) ) ;
#15107 = CARTESIAN_POINT ( 'NONE',  ( 15.04375573756397344, -281.5713180107804874, -214.0752013055139287 ) ) ;
#15108 = CARTESIAN_POINT ( 'NONE',  ( 34.53225460434799743, -282.3923296939545935, -297.8140146280107388 ) ) ;
#15109 = EDGE_LOOP ( 'NONE', ( #64586, #69446, #34865, #39805 ) ) ;
#15110 = B_SPLINE_CURVE_WITH_KNOTS ( 'NONE', 3,
 ( #24954, #18304, #17848, #33439, #54744, #46241 ),
 .UNSPECIFIED., .F., .F.,
 ( 4, 2, 4 ),
 ( 0.000000000000000000, 0.001028964506245427356, 0.002057929012490854713 ),
 .UNSPECIFIED. ) ;
#15111 = VERTEX_POINT ( 'NONE', #91750 ) ;
#15112 = FACE_OUTER_BOUND ( 'NONE', #7241, .T. ) ;
#15113 = CARTESIAN_POINT ( 'NONE',  ( -92.67423654594335858, -291.6945329200743799, -322.1920477383625894 ) ) ;
#15114 = CARTESIAN_POINT ( 'NONE',  ( -75.43277900722347340, -288.2339815521284550, -336.7114607301139699 ) ) ;
#15115 = CARTESIAN_POINT ( 'NONE',  ( -67.88659909682871785, -297.0465831497848512, -340.1712144159924378 ) ) ;
#15116 = CARTESIAN_POINT ( 'NONE',  ( -37.81332025501148308, -297.2432611803557165, -197.2011610251920501 ) ) ;
#15117 = CARTESIAN_POINT ( 'NONE',  ( -61.64848547805958390, -291.0931490998294180, -197.3496199144815364 ) ) ;
#15118 = CARTESIAN_POINT ( 'NONE',  ( 25.55243892172937592, -285.5078758314507468, -231.9549332623005000 ) ) ;
#15119 = CARTESIAN_POINT ( 'NONE',  ( -18.35607478536340409, -290.0072445144078301, -341.3130515415115269 ) ) ;
#15120 = CARTESIAN_POINT ( 'NONE',  ( -110.4683760289727132, -293.2662352645559167, -253.7030783399848985 ) ) ;
#15121 = CARTESIAN_POINT ( 'NONE',  ( -45.77491134458503552, -291.1590929135921328, -344.9372332756022956 ) ) ;
#15122 = CARTESIAN_POINT ( 'NONE',  ( -38.90812818273636253, -287.0716063446362227, -345.5114655092765474 ) ) ;
#15123 = CARTESIAN_POINT ( 'NONE',  ( -38.03165292124556629, -291.0609193960547714, -345.3705491469568756 ) ) ;
#15124 = CARTESIAN_POINT ( 'NONE',  ( -106.3915783605032601, -285.1678883361105932, -294.9153939111548084 ) ) ;
#15125 = CARTESIAN_POINT ( 'NONE',  ( -58.44887042212440065, -293.7800610208776106, -198.2187879246360751 ) ) ;
#15126 = FACE_OUTER_BOUND ( 'NONE', #63166, .T. ) ;
#15127 = CARTESIAN_POINT ( 'NONE',  ( 133.0872704186301405, -299.5541904835127980, -188.7068768330456123 ) ) ;
#15128 = CARTESIAN_POINT ( 'NONE',  ( -95.67911939684735501, -275.1865666471322811, -222.6424180280208702 ) ) ;
#15129 = CARTESIAN_POINT ( 'NONE',  ( 35.68165889153419101, -280.6901700420580141, -265.8677045765517732 ) ) ;
#15130 = CARTESIAN_POINT ( 'NONE',  ( -77.21131527937788519, -281.5860396752066208, -333.9474617813671102 ) ) ;
#15131 = CARTESIAN_POINT ( 'NONE',  ( -65.55374574031428381, -294.6089562854335782, -341.8472586566103928 ) ) ;
#15132 = CARTESIAN_POINT ( 'NONE',  ( -38.07015221690794249, -272.2827592662044935, -196.3513660982877980 ) ) ;
#15133 = CARTESIAN_POINT ( 'NONE',  ( -5.686042623816032204, -274.7124529648054363, -337.7489897319943566 ) ) ;
#15134 = CARTESIAN_POINT ( 'NONE',  ( -97.29466702524970856, -298.4568777370442376, -227.8536452406141848 ) ) ;
#15135 = LINE ( 'NONE', #48894, #73055 ) ;
#15136 = CARTESIAN_POINT ( 'NONE',  ( -55.17833286309119956, -272.4018052091549862, -196.0613143222341250 ) ) ;
#15137 = CARTESIAN_POINT ( 'NONE',  ( -103.7286542139609651, -294.3051287464018628, -307.4382704674184197 ) ) ;
#15138 = CARTESIAN_POINT ( 'NONE',  ( 24.93551944878662496, -295.5157472086812618, -309.6604822016483354 ) ) ;
#15139 = CARTESIAN_POINT ( 'NONE',  ( 219.8344101925596021, 0.000000000000000000, -9.000000000000001776 ) ) ;
#15140 = CARTESIAN_POINT ( 'NONE',  ( -6.687959855693156541, -295.4419057846418468, -336.7911558780933206 ) ) ;
#15141 = AXIS2_PLACEMENT_3D ( 'NONE', #47856, #69653, #53581 ) ;
#15142 = CARTESIAN_POINT ( 'NONE',  ( 200.4738562182569694, 293.9636489450776367, -44.00000000000000000 ) ) ;
#15144 = CARTESIAN_POINT ( 'NONE',  ( -109.1421302913753664, -296.3773796871216746, -283.6098271359936689 ) ) ;
#15143 = CARTESIAN_POINT ( 'NONE',  ( -108.6759548807474545, -282.2595898787317310, -294.6475524849048497 ) ) ;
#15145 = CARTESIAN_POINT ( 'NONE',  ( -114.1518519013656885, -284.6286021544469804, -264.2482390723681647 ) ) ;
#15146 = CARTESIAN_POINT ( 'NONE',  ( -30.32383195700539247, -284.8841808350481983, -345.5945129873040855 ) ) ;
#15147 = AXIS2_PLACEMENT_3D ( 'NONE', #19397, #89947, #33596 ) ;
#15148 = CARTESIAN_POINT ( 'NONE',  ( 22.97796748170735626, -286.5784999961942958, -222.5145695767751590 ) ) ;
#15149 = CARTESIAN_POINT ( 'NONE',  ( -38.91111842682269639, -290.0322565442247083, -195.5442391632657007 ) ) ;
#15150 = CARTESIAN_POINT ( 'NONE',  ( -11.55389753143429843, -279.5766811162470162, -197.9232906108013026 ) ) ;
#15151 = CARTESIAN_POINT ( 'NONE',  ( 21.31550574532286291, -278.4094976428775681, -223.6242672951989618 ) ) ;
#15152 = CARTESIAN_POINT ( 'NONE',  ( 192.9623460957494956, 276.0000000000000568, 16.90571646082668522 ) ) ;
#15153 = CARTESIAN_POINT ( 'NONE',  ( 23.87367499471782750, -285.7872063392975406, -229.7745261804603558 ) ) ;
#15154 = EDGE_CURVE ( 'NONE', #92884, #84200, #84642, .T. ) ;
#15156 = CARTESIAN_POINT ( 'NONE',  ( 198.0747767758275870, 67.35440902555335185, -11.09512694806112698 ) ) ;
#15155 = CARTESIAN_POINT ( 'NONE',  ( -113.6976929224262136, -289.5692559804612074, -262.6542961799540308 ) ) ;
#15157 = DIRECTION ( 'NONE',  ( -0.000000000000000000, -1.000000000000000000, -0.000000000000000000 ) ) ;
#15158 = CARTESIAN_POINT ( 'NONE',  ( -111.1664840662578797, -280.2266880505036397, -250.5999620905804477 ) ) ;
#15160 = CARTESIAN_POINT ( 'NONE',  ( -4.334214791337673844, -280.1663689781372568, -205.2120293380274347 ) ) ;
#15159 = CARTESIAN_POINT ( 'NONE',  ( -55.69461930861432108, -293.3073680560329990, -343.4472121274324081 ) ) ;
#15161 = CARTESIAN_POINT ( 'NONE',  ( -69.52598625362830376, -295.6308246069863799, -340.3267605181873705 ) ) ;
#15162 = CARTESIAN_POINT ( 'NONE',  ( 33.51256270610736010, -285.2938291448624000, -244.1125440293015458 ) ) ;
#15163 = EDGE_CURVE ( 'NONE', #70449, #60290, #91272, .T. ) ;
#15164 = CARTESIAN_POINT ( 'NONE',  ( -85.53946260179677097, -281.3861835382718368, -212.8305810109754361 ) ) ;
#15165 = CARTESIAN_POINT ( 'NONE',  ( -108.7036198770296238, -295.8273178367575156, -253.9025378886643409 ) ) ;
#15166 = VERTEX_POINT ( 'NONE', #77091 ) ;
#15167 = CARTESIAN_POINT ( 'NONE',  ( 201.2849759805909571, 65.05171340438639049, -7.254661561165801409 ) ) ;
#15168 = CARTESIAN_POINT ( 'NONE',  ( -79.28039158902841166, -285.6012269008483599, -332.1105548955749782 ) ) ;
#15169 = DIRECTION ( 'NONE',  ( 0.000000000000000000, -0.000000000000000000, 1.000000000000000000 ) ) ;
#15170 = CARTESIAN_POINT ( 'NONE',  ( 35.78497577281001440, -290.8380690714490129, -253.7030783399848985 ) ) ;
#15171 = CARTESIAN_POINT ( 'NONE',  ( -27.00809219693016772, -273.3773799382550465, -194.1673019692075286 ) ) ;
#15172 = CARTESIAN_POINT ( 'NONE',  ( -83.82740409146008176, -291.2261186226832592, -214.0754241384555883 ) ) ;
#15173 = CARTESIAN_POINT ( 'NONE',  ( 36.38051391880737384, -283.0485808111613437, -268.5473783609551219 ) ) ;
#15174 = CARTESIAN_POINT ( 'NONE',  ( -32.66042078798253812, -275.7122325980164419, -196.6970725281209127 ) ) ;
#15175 = CARTESIAN_POINT ( 'NONE',  ( -60.96410810636794508, -284.9537285270282041, -342.8622135639787984 ) ) ;
#15176 = CARTESIAN_POINT ( 'NONE',  ( 17.89361162317399945, -281.0330107919604075, -318.6952761040914766 ) ) ;
#15177 = CARTESIAN_POINT ( 'NONE',  ( -110.8524918838389226, -280.7440893845216010, -255.4249316866856248 ) ) ;
#15178 = CARTESIAN_POINT ( 'NONE',  ( -114.3417789856397206, -272.7546669925150127, -267.4957702519898248 ) ) ;
#15179 = VERTEX_POINT ( 'NONE', #19793 ) ;
#15180 = CARTESIAN_POINT ( 'NONE',  ( -52.54354444183928052, -273.6960529915692177, -194.8222157423174963 ) ) ;
#15181 = CARTESIAN_POINT ( 'NONE',  ( 36.72557489202645797, -295.3696400451231625, -262.4245545433521443 ) ) ;
#15182 = LINE ( 'NONE', #85739, #89891 ) ;
#15183 = DIRECTION ( 'NONE',  ( -1.000000000000000000, 0.000000000000000000, 0.000000000000000000 ) ) ;
#15184 = CARTESIAN_POINT ( 'NONE',  ( 35.18033417861960999, -291.9735157018828886, -292.4671728409064144 ) ) ;
#15185 = CARTESIAN_POINT ( 'NONE',  ( 19.05034733944065906, -274.4020271799920465, -223.9076420708660464 ) ) ;
#15186 = CARTESIAN_POINT ( 'NONE',  ( -1.149923282487198328, -294.0436351797982297, -203.1832716152183309 ) ) ;
#15188 = CARTESIAN_POINT ( 'NONE',  ( -69.47069151011361043, -292.8437452892238753, -200.8073884647353680 ) ) ;
#15187 = CARTESIAN_POINT ( 'NONE',  ( 10.64812456238590066, -284.9090924074130271, -330.4860931364851808 ) ) ;
#15189 = CARTESIAN_POINT ( 'NONE',  ( 9.138077453083853996, -290.4123875631011060, -329.0097215410813192 ) ) ;
#15190 = CARTESIAN_POINT ( 'NONE',  ( 30.81377120221815247, -273.9582843033544464, -301.2619294799239356 ) ) ;
#15191 = CARTESIAN_POINT ( 'NONE',  ( -83.88849966740357900, -279.6168580128189092, -328.5196936287024982 ) ) ;
#15192 = CARTESIAN_POINT ( 'NONE',  ( 24.10814507329684275, -292.2063990126723638, -312.4658663561411345 ) ) ;
#15193 = CARTESIAN_POINT ( 'NONE',  ( 37.56973689817415618, -283.2641227162248470, -258.6821395268172523 ) ) ;
#15194 = ORIENTED_EDGE ( 'NONE', *, *, #83604, .F. ) ;
#15195 = CARTESIAN_POINT ( 'NONE',  ( -42.93877096930648207, -282.7913153760666205, -343.2175393619461374 ) ) ;
#15196 = CARTESIAN_POINT ( 'NONE',  ( -36.76872702404064341, -281.1388620501670061, -193.6593761586896676 ) ) ;
#15197 = CARTESIAN_POINT ( 'NONE',  ( -44.39800356312578344, -281.9343242565125252, -346.6914404667514873 ) ) ;
#15198 = CARTESIAN_POINT ( 'NONE',  ( -67.60478041881619049, -278.3808782455269011, -340.9087344180882724 ) ) ;
#15199 = DIRECTION ( 'NONE',  ( 1.000000000000000000, 0.000000000000000000, 0.000000000000000000 ) ) ;
#15200 = CARTESIAN_POINT ( 'NONE',  ( 10.11018211553916935, -277.9319559669725663, -330.1866714896522694 ) ) ;
#15201 = VECTOR ( 'NONE', #29265, 1000.000000000000000 ) ;
#15202 = CARTESIAN_POINT ( 'NONE',  ( -105.5937364680635966, -293.2662352645559167, -254.8156830097664738 ) ) ;
#15203 = EDGE_LOOP ( 'NONE', ( #142, #22664, #47855, #3328, #71908 ) ) ;
#15204 = ORIENTED_EDGE ( 'NONE', *, *, #7831, .T. ) ;
#15205 = CARTESIAN_POINT ( 'NONE',  ( -111.4008184333346065, -274.6950462627561365, -259.2695261873302002 ) ) ;
#15206 = AXIS2_PLACEMENT_3D ( 'NONE', #88270, #45167, #75471 ) ;
#15207 = CARTESIAN_POINT ( 'NONE',  ( -77.25617295882872781, -275.6098506058735893, -333.4987112014621857 ) ) ;
#15208 = CARTESIAN_POINT ( 'NONE',  ( -112.8044270791010604, -292.1939099488014335, -279.7022446076493907 ) ) ;
#15209 = CARTESIAN_POINT ( 'NONE',  ( 28.48273147314468190, -293.3318477017017472, -302.2746340421704758 ) ) ;
#15210 = CARTESIAN_POINT ( 'NONE',  ( -12.24972785872560621, -288.2420591111903150, -343.1487780468973483 ) ) ;
#15211 = CARTESIAN_POINT ( 'NONE',  ( 129.4467878515196162, -299.5541904835127980, -192.3225193827704516 ) ) ;
#15213 = CARTESIAN_POINT ( 'NONE',  ( -56.54650048823933162, -281.7037129241570597, -341.6185109766022947 ) ) ;
#15212 = CARTESIAN_POINT ( 'NONE',  ( 25.22169536677001034, -292.7117216417075838, -314.2522465222793357 ) ) ;
#15214 = CARTESIAN_POINT ( 'NONE',  ( -39.97847150189620180, -290.9459225210188720, -344.5998935871107847 ) ) ;
#15215 = CARTESIAN_POINT ( 'NONE',  ( -107.1832547316018918, -283.3433181230396940, -246.6883776761474394 ) ) ;
#15216 = CARTESIAN_POINT ( 'NONE',  ( -26.65462342375412064, -284.2286824502753575, -343.1247307671146132 ) ) ;
#15217 = CARTESIAN_POINT ( 'NONE',  ( -109.6398879997262270, -291.1649302301790385, -296.3215886702050170 ) ) ;
#15218 = CARTESIAN_POINT ( 'NONE',  ( 35.58089727719877260, -281.9851412922354257, -265.8574273658376796 ) ) ;
#15219 = CARTESIAN_POINT ( 'NONE',  ( -30.64104909141789079, -293.7641350407864707, -346.6704227500508750 ) ) ;
#15220 = CARTESIAN_POINT ( 'NONE',  ( 16.17937307715149942, -287.5914534149048336, -215.2280648914523624 ) ) ;
#15221 = CARTESIAN_POINT ( 'NONE',  ( 38.22855990177499308, -287.8636958294777060, -255.9159560789599368 ) ) ;
#15222 = CARTESIAN_POINT ( 'NONE',  ( -93.25646967994852332, -285.3852928549603689, -223.4299071470096294 ) ) ;
#15223 = VERTEX_POINT ( 'NONE', #17932 ) ;
#15224 = CARTESIAN_POINT ( 'NONE',  ( 194.9478318536113477, 25.16799831920036823, 13.68273651490584975 ) ) ;
#15225 = CARTESIAN_POINT ( 'NONE',  ( -39.05576025648635863, -296.9338577699517714, -346.1065302623649131 ) ) ;
#15226 = CARTESIAN_POINT ( 'NONE',  ( -92.35411657558167065, -294.5039483130847771, -323.5300215732144125 ) ) ;
#15227 = CARTESIAN_POINT ( 'NONE',  ( -100.7926649505992032, -277.1098693812487568, -307.0332514468245222 ) ) ;
#15228 = CARTESIAN_POINT ( 'NONE',  ( -36.53361470600247429, -297.4106111465627009, -193.4631366652685358 ) ) ;
#15229 = CARTESIAN_POINT ( 'NONE',  ( 27.76159930737323123, -292.4992830571406444, -304.9993451199967467 ) ) ;
#15230 = CARTESIAN_POINT ( 'NONE',  ( -16.37477079689389825, -276.0868861471752780, -199.3262642550542125 ) ) ;
#15231 = CARTESIAN_POINT ( 'NONE',  ( -90.76194001227179342, -295.5218988998871623, -219.0603444925297083 ) ) ;
#15232 = CARTESIAN_POINT ( 'NONE',  ( 21.65473534918080034, -295.3661067126975013, -314.0251891018666583 ) ) ;
#15233 = CARTESIAN_POINT ( 'NONE',  ( 24.69614967220579516, -295.1702020146665859, -309.5145514576460073 ) ) ;
#15234 = CARTESIAN_POINT ( 'NONE',  ( -43.48180805801840165, -254.5884423091092117, -445.2610164474263001 ) ) ;
#15235 = CARTESIAN_POINT ( 'NONE',  ( -111.0849887327953667, -294.7393583508400638, -255.7363352942988968 ) ) ;
#15236 = CARTESIAN_POINT ( 'NONE',  ( -112.3426482175930232, -274.5879229896262359, -267.5880413896982759 ) ) ;
#15237 = CARTESIAN_POINT ( 'NONE',  ( -70.06685188145638676, -290.4354718463557674, -335.8919867721832588 ) ) ;
#15238 = CARTESIAN_POINT ( 'NONE',  ( -93.09579115647140668, -296.2152653224621872, -317.5352197962346850 ) ) ;
#15239 = CARTESIAN_POINT ( 'NONE',  ( -110.2299268573743234, -280.2868485705914168, -289.5353831041932722 ) ) ;
#15240 = CARTESIAN_POINT ( 'NONE',  ( -36.73950691828656545, -278.7444045972972617, -193.8436745294311550 ) ) ;
#15241 = CARTESIAN_POINT ( 'NONE',  ( 35.96295379401282588, -275.1931366905004666, -293.5934338363402389 ) ) ;
#15242 = CARTESIAN_POINT ( 'NONE',  ( -33.44482177080126206, -281.0825913060816106, -344.7118733701401538 ) ) ;
#15243 = CARTESIAN_POINT ( 'NONE',  ( -111.3044303039521026, -277.1843491475054293, -251.9785694830478633 ) ) ;
#15244 = CARTESIAN_POINT ( 'NONE',  ( -50.59085277116972179, -277.8831487169188108, -196.3713323494931444 ) ) ;
#15245 = CARTESIAN_POINT ( 'NONE',  ( -98.85119200914509463, -295.7917788416601752, -230.0468487854578541 ) ) ;
#15246 = CARTESIAN_POINT ( 'NONE',  ( -0.6409153747703357773, -276.5398619184994118, -204.9397115528984727 ) ) ;
#15247 = CARTESIAN_POINT ( 'NONE',  ( 170.2296700125738198, 215.0000000000000568, -24.97289011430693151 ) ) ;
#15248 = CARTESIAN_POINT ( 'NONE',  ( -104.5259899121446239, -289.0225677856435595, -236.1187607721205097 ) ) ;
#15249 = CARTESIAN_POINT ( 'NONE',  ( -37.50159019729269971, -289.0540657626553980, -347.3740238018522177 ) ) ;
#15250 = CARTESIAN_POINT ( 'NONE',  ( 26.92160825705013494, -277.0297592119269439, -231.2712117033388495 ) ) ;
#15251 = CARTESIAN_POINT ( 'NONE',  ( -96.16592741527880150, -271.1910895173010658, -223.8346638131558564 ) ) ;
#15252 = CARTESIAN_POINT ( 'NONE',  ( -112.9798667870211659, -283.5761080244857908, -284.1822007142310440 ) ) ;
#15253 = CARTESIAN_POINT ( 'NONE',  ( 129.9467878515196162, -299.5541904835127980, -190.0176033293537898 ) ) ;
#15254 = CARTESIAN_POINT ( 'NONE',  ( -108.4072419239234364, -282.2401706353770692, -294.4920533174262118 ) ) ;
#15255 = CARTESIAN_POINT ( 'NONE',  ( 201.2104617360081704, 25.32700003806617772, 9.999999999999998224 ) ) ;
#15256 = CARTESIAN_POINT ( 'NONE',  ( 35.10835770291462410, -292.1918442871239563, -258.5299957570583160 ) ) ;
#15257 = CARTESIAN_POINT ( 'NONE',  ( -111.6266230412442440, -282.6848041490763421, -270.8949300268375850 ) ) ;
#15258 = DIRECTION ( 'NONE',  ( 0.000000000000000000, 0.000000000000000000, 1.000000000000000000 ) ) ;
#15259 = DIRECTION ( 'NONE',  ( 0.000000000000000000, -1.000000000000000000, 0.000000000000000000 ) ) ;
#15260 = CARTESIAN_POINT ( 'NONE',  ( 23.44011677327116416, -290.9534921397819289, -226.4010016420293141 ) ) ;
#15261 = CARTESIAN_POINT ( 'NONE',  ( 38.72214182766492030, -279.9552676791909107, -264.2783802516528908 ) ) ;
#15262 = CARTESIAN_POINT ( 'NONE',  ( -109.2613332816082590, -279.9355551561741891, -286.9702070352231544 ) ) ;
#15263 = CARTESIAN_POINT ( 'NONE',  ( -110.7231671646470659, -285.4794281973779562, -292.3877419741945118 ) ) ;
#15264 = CARTESIAN_POINT ( 'NONE',  ( -59.97862926585872856, -285.7504573797669991, -200.9596090709286784 ) ) ;
#15265 = CARTESIAN_POINT ( 'NONE',  ( -61.97006126762443046, -278.8038369874677755, -339.7609340238977325 ) ) ;
#15266 = CARTESIAN_POINT ( 'NONE',  ( -96.21687980577205224, -278.7473453197708295, -313.8138406829186806 ) ) ;
#15267 = EDGE_CURVE ( 'NONE', #13153, #64177, #50151, .T. ) ;
#15268 = CARTESIAN_POINT ( 'NONE',  ( -82.10319740870546923, -287.4423929183736846, -210.1181951469412468 ) ) ;
#15269 = ORIENTED_EDGE ( 'NONE', *, *, #56521, .F. ) ;
#15270 = CYLINDRICAL_SURFACE ( 'NONE', #8964, 4.999999999999990230 ) ;
#15271 = CARTESIAN_POINT ( 'NONE',  ( -108.3758626312435354, -296.0059437428294586, -300.2169273489993770 ) ) ;
#15273 = CARTESIAN_POINT ( 'NONE',  ( -59.14603817337341951, -291.3154852591933945, -341.8043035169222890 ) ) ;
#15272 = AXIS2_PLACEMENT_3D ( 'NONE', #57470, #44149, #78768 ) ;
#15274 = CARTESIAN_POINT ( 'NONE',  ( 197.0527519259912879, 24.77614581236855074, 12.20486921435629846 ) ) ;
#15275 = CARTESIAN_POINT ( 'NONE',  ( -2.602324593224680793, -279.1233781216987495, -342.4248175857292154 ) ) ;
#15276 = CARTESIAN_POINT ( 'NONE',  ( -73.60728612800370740, -278.5027566370227987, -202.7718266797550086 ) ) ;
#15277 = CARTESIAN_POINT ( 'NONE',  ( 38.70227000252714333, -292.0232930154083419, -276.0004507890507170 ) ) ;
#15278 = VECTOR ( 'NONE', #9930, 1000.000000000000000 ) ;
#15279 = CARTESIAN_POINT ( 'NONE',  ( 33.69247261578643560, -288.8154876329008403, -250.7434204568437224 ) ) ;
#15280 = CARTESIAN_POINT ( 'NONE',  ( -39.75644186291612669, -281.7815878370878977, -196.3744897734738117 ) ) ;
#15281 = CARTESIAN_POINT ( 'NONE',  ( 0.4438376529203304499, -289.9845874673037542, -336.8352177782438162 ) ) ;
#15282 = CARTESIAN_POINT ( 'NONE',  ( -74.77346948222938749, -285.5501706056037392, -335.4115457415587116 ) ) ;
#15283 = CARTESIAN_POINT ( 'NONE',  ( -72.83879534774986553, -277.6758520821545062, -338.7055825328710057 ) ) ;
#15284 = VERTEX_POINT ( 'NONE', #78960 ) ;
#15285 = CARTESIAN_POINT ( 'NONE',  ( -71.19139132135998693, -295.6232275710356134, -203.8183655436061201 ) ) ;
#15286 = CARTESIAN_POINT ( 'NONE',  ( 38.00696136140724235, -291.5600222558498444, -264.7136931131582287 ) ) ;
#15287 = CARTESIAN_POINT ( 'NONE',  ( -95.90442668975327933, -279.0599880909725243, -220.3467968669700383 ) ) ;
#15288 = CARTESIAN_POINT ( 'NONE',  ( -27.14354467667562432, -276.0434319117055111, -196.7779845342168699 ) ) ;
#15289 = CARTESIAN_POINT ( 'NONE',  ( 200.7454649163835541, 299.8601228333361632, -5.413818927456778951 ) ) ;
#15290 = CARTESIAN_POINT ( 'NONE',  ( -95.95921662488163406, -292.4090924074130839, -317.1477375740089997 ) ) ;
#15291 = CARTESIAN_POINT ( 'NONE',  ( -13.36076094935486402, -272.5992579032717913, -198.2577992766572947 ) ) ;
#15292 = DIRECTION ( 'NONE',  ( -1.000000000000000000, 0.000000000000000000, 0.000000000000000000 ) ) ;
#15293 = CARTESIAN_POINT ( 'NONE',  ( -34.30449879329485441, -279.5989798356156939, -197.3501814333233710 ) ) ;
#15294 = CARTESIAN_POINT ( 'NONE',  ( 38.34587447068880550, -276.9098398718295471, -282.5012231946375323 ) ) ;
#15295 = CARTESIAN_POINT ( 'NONE',  ( -39.20126651060222400, -299.4536711487753564, -196.7828771459608106 ) ) ;
#15296 = CARTESIAN_POINT ( 'NONE',  ( -110.8860107189336759, -283.3334469468297812, -292.4080287477763704 ) ) ;
#15297 = CARTESIAN_POINT ( 'NONE',  ( 32.36115072820064142, -289.6391468290395323, -295.2506056222009647 ) ) ;
#15298 = CARTESIAN_POINT ( 'NONE',  ( -109.2044732964808134, -298.3991135533725014, -244.7008454915571463 ) ) ;
#15299 = CARTESIAN_POINT ( 'NONE',  ( -37.62169158028348903, -299.2537886864762413, -193.7587007532200971 ) ) ;
#15300 = CARTESIAN_POINT ( 'NONE',  ( 2.568612614507656655, -296.5163127457378209, -333.7249134376760935 ) ) ;
#15301 = CARTESIAN_POINT ( 'NONE',  ( -6.521108790400147015, -280.6463450114713964, -338.5669586333523853 ) ) ;
#15302 = CARTESIAN_POINT ( 'NONE',  ( -32.56106000304422565, -272.1327900334985088, -195.8567510946501784 ) ) ;
#15303 = CARTESIAN_POINT ( 'NONE',  ( -78.11181243102357996, -287.1138372120078657, -205.9853589015050375 ) ) ;
#15304 = CARTESIAN_POINT ( 'NONE',  ( -61.36924932555739076, -288.2920254633450554, -339.6207956664441667 ) ) ;
#15305 = CARTESIAN_POINT ( 'NONE',  ( -108.6012104099982309, -267.5897348884550979, -306.9379130596528285 ) ) ;
#15306 = ORIENTED_EDGE ( 'NONE', *, *, #8208, .F. ) ;
#15307 = CARTESIAN_POINT ( 'NONE',  ( 35.38135276139608720, -286.4240771481159982, -293.8124264979344389 ) ) ;
#15308 = CARTESIAN_POINT ( 'NONE',  ( 28.24489232128960481, -287.6535754220393528, -302.4623076420973575 ) ) ;
#15309 = ORIENTED_EDGE ( 'NONE', *, *, #77753, .F. ) ;
#15310 = CARTESIAN_POINT ( 'NONE',  ( -111.4262223471554734, -285.8832941003722681, -250.3377617016133172 ) ) ;
#15311 = CARTESIAN_POINT ( 'NONE',  ( -11.24252134828827820, -277.0357179091452053, -338.5587744950851743 ) ) ;
#15312 = CARTESIAN_POINT ( 'NONE',  ( 20.15609093970152443, -291.7823411424012079, -219.5919233574116163 ) ) ;
#15313 = CARTESIAN_POINT ( 'NONE',  ( 35.22872891725126010, -281.8805532111661023, -244.7689692592749964 ) ) ;
#15314 = CARTESIAN_POINT ( 'NONE',  ( -1.478564221311180482, -282.0390073533935720, -203.0072521920707231 ) ) ;
#15315 = CARTESIAN_POINT ( 'NONE',  ( -98.02513364858326383, -284.2524103414684191, -317.7242385281491579 ) ) ;
#15316 = CARTESIAN_POINT ( 'NONE',  ( -11.73971030273082228, -280.7280505131478208, -201.9217884051330145 ) ) ;
#15317 = CARTESIAN_POINT ( 'NONE',  ( -89.88738572736605192, -230.7286653867029713, -347.9689446550020193 ) ) ;
#15318 = CARTESIAN_POINT ( 'NONE',  ( -81.89087134799066803, -279.6609526076622387, -330.4893124272986142 ) ) ;
#15319 = CARTESIAN_POINT ( 'NONE',  ( -49.19496325650769109, -154.3339921397289913, -364.3446390947307805 ) ) ;
#15320 = CARTESIAN_POINT ( 'NONE',  ( -106.7427607202974542, -259.6958249236880647, -315.6408438834064327 ) ) ;
#15321 = CARTESIAN_POINT ( 'NONE',  ( -85.40857260003362228, -272.5650094348158063, -215.1376661235696588 ) ) ;
#15322 = CARTESIAN_POINT ( 'NONE',  ( 15.43191736720857499, -293.8374305555566934, -326.3474752454189343 ) ) ;
#15323 = CARTESIAN_POINT ( 'NONE',  ( 85.24291059917956659, 81.26895831550152138, -298.9807373495123102 ) ) ;
#15324 = ADVANCED_FACE ( 'NONE', ( #71405, #21193, #5605 ), #36331, .F. ) ;
#15326 = CARTESIAN_POINT ( 'NONE',  ( -95.59447479657197277, -288.3203665069697195, -315.6921891144242522 ) ) ;
#15325 = CARTESIAN_POINT ( 'NONE',  ( -52.43185771060288403, -272.5477438386967606, -195.3031254171106923 ) ) ;
#15327 = CARTESIAN_POINT ( 'NONE',  ( -98.18235092230905536, -297.8293001002335814, -312.8967582406389170 ) ) ;
#15328 = EDGE_CURVE ( 'NONE', #65802, #1567, #77399, .T. ) ;
#15329 = CARTESIAN_POINT ( 'NONE',  ( 20.75756271806354292, -289.4971424093940300, -315.3894901371530750 ) ) ;
#15330 = ORIENTED_EDGE ( 'NONE', *, *, #72825, .T. ) ;
#15331 = CARTESIAN_POINT ( 'NONE',  ( -5.883131775773463801, -295.5898353717196301, -340.3838192367417719 ) ) ;
#15332 = CARTESIAN_POINT ( 'NONE',  ( 6.959264756027824461, -287.1659062529643620, -212.1988963803346167 ) ) ;
#15333 = CARTESIAN_POINT ( 'NONE',  ( -29.85532486723949219, -273.0651550450975265, -194.0365040302886257 ) ) ;
#15334 = CARTESIAN_POINT ( 'NONE',  ( 33.17215089936051697, -293.9651387880358584, -239.8331695859829722 ) ) ;
#15335 = CARTESIAN_POINT ( 'NONE',  ( 37.36068917164182324, -293.8139545025637744, -251.9469946960184927 ) ) ;
#15336 = CARTESIAN_POINT ( 'NONE',  ( -55.01440978826175865, -291.9851717417379859, -199.5326255677821905 ) ) ;
#15337 = ORIENTED_EDGE ( 'NONE', *, *, #79978, .T. ) ;
#15338 = CARTESIAN_POINT ( 'NONE',  ( -52.28521652858497504, -275.7825512789535765, -196.2401175497192582 ) ) ;
#15339 = CARTESIAN_POINT ( 'NONE',  ( 39.22579307701682438, -274.3933294783302586, -274.0402769847039508 ) ) ;
#15340 = ORIENTED_EDGE ( 'NONE', *, *, #68145, .T. ) ;
#15341 = CARTESIAN_POINT ( 'NONE',  ( -86.76039210456256967, -278.8940769487023772, -211.3228784931404221 ) ) ;
#15342 = CARTESIAN_POINT ( 'NONE',  ( -11.18784957111032163, -272.7984835083657345, -201.2962092691876421 ) ) ;
#15343 = CARTESIAN_POINT ( 'NONE',  ( -110.1944817108390282, -273.7391095985399261, -262.1942159385521336 ) ) ;
#15344 = CARTESIAN_POINT ( 'NONE',  ( -46.21914874989020916, -274.8780235908361078, -197.6658681115683578 ) ) ;
#15345 = CARTESIAN_POINT ( 'NONE',  ( -34.81320809752045875, -299.6834293582773512, -194.1604374374741724 ) ) ;
#15346 =( GEOMETRIC_REPRESENTATION_CONTEXT ( 3 ) GLOBAL_UNCERTAINTY_ASSIGNED_CONTEXT ( ( #864 ) ) GLOBAL_UNIT_ASSIGNED_CONTEXT ( ( #46095, #75000, #22926 ) ) REPRESENTATION_CONTEXT ( 'NONE', 'WORKASPACE' ) );
#15347 = CARTESIAN_POINT ( 'NONE',  ( -7.255076896303360279, -274.6796336568085053, -339.4634301279916144 ) ) ;
#15348 = CARTESIAN_POINT ( 'NONE',  ( -50.48139850148218244, -295.8758124243128691, -342.2724591918818078 ) ) ;
#15349 = CARTESIAN_POINT ( 'NONE',  ( 4.133635785970411369, -293.0556478034519614, -331.1490397004779425 ) ) ;
#15350 = CARTESIAN_POINT ( 'NONE',  ( 29.33919985515026596, -277.8906705383787994, 25.50000000000000000 ) ) ;
#15351 = CARTESIAN_POINT ( 'NONE',  ( -71.53786057731051073, -277.9841363965887240, -339.2824464234855100 ) ) ;
#15352 = CARTESIAN_POINT ( 'NONE',  ( -38.08449000872437296, -274.2092686259905463, -197.3648970685308370 ) ) ;
#15353 = CARTESIAN_POINT ( 'NONE',  ( -113.1133792082728462, -283.0990852358850134, -281.3165783458058513 ) ) ;
#15354 = CARTESIAN_POINT ( 'NONE',  ( -110.1855073782314776, -298.3140285322057821, -288.9550740863743954 ) ) ;
#15355 = DIRECTION ( 'NONE',  ( 0.000000000000000000, 0.000000000000000000, 1.000000000000000000 ) ) ;
#15356 = CARTESIAN_POINT ( 'NONE',  ( -73.62685291481743377, -284.7545394330281852, -206.8171534796748858 ) ) ;
#15357 = CARTESIAN_POINT ( 'NONE',  ( -110.9138627468296221, -276.6811061017833708, -278.8845582845285662 ) ) ;
#15358 = CARTESIAN_POINT ( 'NONE',  ( -62.00426131226882376, -275.9537518484900147, -339.7487888401189480 ) ) ;
#15359 = CARTESIAN_POINT ( 'NONE',  ( -44.77375041825170854, -285.1462579040637593, -345.0429320035668752 ) ) ;
#15360 = CARTESIAN_POINT ( 'NONE',  ( -3.937601171315169957, -275.7079977478201727, -204.9918520094395262 ) ) ;
#15361 = CARTESIAN_POINT ( 'NONE',  ( 37.16749025082013702, -273.7495129339185382, -254.3362449738000350 ) ) ;
#15362 = CARTESIAN_POINT ( 'NONE',  ( -28.46734655870469055, -282.1645066135703246, -195.6678022783608242 ) ) ;
#15363 = CARTESIAN_POINT ( 'NONE',  ( 139.6925840978351516, -27.00396092263537184, 22.50000000000000000 ) ) ;
#15364 = CARTESIAN_POINT ( 'NONE',  ( 27.45092162264288760, -288.9544822160695503, -231.3857146236530866 ) ) ;
#15365 = CYLINDRICAL_SURFACE ( 'NONE', #84868, 4.000000000000003553 ) ;
#15366 = CARTESIAN_POINT ( 'NONE',  ( 19.00382594025919403, -290.8640596368140905, -220.8427051785129720 ) ) ;
#15367 = DIRECTION ( 'NONE',  ( 0.000000000000000000, 0.000000000000000000, 1.000000000000000000 ) ) ;
#15368 = CARTESIAN_POINT ( 'NONE',  ( -75.40350267319112731, -296.3276379751258105, -207.5452894004086204 ) ) ;
#15369 = CARTESIAN_POINT ( 'NONE',  ( -110.3986613925245450, -288.5208427580174657, -283.5347998072239193 ) ) ;
#15370 = CARTESIAN_POINT ( 'NONE',  ( 139.3989977797154154, 177.7276089766264704, -238.0725708408485843 ) ) ;
#15371 = DIRECTION ( 'NONE',  ( -1.000000000000000000, 0.000000000000000000, 0.000000000000000000 ) ) ;
#15372 = CARTESIAN_POINT ( 'NONE',  ( -65.21199394003551220, -287.8895862575334945, -341.4518425499307455 ) ) ;
#15373 = CARTESIAN_POINT ( 'NONE',  ( -3.233727128736103129, -284.1940206674063916, -335.8205728660128102 ) ) ;
#15374 = CARTESIAN_POINT ( 'NONE',  ( -109.9509919666699034, -283.0791428576383737, -247.7818524211022577 ) ) ;
#15375 = CARTESIAN_POINT ( 'NONE',  ( 8.172521695665620811, -283.8412485106957206, -328.2520732891190960 ) ) ;
#15376 = CARTESIAN_POINT ( 'NONE',  ( -61.57859437390880686, -284.1779536486143343, -339.4447134093149998 ) ) ;
#15377 = CARTESIAN_POINT ( 'NONE',  ( -95.99362198791807543, -291.8837106165035493, -317.6927569271431935 ) ) ;
#15378 = CARTESIAN_POINT ( 'NONE',  ( -83.57078393854244780, -273.7710369225730460, -208.7426653384931967 ) ) ;
#15379 = CARTESIAN_POINT ( 'NONE',  ( -7.511357110192556696, -286.7439872543364459, -339.7974549331641470 ) ) ;
#15380 = CARTESIAN_POINT ( 'NONE',  ( 33.71354887436204706, -275.1733096831787293, -240.5560580419500809 ) ) ;
#15381 = CARTESIAN_POINT ( 'NONE',  ( 34.71085874907662117, -295.7845293362111079, -289.9104346689396721 ) ) ;
#15382 = CARTESIAN_POINT ( 'NONE',  ( -48.18343439339134449, -276.7382201398751249, -436.3198488720590262 ) ) ;
#15383 = CARTESIAN_POINT ( 'NONE',  ( -106.6379572354042296, -292.6233781216987495, -303.7686719486574702 ) ) ;
#15384 = CARTESIAN_POINT ( 'NONE',  ( -21.29675257103413344, -281.5269861995448650, -342.1337916457709412 ) ) ;
#15385 = CARTESIAN_POINT ( 'NONE',  ( -110.7008741339251259, -276.3420841252038826, -286.7458676169089813 ) ) ;
#15386 = CARTESIAN_POINT ( 'NONE',  ( -52.38977702765697586, -272.3428288674879809, -195.4989944281992109 ) ) ;
#15387 = CARTESIAN_POINT ( 'NONE',  ( 24.06551077319547005, -275.4501638977528728, -310.1160959191046800 ) ) ;
#15388 = CARTESIAN_POINT ( 'NONE',  ( -55.19892289577111200, -293.3383958537947933, -198.8640736691187669 ) ) ;
#15389 = CARTESIAN_POINT ( 'NONE',  ( 22.77424686552371824, -293.9120259033625757, -228.5122250550866738 ) ) ;
#15390 = CARTESIAN_POINT ( 'NONE',  ( -109.0154977850382920, -286.5526682517989343, -251.8992452407488543 ) ) ;
#15391 = CARTESIAN_POINT ( 'NONE',  ( 35.71823501086125674, -294.6942363690599223, -247.9813912079839326 ) ) ;
#15392 = CARTESIAN_POINT ( 'NONE',  ( 36.62411581856360243, -295.1136947045292800, -289.9150522489528043 ) ) ;
#15393 = CARTESIAN_POINT ( 'NONE',  ( -96.40966383013012830, -295.7849124579788054, -313.2773922716567085 ) ) ;
#15394 = CARTESIAN_POINT ( 'NONE',  ( -61.88612845664857787, -291.3713609523749142, -341.2312222974078963 ) ) ;
#15395 = CARTESIAN_POINT ( 'NONE',  ( -111.4908979686912858, -284.4587181892767944, -291.1191637506960888 ) ) ;
#15396 = CARTESIAN_POINT ( 'NONE',  ( -108.9269296779008727, -271.0097198716212006, -245.5445833778888129 ) ) ;
#15397 = CARTESIAN_POINT ( 'NONE',  ( -105.7851207363626003, -283.9294843761073253, -305.7549059128548379 ) ) ;
#15398 = CARTESIAN_POINT ( 'NONE',  ( -111.5360518773532306, -280.4205367059468585, -279.0047666204628740 ) ) ;
#15399 = CARTESIAN_POINT ( 'NONE',  ( -104.9574016360991919, -283.7297886563487168, -241.6780112830523137 ) ) ;
#15400 = CARTESIAN_POINT ( 'NONE',  ( 32.98785508828261470, -285.2138356126249050, -244.3082043236840946 ) ) ;
#15401 = CARTESIAN_POINT ( 'NONE',  ( -69.41752987730927771, -277.7742047141237549, -201.7069827068197014 ) ) ;
#15403 = AXIS2_PLACEMENT_3D ( 'NONE', #23490, #80310, #90086 ) ;
#15402 = CARTESIAN_POINT ( 'NONE',  ( -35.93751134800100289, -122.5594593288581251, -363.2174194532766478 ) ) ;
#15404 = CARTESIAN_POINT ( 'NONE',  ( -110.4520475260046481, -284.0526527651196034, -270.9035042900704866 ) ) ;
#15405 = AXIS2_PLACEMENT_3D ( 'NONE', #72555, #1502, #37476 ) ;
#15406 = CARTESIAN_POINT ( 'NONE',  ( 23.09913496815175193, -283.3894092190927836, -317.4451948365138492 ) ) ;
#15407 = CARTESIAN_POINT ( 'NONE',  ( -36.10269794830810497, -288.0957602359025600, -347.1288956867550155 ) ) ;
#15408 = CARTESIAN_POINT ( 'NONE',  ( -95.52501399680663496, -279.4821460033404037, -319.5863559707076433 ) ) ;
#15409 = CARTESIAN_POINT ( 'NONE',  ( -75.07828521310315750, -278.8592459885100538, -336.9137168734408760 ) ) ;
#15410 = CARTESIAN_POINT ( 'NONE',  ( -19.53250049226435792, -280.1208348475300340, -199.5145310700542041 ) ) ;
#15411 = CARTESIAN_POINT ( 'NONE',  ( -77.46921265032453618, -275.4907273521913567, -207.4196408772093037 ) ) ;
#15412 = CARTESIAN_POINT ( 'NONE',  ( 28.10592367883777953, -294.0838060122432580, -311.0273911351308129 ) ) ;
#15413 = CARTESIAN_POINT ( 'NONE',  ( -34.54098843903138061, -287.0370281848212244, -345.0040618070150344 ) ) ;
#15414 = AXIS2_PLACEMENT_3D ( 'NONE', #44355, #8377, #45267 ) ;
#15415 = CARTESIAN_POINT ( 'NONE',  ( -74.30881767538970450, -293.1691916583761781, -203.7287486985987925 ) ) ;
#15416 = CARTESIAN_POINT ( 'NONE',  ( -68.66183837227877973, -294.3940262995200783, -336.6566932860676502 ) ) ;
#15417 = CARTESIAN_POINT ( 'NONE',  ( -3.137608213132380364, -294.2538179820011237, -334.8759812553842607 ) ) ;
#15418 = CARTESIAN_POINT ( 'NONE',  ( -112.0194285377326366, -291.8510213313587656, -252.9046180210496857 ) ) ;
#15419 = CARTESIAN_POINT ( 'NONE',  ( 34.66606907960790807, -282.0375775403526291, -257.7605687045281115 ) ) ;
#15420 = CARTESIAN_POINT ( 'NONE',  ( 53.14800697766726501, -298.0804408912529766, -193.6863325086212342 ) ) ;
#15421 = CARTESIAN_POINT ( 'NONE',  ( -54.47082684962213506, -289.9179250305709274, -345.3817871544957825 ) ) ;
#15422 = CARTESIAN_POINT ( 'NONE',  ( -8.530893964465663615, -280.8187867445068946, -340.4898669552225670 ) ) ;
#15423 = EDGE_CURVE ( 'NONE', #71244, #74736, #57744, .T. ) ;
#15424 = CARTESIAN_POINT ( 'NONE',  ( 28.88771343880231512, -288.3967428443834820, -309.5964218560844188 ) ) ;
#15425 = CARTESIAN_POINT ( 'NONE',  ( -89.68097257443268688, -285.6221978585015222, -219.3701080027280454 ) ) ;
#15426 = DIRECTION ( 'NONE',  ( 0.6056179655966483777, -0.7957555401921979632, -1.840554422280015381E-15 ) ) ;
#15427 = CARTESIAN_POINT ( 'NONE',  ( 119.8541137665874032, 149.3386895696777685, -261.6380840896607083 ) ) ;
#15428 = CARTESIAN_POINT ( 'NONE',  ( 184.3255359987551572, 260.6165026356828207, -150.9744038209046835 ) ) ;
#15429 = CARTESIAN_POINT ( 'NONE',  ( -64.86740973677453326, -278.8803471481014640, -202.5751530804830054 ) ) ;
#15430 = CARTESIAN_POINT ( 'NONE',  ( -108.4753526115228794, -277.2389246256303181, -288.1394287253564812 ) ) ;
#15431 = CARTESIAN_POINT ( 'NONE',  ( 26.91524881597910834, -274.6613155780240163, -227.9725723138843421 ) ) ;
#15432 = CARTESIAN_POINT ( 'NONE',  ( 169.0186518065400207, 229.7053051813165609, -190.5595449943317590 ) ) ;
#15433 = ADVANCED_FACE ( 'NONE', ( #50064 ), #34479, .F. ) ;
#15434 = CARTESIAN_POINT ( 'NONE',  ( -113.6215691676236190, -277.1832258824243240, -265.8903383180676201 ) ) ;
#15435 = CARTESIAN_POINT ( 'NONE',  ( -4.117207549396958655, -280.6319489220272771, -337.2040674947708112 ) ) ;
#15436 = CARTESIAN_POINT ( 'NONE',  ( 3.699105587511749338, -296.2685889135162824, -334.3732642774897954 ) ) ;
#15437 = CARTESIAN_POINT ( 'NONE',  ( -12.24495194684063826, -292.8798780284144527, -201.6912972614359774 ) ) ;
#15438 = CARTESIAN_POINT ( 'NONE',  ( -113.3132253104770513, -273.6360301137744386, -258.9914686285616199 ) ) ;
#15439 = CARTESIAN_POINT ( 'NONE',  ( -15.72246093755871854, -287.4514675733697686, -340.6556792537484739 ) ) ;
#15440 = CARTESIAN_POINT ( 'NONE',  ( -112.3457027523918725, -273.4159770912813769, -253.3990315088814782 ) ) ;
#15441 = CARTESIAN_POINT ( 'NONE',  ( -99.89788960871300105, -297.2377200359368885, -232.6367136827935838 ) ) ;
#15442 = ORIENTED_EDGE ( 'NONE', *, *, #82641, .T. ) ;
#15443 = CARTESIAN_POINT ( 'NONE',  ( 208.4306832106271088, -74.55766379199613425, 0.000000000000000000 ) ) ;
#15444 = CARTESIAN_POINT ( 'NONE',  ( -111.5859246497350910, -280.6521163567664416, -256.2522418109721229 ) ) ;
#15445 = CARTESIAN_POINT ( 'NONE',  ( -49.20541722335731549, -280.9770700740090206, -198.0183347243558103 ) ) ;
#15446 = CARTESIAN_POINT ( 'NONE',  ( -84.22333551785669670, -279.4466209132146446, -330.2283487039617285 ) ) ;
#15447 = CARTESIAN_POINT ( 'NONE',  ( 9.944657221575299744, -273.1969317345193531, -213.7725295160784356 ) ) ;
#15448 = CARTESIAN_POINT ( 'NONE',  ( 160.5350683151633291, 250.0000000000000568, 20.22542485937379908 ) ) ;
#15449 = CYLINDRICAL_SURFACE ( 'NONE', #59273, 4.025000000000000355 ) ;
#15450 = CARTESIAN_POINT ( 'NONE',  ( -1.533896377987240323, -277.3924975820768850, -338.3461164124301490 ) ) ;
#15451 = CARTESIAN_POINT ( 'NONE',  ( -7.350445041457863482, -278.6590430200135984, -339.1174624732529992 ) ) ;
#15452 = CARTESIAN_POINT ( 'NONE',  ( -82.21502377928607075, -276.2259147438053333, -332.2076305431442051 ) ) ;
#15453 = ORIENTED_EDGE ( 'NONE', *, *, #69844, .F. ) ;
#15454 = CARTESIAN_POINT ( 'NONE',  ( 199.9517221346984002, 40.04024871352131498, 9.062294003318640989 ) ) ;
#15455 = CARTESIAN_POINT ( 'NONE',  ( 23.78809117464455980, -284.1292499200839075, -314.4461156251521743 ) ) ;
#15456 = CARTESIAN_POINT ( 'NONE',  ( -14.78692970620623548, -291.5491870720394445, -200.7631003535099410 ) ) ;
#15457 = CARTESIAN_POINT ( 'NONE',  ( -32.30480070587665864, -285.4626604036957929, -193.6150399180537818 ) ) ;
#15458 = CARTESIAN_POINT ( 'NONE',  ( -109.9782385243363905, -282.6071293582365342, -284.5705270272298435 ) ) ;
#15459 = CARTESIAN_POINT ( 'NONE',  ( -40.27587738680338703, -281.6644807898208001, -343.8918294037683268 ) ) ;
#15460 = CARTESIAN_POINT ( 'NONE',  ( -59.87002246616999201, -280.9588795646532162, -200.4533483243079104 ) ) ;
#15461 = CARTESIAN_POINT ( 'NONE',  ( -99.53540881432127208, -271.1200460983058633, -228.3527980389987988 ) ) ;
#15462 = AXIS2_PLACEMENT_3D ( 'NONE', #12551, #55177, #69370 ) ;
#15463 = CARTESIAN_POINT ( 'NONE',  ( -91.87558171365287762, -282.2143529597015004, -323.5823184013495961 ) ) ;
#15464 = CARTESIAN_POINT ( 'NONE',  ( -102.8434524688352667, -298.0648251110738443, -306.9983206699136531 ) ) ;
#15465 = AXIS2_PLACEMENT_3D ( 'NONE', #2295, #37780, #30701 ) ;
#15466 = CARTESIAN_POINT ( 'NONE',  ( -104.4823228387848957, -279.0998642985279616, -299.7378469757191510 ) ) ;
#15467 = CARTESIAN_POINT ( 'NONE',  ( -112.0016947189301248, -286.6639379115852648, -261.6482749732219304 ) ) ;
#15468 = VECTOR ( 'NONE', #3128, 1000.000000000000000 ) ;
#15469 = CARTESIAN_POINT ( 'NONE',  ( 215.9306832106270804, -142.7221692137691775, 9.184850993605173582E-16 ) ) ;
#15470 = CARTESIAN_POINT ( 'NONE',  ( -37.81109012966459915, -293.9664642839941848, -194.8025719700286231 ) ) ;
#15471 = TOROIDAL_SURFACE ( 'NONE', #86492, 5.603083949679977138, 0.5000000000000000000 ) ;
#15472 = CARTESIAN_POINT ( 'NONE',  ( -0.5096664150300678209, -274.5628873235659171, -335.7528852756741458 ) ) ;
#15473 = CARTESIAN_POINT ( 'NONE',  ( 21.35903660258810532, -287.4187249604672729, -319.9431946665179680 ) ) ;
#15474 = CARTESIAN_POINT ( 'NONE',  ( -2.039019217071922796, -290.9276490029278079, -205.5381152348151375 ) ) ;
#15475 = CARTESIAN_POINT ( 'NONE',  ( -70.69144971784091069, -276.1864441551169307, -335.8518629902656016 ) ) ;
#15476 = CARTESIAN_POINT ( 'NONE',  ( -110.9580217513515663, -294.8208446344581830, -260.4080340269800899 ) ) ;
#15477 = CARTESIAN_POINT ( 'NONE',  ( -12.10649988399451615, -293.7025721853072469, -201.2820442769315719 ) ) ;
#15478 = CARTESIAN_POINT ( 'NONE',  ( 154.5625123364531817, 249.5000000000000568, -13.15740740740742076 ) ) ;
#15479 = DIRECTION ( 'NONE',  ( 1.000000000000000000, 0.000000000000000000, 0.000000000000000000 ) ) ;
#15480 = CARTESIAN_POINT ( 'NONE',  ( -64.04188194062869854, -293.8740878990336114, -341.8440393241148740 ) ) ;
#15481 = CARTESIAN_POINT ( 'NONE',  ( 19.26238690199036796, -288.4871869828853619, -222.9872636629539500 ) ) ;
#15482 = CARTESIAN_POINT ( 'NONE',  ( -112.1398541117927579, -288.6214275298790994, -283.8216726500512550 ) ) ;
#15483 = CARTESIAN_POINT ( 'NONE',  ( -18.30370430935523629, -290.2274056412199457, -341.4980935733968295 ) ) ;
#15484 = LINE ( 'NONE', #30623, #92521 ) ;
#15485 = CARTESIAN_POINT ( 'NONE',  ( -96.68361562349598159, -290.7578489211797432, -313.1529255233432423 ) ) ;
#15486 = FACE_OUTER_BOUND ( 'NONE', #22877, .T. ) ;
#15487 = CARTESIAN_POINT ( 'NONE',  ( -84.90605288674601070, -290.8963931897126827, -330.4757758274485582 ) ) ;
#15488 = CARTESIAN_POINT ( 'NONE',  ( -22.85709954863275328, -278.2565650340623051, -196.3580142372265414 ) ) ;
#15489 = CARTESIAN_POINT ( 'NONE',  ( -75.00129581361970565, -279.8979010202619406, -203.2232066034774789 ) ) ;
#15490 = CARTESIAN_POINT ( 'NONE',  ( -3.663025696490039618, -280.1511800364907572, -201.1260053622769419 ) ) ;
#15491 = CARTESIAN_POINT ( 'NONE',  ( 20.21249047490515949, -284.8874804659265010, -222.2524768509212549 ) ) ;
#15492 = CARTESIAN_POINT ( 'NONE',  ( 210.7238915819278589, 32.98517505407394168, 12.09245862095555601 ) ) ;
#15493 = CARTESIAN_POINT ( 'NONE',  ( -97.39115258327184677, -277.2924297602724550, -226.7156286179795188 ) ) ;
#15494 = CARTESIAN_POINT ( 'NONE',  ( -14.06740595226352220, -280.7500629050644534, -341.6584382519707788 ) ) ;
#15495 = CARTESIAN_POINT ( 'NONE',  ( -69.44095347752850955, -196.3684352495399423, -356.8806866962679010 ) ) ;
#15496 = CARTESIAN_POINT ( 'NONE',  ( -86.34452415002552073, -277.8664675687668364, -211.7992629637615778 ) ) ;
#15497 = CARTESIAN_POINT ( 'NONE',  ( -113.2952137877150705, -283.3345498565198000, -281.3459419085112359 ) ) ;
#15498 = CARTESIAN_POINT ( 'NONE',  ( -91.24841961072959862, -274.0634702276702228, -220.8787716704212016 ) ) ;
#15499 = CARTESIAN_POINT ( 'NONE',  ( -94.65661773434429449, -274.6668990126169660, -219.8278961034325221 ) ) ;
#15500 = CARTESIAN_POINT ( 'NONE',  ( 30.29600990820854989, -275.5889779607466608, -298.0134113041055457 ) ) ;
#15501 = CARTESIAN_POINT ( 'NONE',  ( -95.47709060472682552, -297.8992183653352299, -317.7656488081095745 ) ) ;
#15502 = CARTESIAN_POINT ( 'NONE',  ( -5.624555881219731823, -288.8130865274976600, -340.5253735928897072 ) ) ;
#15503 = CARTESIAN_POINT ( 'NONE',  ( 3.072819304755261438, -278.6697504338949329, -206.4558938566724748 ) ) ;
#15504 = CARTESIAN_POINT ( 'NONE',  ( -74.67703883990867553, -291.4026685653622053, -203.0181711522665751 ) ) ;
#15505 = CARTESIAN_POINT ( 'NONE',  ( -73.67207087498614726, -288.6058024108472182, -333.9641971604327750 ) ) ;
#15506 = CARTESIAN_POINT ( 'NONE',  ( 37.65702769368315472, -291.5157384812855526, -267.5379728276618039 ) ) ;
#15507 = EDGE_LOOP ( 'NONE', ( #32884, #10721, #24627, #68792 ) ) ;
#15508 = CARTESIAN_POINT ( 'NONE',  ( 199.8761955117210221, 66.90278937422385752, 8.069515584579029621 ) ) ;
#15509 = CARTESIAN_POINT ( 'NONE',  ( -86.77562673980663988, -289.2693975491652623, -324.2282259305274010 ) ) ;
#15510 = DIRECTION ( 'NONE',  ( -0.000000000000000000, -0.000000000000000000, -1.000000000000000000 ) ) ;
#15511 = CARTESIAN_POINT ( 'NONE',  ( 11.91738437348854696, -287.6583459198519108, -211.4159385299737437 ) ) ;
#15512 = CARTESIAN_POINT ( 'NONE',  ( 34.45848030099739390, -296.0519495502701943, -270.3284710469131937 ) ) ;
#15513 = CARTESIAN_POINT ( 'NONE',  ( 15.30857153722725528, -293.3885980682417767, -326.2249623367883373 ) ) ;
#15514 = CARTESIAN_POINT ( 'NONE',  ( -24.59912086932454756, -284.2081126969912930, -345.8531086079086094 ) ) ;
#15515 = CARTESIAN_POINT ( 'NONE',  ( -107.7617144909671794, -284.1307738691438658, -289.6442625614449753 ) ) ;
#15516 = CARTESIAN_POINT ( 'NONE',  ( 35.84662990274996019, -276.9549491958516114, -277.0478080881935625 ) ) ;
#15517 = CARTESIAN_POINT ( 'NONE',  ( 36.46040943060042139, -291.7208780362105927, -281.8811912947693372 ) ) ;
#15518 = CARTESIAN_POINT ( 'NONE',  ( -56.95302693766149105, -272.5885782481558408, -199.5795779481681222 ) ) ;
#15519 = ORIENTED_EDGE ( 'NONE', *, *, #30767, .F. ) ;
#15520 = CARTESIAN_POINT ( 'NONE',  ( 220.4471435719830197, 34.91984470236808136, -9.000000000000001776 ) ) ;
#15521 = CARTESIAN_POINT ( 'NONE',  ( 38.04902157672568563, -293.4134731304052934, -285.9169327299435395 ) ) ;
#15522 = CARTESIAN_POINT ( 'NONE',  ( -42.80371783198999225, -287.9028809908334665, -196.1088968441945610 ) ) ;
#15523 = CARTESIAN_POINT ( 'NONE',  ( -111.3275404330224063, -297.8879251974468048, -249.9759473579094902 ) ) ;
#15524 = CARTESIAN_POINT ( 'NONE',  ( 20.41609760707875409, -287.5732843027383296, -225.5511919691297180 ) ) ;
#15525 = EDGE_CURVE ( 'NONE', #75506, #6373, #36562, .T. ) ;
#15526 = CARTESIAN_POINT ( 'NONE',  ( -113.0690263310504378, -277.4531231761198455, -282.9385692079628143 ) ) ;
#15527 = CARTESIAN_POINT ( 'NONE',  ( -34.84962683864793576, -295.6730240235590941, -347.2187939663132283 ) ) ;
#15528 = CARTESIAN_POINT ( 'NONE',  ( 17.73043949616242898, -286.4139552355005094, -322.3934628999368783 ) ) ;
#15529 = CARTESIAN_POINT ( 'NONE',  ( 13.38508417406806750, -294.6986037307403876, -328.3328991369119194 ) ) ;
#15531 = CARTESIAN_POINT ( 'NONE',  ( -98.31953436761223486, -291.4435006487648820, -230.0972434778849447 ) ) ;
#15530 = AXIS2_PLACEMENT_3D ( 'NONE', #4865, #91002, #77306 ) ;
#15532 = CARTESIAN_POINT ( 'NONE',  ( 76.08708295871279859, -296.0521521680024080, -472.6442049081569508 ) ) ;
#15533 = AXIS2_PLACEMENT_3D ( 'NONE', #15559, #73336, #8903 ) ;
#15534 = FACE_OUTER_BOUND ( 'NONE', #6848, .T. ) ;
#15535 = CARTESIAN_POINT ( 'NONE',  ( 167.9831408986860311, 229.6749329237118502, -189.9962676830372459 ) ) ;
#15536 = CARTESIAN_POINT ( 'NONE',  ( -26.73678813539466859, -287.7046817743762404, -194.7419480771833946 ) ) ;
#15537 = CARTESIAN_POINT ( 'NONE',  ( -115.3288506153726871, -288.2666405000203440, -252.5284128619063608 ) ) ;
#15538 = ORIENTED_EDGE ( 'NONE', *, *, #46974, .T. ) ;
#15539 = MECHANICAL_DESIGN_GEOMETRIC_PRESENTATION_REPRESENTATION (  '', ( #48848 ), #88107 ) ;
#15540 = CARTESIAN_POINT ( 'NONE',  ( -40.99524215679190320, -279.3559304719699412, -193.5367140391501266 ) ) ;
#15541 = CARTESIAN_POINT ( 'NONE',  ( 22.49070238628492291, -284.1681633019224478, -315.3279585992952434 ) ) ;
#15542 = CARTESIAN_POINT ( 'NONE',  ( 199.0215121565617267, 282.8125914077994594, -111.1903278149338234 ) ) ;
#15543 = CARTESIAN_POINT ( 'NONE',  ( -111.1472884868231148, -283.3787551812042693, -250.3800831854763942 ) ) ;
#15545 = CARTESIAN_POINT ( 'NONE',  ( 33.68026516675332971, -285.9238120139998500, -292.8303560276534085 ) ) ;
#15544 = VECTOR ( 'NONE', #14990, 1000.000000000000000 ) ;
#15546 = CARTESIAN_POINT ( 'NONE',  ( -63.15882302151877781, -275.5798269534439555, -199.1306354260173350 ) ) ;
#15547 = PRODUCT ( 'Reciprocating Rivet Punch Pin', 'Reciprocating Rivet Punch Pin', '', ( #47307 ) ) ;
#15548 = CARTESIAN_POINT ( 'NONE',  ( -96.15358268493778837, -297.6517714330614695, -226.9908198767547276 ) ) ;
#15549 = CARTESIAN_POINT ( 'NONE',  ( -71.17261840074534973, -294.1932781082168731, -335.6186839874679890 ) ) ;
#15550 = CARTESIAN_POINT ( 'NONE',  ( -72.78631088524953441, -278.1605068824746922, -338.6179612575067495 ) ) ;
#15551 = CARTESIAN_POINT ( 'NONE',  ( 3.134106313982170988, -276.4915120258694401, -331.1123244962138870 ) ) ;
#15552 = CARTESIAN_POINT ( 'NONE',  ( 29.67071477812140401, -276.1451962938810993, -232.9581353193223947 ) ) ;
#15553 = CARTESIAN_POINT ( 'NONE',  ( -106.0744761891404693, -277.0321602773960876, -304.4997240623635548 ) ) ;
#15554 = CARTESIAN_POINT ( 'NONE',  ( -108.0627147292225203, -262.2579186427535092, -317.5738021120087069 ) ) ;
#15555 = CARTESIAN_POINT ( 'NONE',  ( 37.67789369394757415, -273.5799789553166192, -272.5411780619711521 ) ) ;
#15556 = EDGE_CURVE ( 'NONE', #48224, #74021, #36715, .T. ) ;
#15557 = CARTESIAN_POINT ( 'NONE',  ( -100.2757451797973403, -298.5541765641321490, -227.0032316287117169 ) ) ;
#15558 = CARTESIAN_POINT ( 'NONE',  ( 175.2296996224749250, 215.0000000000000568, -24.99999999999999289 ) ) ;
#15559 = CARTESIAN_POINT ( 'NONE',  ( 223.4306832106270804, -135.2391364535880882, -21.50000000000000000 ) ) ;
#15560 = CARTESIAN_POINT ( 'NONE',  ( -8.144417319489569707, -287.5234762706672313, -203.1171981764386203 ) ) ;
#15561 = CARTESIAN_POINT ( 'NONE',  ( -94.55676660713815807, -285.6269370007227053, -320.3652196448921927 ) ) ;
#15562 = CARTESIAN_POINT ( 'NONE',  ( 11.20794237688972927, -286.0941820544749703, -215.6412479039078107 ) ) ;
#15563 = CARTESIAN_POINT ( 'NONE',  ( -102.5734509685682383, -276.4869920278521818, -304.8757394560932426 ) ) ;
#15564 = CARTESIAN_POINT ( 'NONE',  ( -71.96432037833695006, -285.3754567050283413, -336.0280019457031244 ) ) ;
#15565 = CARTESIAN_POINT ( 'NONE',  ( -30.17587885582971552, -278.6241839869974797, -196.9661724759061485 ) ) ;
#15566 = CARTESIAN_POINT ( 'NONE',  ( 28.31344128722500741, -277.0735379453712994, -303.0889167322516755 ) ) ;
#15567 = CARTESIAN_POINT ( 'NONE',  ( 198.8656410362497695, 68.63459961102830675, -9.310658723936024117 ) ) ;
#15568 = CARTESIAN_POINT ( 'NONE',  ( -67.08829714036308189, -274.1437299935051897, -203.6156482484107926 ) ) ;
#15569 = CARTESIAN_POINT ( 'NONE',  ( -19.80303690281566986, -281.0747829459431841, -195.4963438305881596 ) ) ;
#15570 = VECTOR ( 'NONE', #139, 1000.000000000000000 ) ;
#15571 = CARTESIAN_POINT ( 'NONE',  ( -10.71744063881215503, -283.2065319318710976, -342.6027311592188767 ) ) ;
#15572 = ORIENTED_EDGE ( 'NONE', *, *, #30621, .T. ) ;
#15573 = VERTEX_POINT ( 'NONE', #49147 ) ;
#15574 = CARTESIAN_POINT ( 'NONE',  ( 195.7540919006722504, 41.65591105122726390, 14.27491332538345148 ) ) ;
#15575 = CARTESIAN_POINT ( 'NONE',  ( 29.03776111825984074, -288.9305519403758922, -233.7273628332340252 ) ) ;
#15576 = CARTESIAN_POINT ( 'NONE',  ( -109.0059822543751409, -289.5796578308784888, -243.4235014689797936 ) ) ;
#15577 = CARTESIAN_POINT ( 'NONE',  ( -104.0881193809927652, -295.3451835055575430, -300.4435881306248461 ) ) ;
#15578 = CARTESIAN_POINT ( 'NONE',  ( -27.85343086611573327, -291.5180707966947580, -193.9970591528559396 ) ) ;
#15579 = CARTESIAN_POINT ( 'NONE',  ( 6.239210459243984985, -286.9286035570306694, -329.8503855643155589 ) ) ;
#15580 = CARTESIAN_POINT ( 'NONE',  ( 0.3595220217773859583, -287.7711873389431503, -207.3276844743342906 ) ) ;
#15581 = CARTESIAN_POINT ( 'NONE',  ( -69.91165696735023971, -294.1233781216987495, -202.8022627189028810 ) ) ;
#15582 = CARTESIAN_POINT ( 'NONE',  ( 36.70468566338232819, -289.7094520672786757, -282.5994867599419536 ) ) ;
#15583 = CARTESIAN_POINT ( 'NONE',  ( -102.2289997878032040, -288.0449517667890404, -308.4070688725983587 ) ) ;
#15584 = CARTESIAN_POINT ( 'NONE',  ( -71.50806339830540992, -284.4564413394722919, -335.1381823614480027 ) ) ;
#15585 = CARTESIAN_POINT ( 'NONE',  ( -110.7688462590590603, -292.3463345877702864, -286.4385133592856505 ) ) ;
#15586 = CARTESIAN_POINT ( 'NONE',  ( 82.15764098272329363, -298.8646310024031436, -193.4766962576139804 ) ) ;
#15587 = DIRECTION ( 'NONE',  ( 0.000000000000000000, 0.000000000000000000, 1.000000000000000000 ) ) ;
#15588 = CARTESIAN_POINT ( 'NONE',  ( -34.84395483231872248, -300.0033357693390030, -194.8003003694630308 ) ) ;
#15589 = CARTESIAN_POINT ( 'NONE',  ( 25.27978124254390480, -280.2285769419000303, -232.4323528950670834 ) ) ;
#15590 = CARTESIAN_POINT ( 'NONE',  ( -95.86110629276807060, -281.9066092695691168, -317.2908288172852735 ) ) ;
#15591 = CARTESIAN_POINT ( 'NONE',  ( -22.13951346636238071, -294.0593382188949931, -345.6807856710722149 ) ) ;
#15592 = CARTESIAN_POINT ( 'NONE',  ( -72.36776059174798092, -271.8222390082464699, -205.1031827726991992 ) ) ;
#15593 = CARTESIAN_POINT ( 'NONE',  ( -6.941515913247738645, -274.7299029188646955, -338.3106801618453119 ) ) ;
#15594 = CARTESIAN_POINT ( 'NONE',  ( -107.1806343046838066, -298.1709387182804676, -247.3137143412378691 ) ) ;
#15595 = FACE_OUTER_BOUND ( 'NONE', #73538, .T. ) ;
#15596 = CARTESIAN_POINT ( 'NONE',  ( -108.4966480947757930, -294.4485538557960354, -297.1732855322821365 ) ) ;
#15597 = AXIS2_PLACEMENT_3D ( 'NONE', #49250, #460, #51104 ) ;
#15598 = CARTESIAN_POINT ( 'NONE',  ( -10.25637852233398917, -296.1168338599671301, -338.7845077774825313 ) ) ;
#15599 = DIRECTION ( 'NONE',  ( 0.000000000000000000, 0.000000000000000000, -1.000000000000000000 ) ) ;
#15600 = CARTESIAN_POINT ( 'NONE',  ( -36.98451421717186349, -295.8503687901634294, -343.5341749740960040 ) ) ;
#15601 = DIRECTION ( 'NONE',  ( -0.3307782319877045629, -0.9437085149785860994, 0.000000000000000000 ) ) ;
#15602 = CIRCLE ( 'NONE', #56443, 5.000000000000004441 ) ;
#15604 = CARTESIAN_POINT ( 'NONE',  ( -106.8692721386701265, -296.2551786450661666, -292.7714844526203706 ) ) ;
#15603 = CARTESIAN_POINT ( 'NONE',  ( -101.1128170511424571, -283.1094614313733473, -230.2157390696378627 ) ) ;
#15605 = AXIS2_PLACEMENT_3D ( 'NONE', #59729, #88571, #45946 ) ;
#15606 = CARTESIAN_POINT ( 'NONE',  ( -109.9772555785848880, -284.8745343175664857, -244.8057646412964630 ) ) ;
#15607 = CARTESIAN_POINT ( 'NONE',  ( 36.15354970941837820, -283.6965394059326400, -287.9595439960593808 ) ) ;
#15608 = CARTESIAN_POINT ( 'NONE',  ( 35.05113572283053003, -287.5512505406355217, -296.6890974025344576 ) ) ;
#15609 = CARTESIAN_POINT ( 'NONE',  ( -52.72230746304008164, -289.8546012352798584, -197.0722341398119681 ) ) ;
#15610 = CARTESIAN_POINT ( 'NONE',  ( -112.3867484786949404, -277.6906130078346564, -287.1406741517341175 ) ) ;
#15611 = CARTESIAN_POINT ( 'NONE',  ( -106.6379572354042153, -276.4809262143061233, -236.9535640164627068 ) ) ;
#15612 = AXIS2_PLACEMENT_3D ( 'NONE', #15955, #2213, #45730 ) ;
#15613 = CARTESIAN_POINT ( 'NONE',  ( -43.43026024688149533, -259.9949877806594714, -498.9966730678170279 ) ) ;
#15614 = CARTESIAN_POINT ( 'NONE',  ( -8.082631778666776512, -285.2390984480305747, -203.0481368793026604 ) ) ;
#15615 = CARTESIAN_POINT ( 'NONE',  ( -108.5167148168941225, -289.1085914890034019, -298.9200008927197700 ) ) ;
#15616 = CYLINDRICAL_SURFACE ( 'NONE', #14361, 5.999999999999998224 ) ;
#15617 = CARTESIAN_POINT ( 'NONE',  ( -75.02965664345900620, -278.9693264961290993, -336.8308421195906135 ) ) ;
#15619 = CARTESIAN_POINT ( 'NONE',  ( 15.27756267139046820, -280.4873756404109031, -219.6598301418038943 ) ) ;
#15618 = CARTESIAN_POINT ( 'NONE',  ( -3.980152954366232620, -292.6345629494124978, -337.9432552927411280 ) ) ;
#15620 = CARTESIAN_POINT ( 'NONE',  ( -34.85251716959677282, -295.1883692188969803, -347.3208735222163455 ) ) ;
#15621 = CONICAL_SURFACE ( 'NONE', #82114, 2.738891987356051327, 0.09862129276975473147 ) ;
#15622 = CARTESIAN_POINT ( 'NONE',  ( -26.79740472569955045, -284.2649598192937219, -195.4879523725978174 ) ) ;
#15623 = CARTESIAN_POINT ( 'NONE',  ( -111.7366965054040264, -280.6794707973262462, -260.4578789101729512 ) ) ;
#15624 = CARTESIAN_POINT ( 'NONE',  ( -31.59581466333957067, -294.0367225890842633, -343.4209350127624134 ) ) ;
#15625 = EDGE_LOOP ( 'NONE', ( #53579, #46500, #71098, #20534 ) ) ;
#15626 = LINE ( 'NONE', #72924, #80151 ) ;
#15627 = AXIS2_PLACEMENT_3D ( 'NONE', #21779, #42119, #79989 ) ;
#15628 = CARTESIAN_POINT ( 'NONE',  ( 19.19416639992928353, -282.8529442103424572, -221.6019670233719125 ) ) ;
#15629 = CARTESIAN_POINT ( 'NONE',  ( -106.7632923745864417, -296.3637089674620029, -247.4273004536887584 ) ) ;
#15630 = FACE_OUTER_BOUND ( 'NONE', #33085, .T. ) ;
#15631 = CARTESIAN_POINT ( 'NONE',  ( -85.28047601435909542, -270.9094976428775681, -210.1954327657594206 ) ) ;
#15632 = CARTESIAN_POINT ( 'NONE',  ( -67.46290370518146062, -272.8641379301053576, -199.6725622195420726 ) ) ;
#15633 = CARTESIAN_POINT ( 'NONE',  ( -108.1079520002728600, -290.6225939575098209, -252.3899727515743336 ) ) ;
#15634 = CARTESIAN_POINT ( 'NONE',  ( -108.2910374738124517, -280.3336870025995609, -250.3919718224957762 ) ) ;
#15635 = CARTESIAN_POINT ( 'NONE',  ( -29.92956130563193184, -275.7476633421790666, -196.9342794773952505 ) ) ;
#15636 = CARTESIAN_POINT ( 'NONE',  ( -16.34253484235405551, -284.3854089957309839, -343.6652401631999965 ) ) ;
#15637 = CARTESIAN_POINT ( 'NONE',  ( 18.78815316669153290, -281.0154728718585488, -317.6730118753061447 ) ) ;
#15638 = CARTESIAN_POINT ( 'NONE',  ( -0.4652335564866330597, -278.5625625254471629, -335.7278345602061904 ) ) ;
#15639 = VERTEX_POINT ( 'NONE', #42974 ) ;
#15640 = CARTESIAN_POINT ( 'NONE',  ( -60.86910050608528877, -273.5885139934989638, -196.9879500593584680 ) ) ;
#15641 = CARTESIAN_POINT ( 'NONE',  ( -82.62401545215251986, -293.3485412286007090, -211.2126606203711958 ) ) ;
#15642 = DIRECTION ( 'NONE',  ( -0.1727706028203382094, 0.000000000000000000, -0.9849620900324524975 ) ) ;
#15643 = FACE_OUTER_BOUND ( 'NONE', #7304, .T. ) ;
#15644 = EDGE_CURVE ( 'NONE', #54449, #93705, #66778, .T. ) ;
#15645 = CARTESIAN_POINT ( 'NONE',  ( 35.89638832292738613, -291.9386181222029677, -289.7644136533795631 ) ) ;
#15646 = CARTESIAN_POINT ( 'NONE',  ( -31.32840057402644263, -273.6377638889694595, -197.5348005380731706 ) ) ;
#15647 = DIRECTION ( 'NONE',  ( 0.000000000000000000, 1.000000000000000000, 0.000000000000000000 ) ) ;
#15648 = CARTESIAN_POINT ( 'NONE',  ( -36.40648853187516920, -293.5837930312608819, -194.0472653596006012 ) ) ;
#15650 = CARTESIAN_POINT ( 'NONE',  ( 1.485532896573637407, -293.7636489305879195, -204.2667656040680413 ) ) ;
#15649 = CARTESIAN_POINT ( 'NONE',  ( -95.95921662488163406, -286.4090924074130839, -317.1477375740089997 ) ) ;
#15651 = CARTESIAN_POINT ( 'NONE',  ( 34.78978824073960396, -289.2954485892807952, -250.4343316301820153 ) ) ;
#15652 = CARTESIAN_POINT ( 'NONE',  ( 37.43247904811050120, -273.6044406496577039, -274.4372635320963809 ) ) ;
#15653 = CARTESIAN_POINT ( 'NONE',  ( -51.53190311712203453, -279.1552107154237774, -343.4360954657726097 ) ) ;
#15654 = CARTESIAN_POINT ( 'NONE',  ( 36.63516107616717221, -291.7450886635492679, -279.1034642373022621 ) ) ;
#15655 = CARTESIAN_POINT ( 'NONE',  ( -86.02939095455678853, -281.2464614706670432, -212.2426167304207354 ) ) ;
#15656 = ORIENTED_EDGE ( 'NONE', *, *, #1219, .T. ) ;
#15657 = CARTESIAN_POINT ( 'NONE',  ( -4.821557711363796628, -282.2782934457702027, -335.7409912163431045 ) ) ;
#15658 = CARTESIAN_POINT ( 'NONE',  ( -98.33889595381744186, -280.2542030202112073, -223.8549429124280721 ) ) ;
#15659 = CIRCLE ( 'NONE', #80675, 5.343514653206204557 ) ;
#15660 = CARTESIAN_POINT ( 'NONE',  ( -55.62236848749311946, -282.0773174121798661, -344.7508073339952261 ) ) ;
#15661 = CARTESIAN_POINT ( 'NONE',  ( 18.73952676063448308, -277.2105001825364639, -322.7797807240210659 ) ) ;
#15662 = EDGE_CURVE ( 'NONE', #15179, #89341, #7449, .T. ) ;
#15663 = EDGE_CURVE ( 'NONE', #50862, #35587, #64334, .T. ) ;
#15664 = CARTESIAN_POINT ( 'NONE',  ( 32.39405704835434108, -277.4712245351720412, -301.3390443492152713 ) ) ;
#15665 = CARTESIAN_POINT ( 'NONE',  ( -6.941161984400275209, -285.1233781216987495, -333.4151289067050357 ) ) ;
#15666 = ORIENTED_EDGE ( 'NONE', *, *, #32210, .T. ) ;
#15667 = CIRCLE ( 'NONE', #53445, 24.50000000000000355 ) ;
#15668 = CARTESIAN_POINT ( 'NONE',  ( -33.71597685990347060, -300.0976955582013943, -195.3598731451911021 ) ) ;
#15669 = VECTOR ( 'NONE', #21636, 1000.000000000000000 ) ;
#15670 = CARTESIAN_POINT ( 'NONE',  ( -95.36745559087739821, -292.2599202865949906, -225.5589106980830536 ) ) ;
#15671 = CARTESIAN_POINT ( 'NONE',  ( -40.60229248747013031, -275.1134375053601957, -344.9474195032431112 ) ) ;
#15672 = CARTESIAN_POINT ( 'NONE',  ( -67.62910702470186664, -291.2042600439678495, -340.0507657006041313 ) ) ;
#15673 = CARTESIAN_POINT ( 'NONE',  ( -46.99973260817423437, -291.2748188540548426, -197.8999899439994579 ) ) ;
#15674 = CARTESIAN_POINT ( 'NONE',  ( 37.76350133194356573, -287.2695260824559114, -287.1166195608068961 ) ) ;
#15675 = DIRECTION ( 'NONE',  ( -0.9693563597868452009, -0.2456588035076220644, -3.046750416192724932E-15 ) ) ;
#15677 = CARTESIAN_POINT ( 'NONE',  ( -109.7684933844223281, -282.7671163252316546, -284.5315109020893942 ) ) ;
#15676 = CARTESIAN_POINT ( 'NONE',  ( 35.72886334755724391, -291.8441518527105245, -248.0161175045146251 ) ) ;
#15678 = CARTESIAN_POINT ( 'NONE',  ( -78.84570555296532746, -291.4780574855929558, -331.9720196402687975 ) ) ;
#15679 = CARTESIAN_POINT ( 'NONE',  ( -105.2287869595842977, -283.4147931306565624, -241.5586038003118006 ) ) ;
#15680 = CARTESIAN_POINT ( 'NONE',  ( -1.741765096175014627, -281.8496173591730667, -206.0657985231597991 ) ) ;
#15681 = CARTESIAN_POINT ( 'NONE',  ( -80.39869404468016967, -290.5609782341948630, -333.9777894127583977 ) ) ;
#15682 = VECTOR ( 'NONE', #78384, 1000.000000000000000 ) ;
#15683 = CARTESIAN_POINT ( 'NONE',  ( -39.70950334026598227, -280.5139987854534525, -197.3254273463019501 ) ) ;
#15684 = CARTESIAN_POINT ( 'NONE',  ( -16.71868838367480592, -291.1077458807506559, -196.5864603815265639 ) ) ;
#15685 = CARTESIAN_POINT ( 'NONE',  ( 38.12965419157688984, -288.1741310256004454, -255.9308200620623666 ) ) ;
#15686 = CARTESIAN_POINT ( 'NONE',  ( 30.31156959021290831, -288.5201206140747558, -307.1135440825466389 ) ) ;
#15687 = CARTESIAN_POINT ( 'NONE',  ( -79.31101823185777278, -285.6348940655125261, -210.5698675560418280 ) ) ;
#15688 = ORIENTED_EDGE ( 'NONE', *, *, #51345, .T. ) ;
#15689 = CARTESIAN_POINT ( 'NONE',  ( 200.9306832106270804, -198.2391364535880598, 0.000000000000000000 ) ) ;
#15690 = CARTESIAN_POINT ( 'NONE',  ( 36.58402615480707709, -295.6241951317577445, -287.0116963799118821 ) ) ;
#15691 = AXIS2_PLACEMENT_3D ( 'NONE', #6767, #14343, #21419 ) ;
#15692 = CARTESIAN_POINT ( 'NONE',  ( -93.34000908395449869, -294.5216563131037333, -322.5099454494621227 ) ) ;
#15693 = AXIS2_PLACEMENT_3D ( 'NONE', #73314, #38223, #88426 ) ;
#15694 = ADVANCED_FACE ( 'NONE', ( #71880 ), #86979, .F. ) ;
#15695 = CARTESIAN_POINT ( 'NONE',  ( -32.41667044919245200, -276.0474209155116796, -343.4807504083718186 ) ) ;
#15696 = CARTESIAN_POINT ( 'NONE',  ( -99.00572534570937933, -296.5128873753518519, -224.3950392202188482 ) ) ;
#15697 = CARTESIAN_POINT ( 'NONE',  ( 36.31492657235076393, -292.0016308222263319, -268.0353721416071835 ) ) ;
#15698 = CARTESIAN_POINT ( 'NONE',  ( -75.71714431431529135, -295.7726619851313785, -207.0142731760786035 ) ) ;
#15699 = CARTESIAN_POINT ( 'NONE',  ( 34.45920473183720389, -294.9577614113862865, -285.6451458672650006 ) ) ;
#15700 = CARTESIAN_POINT ( 'NONE',  ( 34.07968623757008686, -294.8496097595959782, -286.9455817794044492 ) ) ;
#15701 = CARTESIAN_POINT ( 'NONE',  ( 222.8344101925596306, 36.73669859915801794, 10.00000000000000000 ) ) ;
#15702 = VECTOR ( 'NONE', #13168, 1000.000000000000000 ) ;
#15703 = CARTESIAN_POINT ( 'NONE',  ( 14.20255407332929387, -292.3298601340402456, -325.0714303866116097 ) ) ;
#15704 = CARTESIAN_POINT ( 'NONE',  ( -37.81818092046705715, -300.0463442340226266, -195.3612717124876497 ) ) ;
#15705 = CARTESIAN_POINT ( 'NONE',  ( -71.27115696686891511, -290.4528696796340341, -335.2767519414826438 ) ) ;
#15706 = CARTESIAN_POINT ( 'NONE',  ( -23.51067229161319716, -295.2038797835400601, -342.1120413905046007 ) ) ;
#15707 = CARTESIAN_POINT ( 'NONE',  ( -76.92890028663416047, -279.5590586656325058, -334.5408551758219460 ) ) ;
#15708 = CARTESIAN_POINT ( 'NONE',  ( -42.38074216411054351, -278.6746807049123618, -194.0203927541775784 ) ) ;
#15709 = ORIENTED_EDGE ( 'NONE', *, *, #51565, .F. ) ;
#15710 = CARTESIAN_POINT ( 'NONE',  ( -107.9805766389407324, -272.2898811240633563, -239.8379718082779277 ) ) ;
#15711 = CARTESIAN_POINT ( 'NONE',  ( 32.42836794541195644, -279.2908425936963681, -244.2621535599756726 ) ) ;
#15712 = CARTESIAN_POINT ( 'NONE',  ( -110.9528672262496087, -277.2017763639781833, -250.6172295769206073 ) ) ;
#15713 = CARTESIAN_POINT ( 'NONE',  ( -100.3404162136024951, -277.1047367088375495, -229.2646613154101090 ) ) ;
#15714 = CARTESIAN_POINT ( 'NONE',  ( -94.82665083913092019, -295.8793068962090729, -224.5711199316950513 ) ) ;
#15715 = CARTESIAN_POINT ( 'NONE',  ( -92.90992337966571313, -275.2550195736002934, -219.9719367496673783 ) ) ;
#15716 = B_SPLINE_CURVE_WITH_KNOTS ( 'NONE', 3,
 ( #52129, #9023, #24170, #52582 ),
 .UNSPECIFIED., .F., .F.,
 ( 4, 4 ),
 ( 0.000000000000000000, 0.0008009674008373282583 ),
 .UNSPECIFIED. ) ;
#15717 = FACE_OUTER_BOUND ( 'NONE', #81090, .T. ) ;
#15718 = CARTESIAN_POINT ( 'NONE',  ( -111.5187946762251698, -288.4017120755921724, -283.7068696385525755 ) ) ;
#15719 = CARTESIAN_POINT ( 'NONE',  ( -111.5419714876580741, -290.2943815622888337, -290.9358532218086566 ) ) ;
#15720 = CARTESIAN_POINT ( 'NONE',  ( 18.65270835133079785, -276.8548607424910415, -220.1383267602795968 ) ) ;
#15721 = CARTESIAN_POINT ( 'NONE',  ( -107.2720668098868941, -270.9062053259660843, -243.1118168049154633 ) ) ;
#15722 = CARTESIAN_POINT ( 'NONE',  ( -60.45159488267000825, -284.9571876438917570, -197.0247525413947187 ) ) ;
#15723 = FACE_BOUND ( 'NONE', #92036, .T. ) ;
#15724 = CARTESIAN_POINT ( 'NONE',  ( -22.84022592749805369, -280.8665639038884478, -343.9980578094197767 ) ) ;
#15725 = DIRECTION ( 'NONE',  ( 0.000000000000000000, 0.000000000000000000, 1.000000000000000000 ) ) ;
#15726 = CARTESIAN_POINT ( 'NONE',  ( -32.11376847893124165, -290.9144513123974889, -197.1377792708069592 ) ) ;
#15727 = CARTESIAN_POINT ( 'NONE',  ( -104.5946170076872619, -283.1105473254152116, -238.8082966797575750 ) ) ;
#15728 = CARTESIAN_POINT ( 'NONE',  ( 196.8803347170859865, 24.42324672360809856, 12.49999999999999289 ) ) ;
#15729 = CARTESIAN_POINT ( 'NONE',  ( 113.5000000000000568, -218.8335761803644743, -490.8867980474134356 ) ) ;
#15730 = CARTESIAN_POINT ( 'NONE',  ( 37.41599315172956608, -291.6293351546223107, -276.3850653720522814 ) ) ;
#15731 = CARTESIAN_POINT ( 'NONE',  ( -108.9433452175861987, -279.9182908714823839, -288.2917687642296869 ) ) ;
#15732 = CARTESIAN_POINT ( 'NONE',  ( -88.04715580857174473, -284.9478374354295056, -327.8511397666733274 ) ) ;
#15734 = CARTESIAN_POINT ( 'NONE',  ( -102.2383922971621359, -285.0065767237442742, -236.9332950574640790 ) ) ;
#15733 = CARTESIAN_POINT ( 'NONE',  ( 20.75956128145462998, -272.9699373103212565, -222.0542072548558110 ) ) ;
#15735 = CARTESIAN_POINT ( 'NONE',  ( -16.19431822141394406, -278.1987515482655908, -340.8997570737070077 ) ) ;
#15736 = CARTESIAN_POINT ( 'NONE',  ( -70.51690510617177665, -278.3041081003494810, -335.5685370552156996 ) ) ;
#15737 = EDGE_CURVE ( 'NONE', #46977, #81769, #87975, .T. ) ;
#15738 = CARTESIAN_POINT ( 'NONE',  ( -99.74064001227507958, -285.9889349028352399, -312.0640274430530212 ) ) ;
#15739 = B_SPLINE_CURVE_WITH_KNOTS ( 'NONE', 3,
 ( #10300, #9844, #39626, #17891, #2294, #61912 ),
 .UNSPECIFIED., .F., .F.,
 ( 4, 2, 4 ),
 ( -4.472146915497830869E-06, 0.0004206930844425595313, 0.0008458583158006168900 ),
 .UNSPECIFIED. ) ;
#15740 = ORIENTED_EDGE ( 'NONE', *, *, #37853, .T. ) ;
#15741 = TOROIDAL_SURFACE ( 'NONE', #42980, 2.500000000000007994, 0.5000000000000000000 ) ;
#15742 = DIRECTION ( 'NONE',  ( 0.000000000000000000, 1.000000000000000000, 0.000000000000000000 ) ) ;
#15743 = CARTESIAN_POINT ( 'NONE',  ( -90.71360426056845938, -295.6168412863164576, -325.9362385528231698 ) ) ;
#15744 = CARTESIAN_POINT ( 'NONE',  ( 0.9921854987479219457, -288.5458788378502391, -206.2512012368181047 ) ) ;
#15745 = CARTESIAN_POINT ( 'NONE',  ( 189.9243309297870610, 249.5000000000000568, 20.22542485937349355 ) ) ;
#15746 = CARTESIAN_POINT ( 'NONE',  ( -88.47809603358389552, -294.9094976428775681, -206.1857440867352693 ) ) ;
#15747 = CARTESIAN_POINT ( 'NONE',  ( -95.66175755329258834, -278.1471443202430578, -220.5387092342852213 ) ) ;
#15748 = CARTESIAN_POINT ( 'NONE',  ( -41.98464699157413804, -290.3944247489505983, -194.3026966182522415 ) ) ;
#15749 = VECTOR ( 'NONE', #16529, 1000.000000000000000 ) ;
#15750 = CARTESIAN_POINT ( 'NONE',  ( -111.0110390225973873, -286.0288001858123721, -273.6885650728635255 ) ) ;
#15751 = CARTESIAN_POINT ( 'NONE',  ( -49.32778712253682585, -281.6574303330163502, -197.3247727152945572 ) ) ;
#15752 = CARTESIAN_POINT ( 'NONE',  ( 23.38204111116941064, -288.3540016237112695, -223.9582792730560072 ) ) ;
#15753 = CARTESIAN_POINT ( 'NONE',  ( 37.51450298795468541, -283.4927118020830790, -265.7189739419508214 ) ) ;
#15754 = CARTESIAN_POINT ( 'NONE',  ( -84.86471090653175509, -277.8534161338482704, -331.0140421337385419 ) ) ;
#15755 = CARTESIAN_POINT ( 'NONE',  ( -103.6432370432231664, -271.0139915167394520, -235.5483136870002454 ) ) ;
#15756 = CARTESIAN_POINT ( 'NONE',  ( -45.27125990234764430, -279.7877971359382627, -193.7175141029504744 ) ) ;
#15757 = AXIS2_PLACEMENT_3D ( 'NONE', #58704, #44003, #72900 ) ;
#15758 = CARTESIAN_POINT ( 'NONE',  ( -32.63600604481754175, -275.9724781262844999, -196.2624705463541659 ) ) ;
#15759 = AXIS2_PLACEMENT_3D ( 'NONE', #12406, #6247, #63570 ) ;
#15760 = DIRECTION ( 'NONE',  ( -0.000000000000000000, -0.000000000000000000, -1.000000000000000000 ) ) ;
#15761 = CARTESIAN_POINT ( 'NONE',  ( -54.42813229853333468, -285.7662352645560873, -345.3683826091709648 ) ) ;
#15762 = CARTESIAN_POINT ( 'NONE',  ( -67.11763380038603088, -271.9069839684858607, -200.4514062885034207 ) ) ;
#15763 = DIRECTION ( 'NONE',  ( -0.000000000000000000, -0.000000000000000000, 1.000000000000000000 ) ) ;
#15764 = CARTESIAN_POINT ( 'NONE',  ( -59.74654628216803331, -279.2617300106088578, -200.7663338298953875 ) ) ;
#15765 = CIRCLE ( 'NONE', #91372, 6.654241149514406040 ) ;
#15766 = CARTESIAN_POINT ( 'NONE',  ( 0.8623889957438575227, -277.7597621792862697, -336.8174971393888200 ) ) ;
#15767 = CARTESIAN_POINT ( 'NONE',  ( -35.91562233682809335, -282.0934631412376348, -347.1256543763460627 ) ) ;
#15768 = CARTESIAN_POINT ( 'NONE',  ( -23.57500759919864564, -290.6340851210343317, -343.1352824096118184 ) ) ;
#15769 = CARTESIAN_POINT ( 'NONE',  ( -36.56901364325128867, -299.5817749106086012, -194.0542508093429035 ) ) ;
#15770 = CARTESIAN_POINT ( 'NONE',  ( -34.79137658881326445, -299.2884837342763831, -193.7576786726185674 ) ) ;
#15771 = CARTESIAN_POINT ( 'NONE',  ( 37.03190257185073619, -295.6647713112477618, -279.0999586585848533 ) ) ;
#15772 = CARTESIAN_POINT ( 'NONE',  ( 37.18050840112420730, -279.4572050373725460, -262.9956068851622604 ) ) ;
#15773 = CARTESIAN_POINT ( 'NONE',  ( -62.56224024776824422, -271.7424425916609607, -200.1060743341718933 ) ) ;
#15774 = CARTESIAN_POINT ( 'NONE',  ( -112.6994222293774897, -286.2994677473962497, -258.7141483890073914 ) ) ;
#15775 = CIRCLE ( 'NONE', #59658, 4.999999999999990230 ) ;
#15776 = CARTESIAN_POINT ( 'NONE',  ( -58.79265596617397449, -288.2564142794927307, -340.5146667550876600 ) ) ;
#15777 = CARTESIAN_POINT ( 'NONE',  ( -94.25799649422008031, -240.8346478425894759, -341.8059174816269206 ) ) ;
#15778 = VERTEX_POINT ( 'NONE', #64790 ) ;
#15779 = CARTESIAN_POINT ( 'NONE',  ( 31.15113858071259401, -286.5668891689415432, -304.3527590392434945 ) ) ;
#15780 = CARTESIAN_POINT ( 'NONE',  ( -34.58145317239293348, -288.6833730786188426, -343.3796701595642276 ) ) ;
#15781 = EDGE_LOOP ( 'NONE', ( #13494, #40545, #58785, #75929 ) ) ;
#15782 = CARTESIAN_POINT ( 'NONE',  ( -87.55796226229870172, -286.4503291221897712, -212.3268524840556211 ) ) ;
#15783 = CARTESIAN_POINT ( 'NONE',  ( -59.19728555027650430, -277.6762602717579966, -340.0347921541303435 ) ) ;
#15784 = CARTESIAN_POINT ( 'NONE',  ( 27.79710632349152633, -291.9397314209022056, -229.7832409918204348 ) ) ;
#15785 = CARTESIAN_POINT ( 'NONE',  ( 13.61945179376667880, -283.0119442179482689, -328.0191005904653139 ) ) ;
#15786 = CARTESIAN_POINT ( 'NONE',  ( 25.37164984025568870, -283.6519863530356247, -313.8552863653348481 ) ) ;
#15787 = CARTESIAN_POINT ( 'NONE',  ( -93.41322580413236665, -284.1651751784793873, -323.1225336249639213 ) ) ;
#15788 = CARTESIAN_POINT ( 'NONE',  ( -19.53350555847921655, -280.6207156214569522, -199.4924618051631455 ) ) ;
#15789 = CARTESIAN_POINT ( 'NONE',  ( 21.31550574532286291, -272.4094976428775681, -223.6242672951989618 ) ) ;
#15790 = CARTESIAN_POINT ( 'NONE',  ( -55.96988853928130681, -169.5567205125497026, -364.5607778869738809 ) ) ;
#15791 = VERTEX_POINT ( 'NONE', #28773 ) ;
#15792 = CARTESIAN_POINT ( 'NONE',  ( -37.79595051760566093, -279.0579763670951934, -345.2058430138453105 ) ) ;
#15793 = CARTESIAN_POINT ( 'NONE',  ( 63.86165590144513260, 48.22071679732245997, -318.3204609132440055 ) ) ;
#15794 = CARTESIAN_POINT ( 'NONE',  ( -31.96053399027169561, -124.1536744858074144, -360.9188437396628615 ) ) ;
#15795 = CARTESIAN_POINT ( 'NONE',  ( -108.8771599182628762, -296.0998013240203477, -255.2486996240658641 ) ) ;
#15796 = CARTESIAN_POINT ( 'NONE',  ( 23.11941843600870428, -293.6968422706145816, -317.9635528164654374 ) ) ;
#15797 = CARTESIAN_POINT ( 'NONE',  ( -11.69923036777068504, -92.83970553864392627, -356.5485982400477383 ) ) ;
#15799 = CARTESIAN_POINT ( 'NONE',  ( -103.5722528561838800, -288.5156620334610693, -302.9180573094117221 ) ) ;
#15798 = CARTESIAN_POINT ( 'NONE',  ( -91.20719530715918211, -295.8791242684621920, -216.1659639444002039 ) ) ;
#15800 = CARTESIAN_POINT ( 'NONE',  ( -38.33545915039621121, -296.9251556898597642, -344.5896699455098542 ) ) ;
#15801 = CARTESIAN_POINT ( 'NONE',  ( 27.47323519179343876, -289.3376964818619967, -305.1143548479905121 ) ) ;
#15802 = ORIENTED_EDGE ( 'NONE', *, *, #55196, .F. ) ;
#15803 = CARTESIAN_POINT ( 'NONE',  ( -3.322242422785143923, -295.5552343417230645, -339.1906236281188285 ) ) ;
#15804 = CARTESIAN_POINT ( 'NONE',  ( 23.58191507446265334, -287.4843554956995035, -229.9421043074399051 ) ) ;
#15805 = CARTESIAN_POINT ( 'NONE',  ( -65.38228815324573873, -296.4886999787862010, -199.0181447060146525 ) ) ;
#15806 = CARTESIAN_POINT ( 'NONE',  ( 13.16463340631999479, -293.5402353310277022, -212.4536996931710746 ) ) ;
#15807 = ADVANCED_FACE ( 'NONE', ( #92216 ), #57656, .F. ) ;
#15808 = CARTESIAN_POINT ( 'NONE',  ( 23.12720196275153484, -294.6813772648756640, -317.9536647553479156 ) ) ;
#15809 = CARTESIAN_POINT ( 'NONE',  ( -108.4279585600876601, -290.9386064109465906, -253.7010609757184909 ) ) ;
#15810 = ORIENTED_EDGE ( 'NONE', *, *, #20342, .T. ) ;
#15811 = DIRECTION ( 'NONE',  ( 0.000000000000000000, -0.000000000000000000, 1.000000000000000000 ) ) ;
#15812 = CARTESIAN_POINT ( 'NONE',  ( -0.7643527836910239959, -276.4541324976058831, -204.2297539535574629 ) ) ;
#15813 = CARTESIAN_POINT ( 'NONE',  ( 28.17096716750732810, -273.8250393617002487, -230.5595654155608258 ) ) ;
#15814 = ADVANCED_FACE ( 'NONE', ( #79441 ), #78883, .T. ) ;
#15815 = ORIENTED_EDGE ( 'NONE', *, *, #7662, .T. ) ;
#15816 = CARTESIAN_POINT ( 'NONE',  ( 5.831565484502884367, -275.9914444384368721, -334.0446797504306460 ) ) ;
#15817 = CARTESIAN_POINT ( 'NONE',  ( -62.28108434329747922, -272.1221451649846017, -200.9027309463273809 ) ) ;
#15818 = CARTESIAN_POINT ( 'NONE',  ( 34.43045383032324480, -273.9379818480910558, -289.3248570320944850 ) ) ;
#15819 = CARTESIAN_POINT ( 'NONE',  ( -65.94638528093550178, -274.7485101320852436, -202.8629842196025947 ) ) ;
#15820 = CARTESIAN_POINT ( 'NONE',  ( -74.40277007354357863, -274.4878848261452049, -207.1368270804752569 ) ) ;
#15821 = CARTESIAN_POINT ( 'NONE',  ( -36.57141465482660436, -299.6617648581236040, -194.1609068640118494 ) ) ;
#15822 = CARTESIAN_POINT ( 'NONE',  ( -3.278009125179975669, -272.5197785983277754, -203.1301239395667437 ) ) ;
#15823 = CARTESIAN_POINT ( 'NONE',  ( -36.98673327514982390, -295.6989739534406567, -343.4746312403531192 ) ) ;
#15824 = CARTESIAN_POINT ( 'NONE',  ( -34.29482001438502436, -293.5878205805398693, -343.8872455823365044 ) ) ;
#15825 = DIRECTION ( 'NONE',  ( -1.000000000000000000, -0.000000000000000000, -0.000000000000000000 ) ) ;
#15826 = CARTESIAN_POINT ( 'NONE',  ( -35.70652650738632161, -277.5245315989930077, -347.2953146444539811 ) ) ;
#15827 = CARTESIAN_POINT ( 'NONE',  ( 33.50866773477660843, -275.4867835498943691, -252.7763126600675605 ) ) ;
#15828 = CARTESIAN_POINT ( 'NONE',  ( -108.8480569770757285, -282.8887269668780959, -297.7143281265255155 ) ) ;
#15829 = CARTESIAN_POINT ( 'NONE',  ( -89.42299444709324518, -297.7833327765368949, -324.6320819047000441 ) ) ;
#15830 = CARTESIAN_POINT ( 'NONE',  ( 175.2296996224750103, 247.0000000000001137, 0.000000000000000000 ) ) ;
#15831 = CARTESIAN_POINT ( 'NONE',  ( -77.12832246288606086, -284.7013812388969427, -208.9037307011588211 ) ) ;
#15832 = VECTOR ( 'NONE', #3802, 1000.000000000000000 ) ;
#15833 = CARTESIAN_POINT ( 'NONE',  ( -108.8044456165321776, -276.5410567607178223, -289.6237767427979293 ) ) ;
#15834 = CARTESIAN_POINT ( 'NONE',  ( -59.38867912442427865, -275.9179900232000477, -340.5701318852129020 ) ) ;
#15835 = CARTESIAN_POINT ( 'NONE',  ( 19.46028180675816799, -284.2314646432311065, -319.3552285864406599 ) ) ;
#15836 = CARTESIAN_POINT ( 'NONE',  ( -19.18817475961845886, -275.4959466997436266, -199.1917435567324333 ) ) ;
#15837 = DIRECTION ( 'NONE',  ( 0.000000000000000000, 0.000000000000000000, 1.000000000000000000 ) ) ;
#15838 = CARTESIAN_POINT ( 'NONE',  ( 21.10378306268967208, -274.6169536895415604, -319.2545317751090010 ) ) ;
#15839 = CARTESIAN_POINT ( 'NONE',  ( -20.19967638916713426, -282.2719182001559375, -197.1217323681618439 ) ) ;
#15840 = DIRECTION ( 'NONE',  ( -0.000000000000000000, -1.000000000000000000, -0.000000000000000000 ) ) ;
#15841 = CARTESIAN_POINT ( 'NONE',  ( 0.7737664981769470929, -288.4764068715076064, -205.1040166087259990 ) ) ;
#15842 = CARTESIAN_POINT ( 'NONE',  ( -100.2168347810491724, -289.1043477193641138, -229.3815903185768832 ) ) ;
#15843 = CIRCLE ( 'NONE', #68758, 4.025000000000000355 ) ;
#15844 = CARTESIAN_POINT ( 'NONE',  ( 180.5131398354828320, 275.5000000000000568, -23.92352941176473635 ) ) ;
#15845 = CARTESIAN_POINT ( 'NONE',  ( -101.1375842259761981, -271.7348080440483500, -233.7714437810683421 ) ) ;
#15846 = CARTESIAN_POINT ( 'NONE',  ( -108.9231018478902939, -288.4339240464086060, -290.2222898316994701 ) ) ;
#15847 = CARTESIAN_POINT ( 'NONE',  ( 197.9739649220119588, 291.4634315377682583, -67.91333382494548232 ) ) ;
#15848 = CARTESIAN_POINT ( 'NONE',  ( 201.2104617360081704, 60.19600395700749829, -10.00000000000000000 ) ) ;
#15849 = CARTESIAN_POINT ( 'NONE',  ( 0.3597301801255887166, -287.0396685991814252, -336.7631898778850541 ) ) ;
#15850 = CARTESIAN_POINT ( 'NONE',  ( -57.46570152981070834, -284.0358730944445824, -197.0330485416895385 ) ) ;
#15851 = CARTESIAN_POINT ( 'NONE',  ( -83.82903660226966736, -291.3927718394438102, -214.0767724899135374 ) ) ;
#15852 = CARTESIAN_POINT ( 'NONE',  ( 35.93731676802683950, -282.8820859717162080, -263.0751017122723283 ) ) ;
#15853 = CARTESIAN_POINT ( 'NONE',  ( 17.73314211791389994, -283.0405946407308875, -318.5208883191551195 ) ) ;
#15854 = CARTESIAN_POINT ( 'NONE',  ( -59.51863613430510469, -291.3178376571415242, -342.3791039995995220 ) ) ;
#15855 = CARTESIAN_POINT ( 'NONE',  ( -99.55247379169004773, -273.4883377789485053, -224.9343960973226046 ) ) ;
#15856 = CARTESIAN_POINT ( 'NONE',  ( -48.67756867471482707, -287.2751222521179670, -345.1188901777998126 ) ) ;
#15857 = CARTESIAN_POINT ( 'NONE',  ( 11.78569239055504880, -274.7124983179081141, -211.0001866675216888 ) ) ;
#15858 = CARTESIAN_POINT ( 'NONE',  ( -52.73300147527349679, -293.8340134860398507, -197.2672699442896658 ) ) ;
#15859 = CARTESIAN_POINT ( 'NONE',  ( 169.9358031814915080, 214.6007075219706621, -24.43326837773184934 ) ) ;
#15860 = CARTESIAN_POINT ( 'NONE',  ( -85.28047601435908120, -298.1948066931273615, -330.5268031993605859 ) ) ;
#15861 = CARTESIAN_POINT ( 'NONE',  ( -29.40795054730552494, -281.6345175559641234, -343.4756271270165939 ) ) ;
#15862 = EDGE_CURVE ( 'NONE', #33370, #72504, #6299, .T. ) ;
#15863 = CARTESIAN_POINT ( 'NONE',  ( -69.53939256847833406, -275.4747023180252654, -338.2967640226538037 ) ) ;
#15864 = EDGE_CURVE ( 'NONE', #4269, #52800, #42738, .T. ) ;
#15865 = CARTESIAN_POINT ( 'NONE',  ( 139.6925840978351516, -43.55766379199612004, 22.50000000000000000 ) ) ;
#15866 = CARTESIAN_POINT ( 'NONE',  ( -112.4192724977080502, -294.7835768336193496, -283.6904141885146942 ) ) ;
#15867 = CIRCLE ( 'NONE', #80874, 4.999999999999984013 ) ;
#15868 = CARTESIAN_POINT ( 'NONE',  ( 34.26273633242944072, -275.0946559646685614, -285.0817615718671050 ) ) ;
#15869 = CARTESIAN_POINT ( 'NONE',  ( -60.49499394487303050, -293.2666145312089725, -200.3459167165141253 ) ) ;
#15870 = CARTESIAN_POINT ( 'NONE',  ( 20.71704865997834588, -295.1198167787104012, -315.0200924110563960 ) ) ;
#15871 = CARTESIAN_POINT ( 'NONE',  ( -105.0311366971539826, -285.9149389863769670, -300.2962843925435550 ) ) ;
#15872 = CARTESIAN_POINT ( 'NONE',  ( 3.808804004809474453, -294.0193454912460425, -205.9148541086267130 ) ) ;
#15873 = CARTESIAN_POINT ( 'NONE',  ( 31.73346565615385728, -294.4415800110484156, -237.3455084458495605 ) ) ;
#15874 = CARTESIAN_POINT ( 'NONE',  ( -67.29715047758752178, -295.2895583513290489, -336.9456211854137564 ) ) ;
#15875 = CARTESIAN_POINT ( 'NONE',  ( -100.5129852052107395, -292.0079916843238266, -310.7887000235631376 ) ) ;
#15876 = CARTESIAN_POINT ( 'NONE',  ( -92.43225546529755832, -283.9808764911872458, -324.1573141040151427 ) ) ;
#15877 = CARTESIAN_POINT ( 'NONE',  ( -33.40300596452087944, -296.1809437869289354, -194.8023867302687506 ) ) ;
#15878 = CARTESIAN_POINT ( 'NONE',  ( -107.0065457804658564, -283.9653439342915249, -303.1606497583886153 ) ) ;
#15879 = CARTESIAN_POINT ( 'NONE',  ( -95.72406915748916845, -279.8894060920168840, -316.8933080821197450 ) ) ;
#15880 = CARTESIAN_POINT ( 'NONE',  ( -33.20099175315139206, -284.9002324454621089, -197.0308457171405223 ) ) ;
#15881 = CARTESIAN_POINT ( 'NONE',  ( 36.07122548115266625, -285.3541356083511005, -254.9514249164482464 ) ) ;
#15882 = CARTESIAN_POINT ( 'NONE',  ( -99.22617866293555267, -277.2795860729529522, -226.6505151729262479 ) ) ;
#15883 = CARTESIAN_POINT ( 'NONE',  ( -32.04911714649202992, -124.5213432794980974, -365.6788127701597659 ) ) ;
#15884 = CARTESIAN_POINT ( 'NONE',  ( -67.56743679874085728, -285.1522027307956364, -203.8450050131483522 ) ) ;
#15885 = CARTESIAN_POINT ( 'NONE',  ( 25.61280253863908030, -283.3369909798606727, -314.0275131697265465 ) ) ;
#15886 = CARTESIAN_POINT ( 'NONE',  ( -80.41852276767058072, -288.6787774023308657, -333.9643640420392217 ) ) ;
#15887 = CARTESIAN_POINT ( 'NONE',  ( -98.99041047885765465, -279.5515372482508383, -315.1703149527498340 ) ) ;
#15888 = CARTESIAN_POINT ( 'NONE',  ( -96.66133552830895326, -279.2145446872268622, -318.6980759225766633 ) ) ;
#15889 = CARTESIAN_POINT ( 'NONE',  ( -39.69910605584753682, -279.8550781085256745, -197.3866722092923851 ) ) ;
#15890 = CARTESIAN_POINT ( 'NONE',  ( -4.609045273264730902, -276.4653987453200443, -203.2618146295105248 ) ) ;
#15891 = CARTESIAN_POINT ( 'NONE',  ( 35.45261220471979868, -293.2339486485220732, -245.1001564367266212 ) ) ;
#15892 = CARTESIAN_POINT ( 'NONE',  ( -11.36221711908693699, -284.3912514542772669, -200.1820976934847067 ) ) ;
#15893 = CARTESIAN_POINT ( 'NONE',  ( 3.693376998837470726, -294.1941734058470388, -206.0913973756002804 ) ) ;
#15894 = CARTESIAN_POINT ( 'NONE',  ( -4.209203439874178443, -293.5250542679443129, -335.7698510459715635 ) ) ;
#15895 = CARTESIAN_POINT ( 'NONE',  ( 16.17174615579032704, -293.9327703463718535, -320.0440985052070459 ) ) ;
#15896 = CARTESIAN_POINT ( 'NONE',  ( -109.1891016106313685, -291.9741175021994763, -243.3872642888283622 ) ) ;
#15897 = AXIS2_PLACEMENT_3D ( 'NONE', #76173, #2803, #39220 ) ;
#15898 = CARTESIAN_POINT ( 'NONE',  ( 26.54390395016679349, -281.7184280983207145, -234.8291287410467021 ) ) ;
#15899 = CARTESIAN_POINT ( 'NONE',  ( -23.41573227742476604, -297.1429999092800927, -193.6727113408300909 ) ) ;
#15900 = CARTESIAN_POINT ( 'NONE',  ( 38.18850224560330986, -288.0227361338855303, -255.9215433258822827 ) ) ;
#15901 = CARTESIAN_POINT ( 'NONE',  ( 6.195537895881389368, -280.6081295510135192, -332.4318260222510730 ) ) ;
#15902 = CARTESIAN_POINT ( 'NONE',  ( -70.62608484619411797, -289.8123273752514137, -339.7866506870747685 ) ) ;
#15903 = CARTESIAN_POINT ( 'NONE',  ( -65.10519041269610341, -286.0125392203438537, -202.7700729462104050 ) ) ;
#15904 = DIRECTION ( 'NONE',  ( -0.000000000000000000, -1.000000000000000000, 0.000000000000000000 ) ) ;
#15905 = CARTESIAN_POINT ( 'NONE',  ( -90.98605276365739769, -229.1079664473872413, -346.1131341628189375 ) ) ;
#15906 = CARTESIAN_POINT ( 'NONE',  ( 45.01749665140694390, 11.19730123446569081, -328.3103152587933664 ) ) ;
#15907 = AXIS2_PLACEMENT_3D ( 'NONE', #7619, #86683, #30807 ) ;
#15908 = CARTESIAN_POINT ( 'NONE',  ( -68.58298753371472856, -278.8278934792664927, -204.2053647272176988 ) ) ;
#15909 = CARTESIAN_POINT ( 'NONE',  ( -109.1874494767653516, -277.6647556635431897, -255.7236955823417475 ) ) ;
#15910 = CARTESIAN_POINT ( 'NONE',  ( -113.0467096792613972, -272.3968957623358165, -256.1304345755483496 ) ) ;
#15911 = CARTESIAN_POINT ( 'NONE',  ( -81.55632558770187757, -219.7645460677553899, -349.7766062465405525 ) ) ;
#15912 = CARTESIAN_POINT ( 'NONE',  ( -35.33318618733856908, -278.6516012964420383, -193.9637106765003693 ) ) ;
#15913 = CARTESIAN_POINT ( 'NONE',  ( 14.79984501326969237, -296.0895561520632668, -325.6352826736072643 ) ) ;
#15914 = AXIS2_PLACEMENT_3D ( 'NONE', #17430, #69018, #74720 ) ;
#15915 = CARTESIAN_POINT ( 'NONE',  ( -47.00880822376538504, -292.4183950030986239, -197.9419529595729728 ) ) ;
#15916 = CARTESIAN_POINT ( 'NONE',  ( -33.35518257146905796, -298.9037006361731414, -193.5220654726613816 ) ) ;
#15917 = CARTESIAN_POINT ( 'NONE',  ( -31.85111590134202686, -287.6663828040902899, -343.6998511869097115 ) ) ;
#15918 = CARTESIAN_POINT ( 'NONE',  ( -20.53292325580157041, -298.7496616662710949, -193.4212930106775161 ) ) ;
#15919 = CARTESIAN_POINT ( 'NONE',  ( -108.1754613256751867, -296.9523789220810386, -252.6583560709639187 ) ) ;
#15920 = EDGE_LOOP ( 'NONE', ( #24151, #50514, #36761, #12885 ) ) ;
#15921 = LINE ( 'NONE', #8336, #88543 ) ;
#15922 = CARTESIAN_POINT ( 'NONE',  ( -38.17894846926897401, -281.9618848822379391, -194.8057527372322966 ) ) ;
#15923 = B_SPLINE_CURVE_WITH_KNOTS ( 'NONE', 3,
 ( #23125, #52935, #45826, #68090 ),
 .UNSPECIFIED., .F., .F.,
 ( 4, 4 ),
 ( 0.000000000000000000, 0.001074155171061463854 ),
 .UNSPECIFIED. ) ;
#15924 = CARTESIAN_POINT ( 'NONE',  ( -109.5883790293937778, -279.4674996136322420, -282.8708092280111259 ) ) ;
#15925 = CARTESIAN_POINT ( 'NONE',  ( -79.64321512363108013, -279.3750100342851397, -333.5477849375291726 ) ) ;
#15926 = CARTESIAN_POINT ( 'NONE',  ( -85.75117965112542606, -271.8478354881674477, -214.7302729333593163 ) ) ;
#15927 = CARTESIAN_POINT ( 'NONE',  ( 209.4952545125645145, 27.94237698917519452, 13.96055292456872898 ) ) ;
#15928 = DIRECTION ( 'NONE',  ( -0.000000000000000000, 1.000000000000000000, -0.000000000000000000 ) ) ;
#15929 = CARTESIAN_POINT ( 'NONE',  ( 26.45781019393561806, -281.2337729652594476, -234.8840481041486896 ) ) ;
#15930 = CARTESIAN_POINT ( 'NONE',  ( 36.73268832053429378, -276.6119308294917118, -290.8343009444925542 ) ) ;
#15931 = CARTESIAN_POINT ( 'NONE',  ( -6.094197931968958315, -278.6416711544894156, -338.5417182950293977 ) ) ;
#15932 = CARTESIAN_POINT ( 'NONE',  ( -56.79170282384747281, -275.8727652911543942, -344.3096208910608880 ) ) ;
#15933 = ORIENTED_EDGE ( 'NONE', *, *, #37438, .T. ) ;
#15934 = DIRECTION ( 'NONE',  ( -0.8660254037844410391, 0.000000000000000000, -0.4999999999999960032 ) ) ;
#15935 = CARTESIAN_POINT ( 'NONE',  ( -22.03492582838287106, -284.8368732810368442, -344.1453267289542737 ) ) ;
#15936 = CARTESIAN_POINT ( 'NONE',  ( -36.19336221950214849, -291.2640432893157367, -197.1961496731574641 ) ) ;
#15937 = CARTESIAN_POINT ( 'NONE',  ( -54.93322377169864268, -285.1802831239406828, -195.5022435442901099 ) ) ;
#15938 = CARTESIAN_POINT ( 'NONE',  ( -92.43411711634762185, -282.0941886324004031, -319.8048815337610336 ) ) ;
#15939 = CARTESIAN_POINT ( 'NONE',  ( -78.72283324967605722, -282.1966108107049536, -331.2132069982210965 ) ) ;
#15940 = CARTESIAN_POINT ( 'NONE',  ( -38.37478025898267475, -281.2439995241444990, -196.9588460392263585 ) ) ;
#15941 = CARTESIAN_POINT ( 'NONE',  ( 84.21812863670487559, 83.45443854015287855, -302.1763853752734690 ) ) ;
#15942 = CARTESIAN_POINT ( 'NONE',  ( -68.87420532806851270, -281.8597041497235978, -339.7449853301349094 ) ) ;
#15943 = CARTESIAN_POINT ( 'NONE',  ( 23.28500189172707380, -296.1541468748567354, -314.5348119044927557 ) ) ;
#15944 = CARTESIAN_POINT ( 'NONE',  ( -104.3615276920238699, -278.8100721612821076, -299.6809964782769384 ) ) ;
#15945 = CARTESIAN_POINT ( 'NONE',  ( -46.31257577213033017, -287.9387348551020409, -195.7316880277365101 ) ) ;
#15946 = CARTESIAN_POINT ( 'NONE',  ( 196.7383257810085979, 24.47698789593438917, 11.00000000000000000 ) ) ;
#15947 = CARTESIAN_POINT ( 'NONE',  ( -100.4941334670849642, -293.0291063376437819, -228.7812293942942006 ) ) ;
#15948 = CARTESIAN_POINT ( 'NONE',  ( 33.99278675747681433, -273.8510802729205125, -293.5212481501260413 ) ) ;
#15949 = CARTESIAN_POINT ( 'NONE',  ( -12.28606465868557329, -287.9316237590953165, -343.0555225710816103 ) ) ;
#15950 = CARTESIAN_POINT ( 'NONE',  ( -30.71506785053314914, -290.5371847694526650, -196.8592257636908300 ) ) ;
#15951 = CARTESIAN_POINT ( 'NONE',  ( -109.2507453764554413, -277.0381129366954269, -285.5378334026153766 ) ) ;
#15952 = CARTESIAN_POINT ( 'NONE',  ( -110.2544665096139624, -294.8735690269878091, -256.3438328149949825 ) ) ;
#15953 = CARTESIAN_POINT ( 'NONE',  ( -110.8299773619172015, -291.8562414405818686, -271.2076318766708596 ) ) ;
#15954 = DIRECTION ( 'NONE',  ( -0.000000000000000000, -1.000000000000000000, -0.000000000000000000 ) ) ;
#15955 = CARTESIAN_POINT ( 'NONE',  ( 197.2116943569230330, 250.5000000000000568, -12.92446933126074882 ) ) ;
#15956 = CARTESIAN_POINT ( 'NONE',  ( 39.01782031851747945, -292.0316349883576663, -270.3297410190102710 ) ) ;
#15957 = CARTESIAN_POINT ( 'NONE',  ( 15.58923712835949082, -288.4167404178641618, -218.9339238530691318 ) ) ;
#15958 = CARTESIAN_POINT ( 'NONE',  ( -94.70820682386745659, -288.1095375210364296, -320.1914092210054719 ) ) ;
#15959 = CARTESIAN_POINT ( 'NONE',  ( -10.49233490484472853, -290.1202742494306790, -338.9321004164506803 ) ) ;
#15960 = CARTESIAN_POINT ( 'NONE',  ( 175.2296996224749250, 275.5000000000000568, -24.99999999999999289 ) ) ;
#15961 = CARTESIAN_POINT ( 'NONE',  ( 28.37728414301563973, -288.7895063551759449, -302.5110298454625308 ) ) ;
#15962 = CARTESIAN_POINT ( 'NONE',  ( -34.88251444973987958, -297.0012882059284607, -345.6761842802283127 ) ) ;
#15963 = DIRECTION ( 'NONE',  ( 0.000000000000000000, -1.000000000000000000, 0.000000000000000000 ) ) ;
#15964 = CARTESIAN_POINT ( 'NONE',  ( -41.72243194040052572, -290.3112279792222239, -346.8518367590256730 ) ) ;
#15965 = CARTESIAN_POINT ( 'NONE',  ( -111.1022407369145526, -276.7701167893360434, -254.8785703103167464 ) ) ;
#15966 = CARTESIAN_POINT ( 'NONE',  ( -112.3820702055426466, -279.1001805600450325, -253.1946637674726901 ) ) ;
#15967 = CARTESIAN_POINT ( 'NONE',  ( -48.11162366469079643, -279.5855622687032564, -194.0855526428520363 ) ) ;
#15968 = CARTESIAN_POINT ( 'NONE',  ( -107.4250137091842703, -282.8990944422551479, -243.6528832169257157 ) ) ;
#15969 = CARTESIAN_POINT ( 'NONE',  ( 150.6539576904058606, 293.9636489450775230, 0.000000000000000000 ) ) ;
#15970 = CARTESIAN_POINT ( 'NONE',  ( -82.01258227717343630, -277.5758828579101873, -211.0059641890439366 ) ) ;
#15971 = ADVANCED_FACE ( 'NONE', ( #59524 ), #23523, .F. ) ;
#15972 = CARTESIAN_POINT ( 'NONE',  ( -107.4429284448295761, -282.2038508074141419, -297.1671448048194293 ) ) ;
#15973 = CARTESIAN_POINT ( 'NONE',  ( 26.24832811123609133, -24.45034257384636334, -341.6199305999596163 ) ) ;
#15974 = CARTESIAN_POINT ( 'NONE',  ( -105.5470917296300115, -277.4775168405614068, -236.0275290323528168 ) ) ;
#15975 = AXIS2_PLACEMENT_3D ( 'NONE', #91706, #26858, #12666 ) ;
#15976 = CARTESIAN_POINT ( 'NONE',  ( -37.84651135024520840, -299.5658396127653305, -196.6695111315174813 ) ) ;
#15977 = CARTESIAN_POINT ( 'NONE',  ( -105.5156940864888071, -283.0166399422415111, -305.6025031000589820 ) ) ;
#15978 = CARTESIAN_POINT ( 'NONE',  ( -78.95529992700123501, -274.2782271399448177, -210.1255761164408113 ) ) ;
#15979 = CARTESIAN_POINT ( 'NONE',  ( -57.98005124871750127, -275.2160329142224100, -196.7352989101937339 ) ) ;
#15980 = CARTESIAN_POINT ( 'NONE',  ( 33.85532700170085718, -275.0043060808779956, -254.0857411769362670 ) ) ;
#15981 = CARTESIAN_POINT ( 'NONE',  ( -70.58835413796140301, -297.4907178387658178, -337.5895394291843559 ) ) ;
#15982 = CARTESIAN_POINT ( 'NONE',  ( -31.82465905316621857, -289.1511588016697942, -347.2157719042038480 ) ) ;
#15983 = CARTESIAN_POINT ( 'NONE',  ( -20.06133236464767577, -278.3522344582344203, -196.7498858325006097 ) ) ;
#15984 = CARTESIAN_POINT ( 'NONE',  ( -113.6658509090508176, -290.5176634014234764, -259.7912570798114302 ) ) ;
#15985 = CARTESIAN_POINT ( 'NONE',  ( -23.75323706710615923, -287.9331266285080346, -342.3765984985037107 ) ) ;
#15986 = CARTESIAN_POINT ( 'NONE',  ( 24.84913480755347237, -290.9838813688306232, -228.3495466137204630 ) ) ;
#15987 = VERTEX_POINT ( 'NONE', #73265 ) ;
#15988 = CARTESIAN_POINT ( 'NONE',  ( 198.9432932128748632, 67.99483610340296025, 10.39078689545250711 ) ) ;
#15989 = CARTESIAN_POINT ( 'NONE',  ( -110.3681053163185339, -290.0130823218111686, -273.9056959723057503 ) ) ;
#15990 = CARTESIAN_POINT ( 'NONE',  ( 125.0516381006429043, 8.053287430127898716, 22.50000000000000000 ) ) ;
#15991 = CARTESIAN_POINT ( 'NONE',  ( 26.15597618984440942, -287.9226188571277589, -227.1998933662609943 ) ) ;
#15992 = CARTESIAN_POINT ( 'NONE',  ( -53.35057174420112602, -288.3376638359845288, -200.3683826091709648 ) ) ;
#15993 = CARTESIAN_POINT ( 'NONE',  ( -71.97862873181199461, -294.5576543056366177, -338.8673468289770767 ) ) ;
#15994 = CARTESIAN_POINT ( 'NONE',  ( -27.41935687340967931, -284.2439015776776046, -346.2748353269673771 ) ) ;
#15995 = CARTESIAN_POINT ( 'NONE',  ( -81.47688983342892755, -285.2656708238984606, -212.2140197389120715 ) ) ;
#15996 = CARTESIAN_POINT ( 'NONE',  ( 14.08831880860145880, -277.6270861099894773, -322.9315021422164023 ) ) ;
#15997 = CARTESIAN_POINT ( 'NONE',  ( 37.17842697681656716, -291.5060297671319631, -265.2277950931076589 ) ) ;
#15998 = CARTESIAN_POINT ( 'NONE',  ( -13.92430640745994808, -273.1578094841852931, -200.7999493921857095 ) ) ;
#15999 = ORIENTED_EDGE ( 'NONE', *, *, #11999, .T. ) ;
#16000 = CARTESIAN_POINT ( 'NONE',  ( 195.4987509559167904, 41.28370916884458808, 12.85659709285176611 ) ) ;
#16001 = CARTESIAN_POINT ( 'NONE',  ( 8.890071546132155333, -294.1039135029694762, -331.9108343044175058 ) ) ;
#16002 = CARTESIAN_POINT ( 'NONE',  ( -1.514382050981514460, -288.4507612945305368, -205.0521037722574533 ) ) ;
#16003 = CARTESIAN_POINT ( 'NONE',  ( -111.9767195722728133, -297.8533098234541967, -252.7229099152794447 ) ) ;
#16004 = CARTESIAN_POINT ( 'NONE',  ( 35.65388830598798364, -288.1404780496431499, -265.5717704489886160 ) ) ;
#16005 = CARTESIAN_POINT ( 'NONE',  ( -95.97724669800747677, -276.9411765550994460, -319.9262680029857506 ) ) ;
#16006 = CARTESIAN_POINT ( 'NONE',  ( 38.22352988415124031, -294.0250459441383555, -256.1059855716057427 ) ) ;
#16007 = CARTESIAN_POINT ( 'NONE',  ( 33.70432100556923416, -285.3535576477246423, -244.0406248269138132 ) ) ;
#16008 = CARTESIAN_POINT ( 'NONE',  ( -5.802482194022864803, -294.9819628773301474, -340.5823542556489087 ) ) ;
#16009 = CARTESIAN_POINT ( 'NONE',  ( -30.80930709945117840, -292.4702824665305911, -197.6327512465219911 ) ) ;
#16010 = CARTESIAN_POINT ( 'NONE',  ( 202.9738562182569694, 293.9636489450776367, -54.00000000000000000 ) ) ;
#16011 = DIRECTION ( 'NONE',  ( -0.000000000000000000, -1.000000000000000000, -0.000000000000000000 ) ) ;
#16012 = CARTESIAN_POINT ( 'NONE',  ( 121.9599628496891199, 147.3134478266455858, -260.3665198286096256 ) ) ;
#16013 = CARTESIAN_POINT ( 'NONE',  ( 37.15234745078601719, -289.2816694478893851, -286.9539744732303461 ) ) ;
#16014 = CARTESIAN_POINT ( 'NONE',  ( 40.64545035920995986, -291.2666405000203440, -288.1938231032136741 ) ) ;
#16015 = ORIENTED_EDGE ( 'NONE', *, *, #5207, .F. ) ;
#16017 = EDGE_CURVE ( 'NONE', #65497, #41863, #15484, .T. ) ;
#16016 = CARTESIAN_POINT ( 'NONE',  ( -7.138634476440246068, -281.5666852245482232, -337.1730985148406035 ) ) ;
#16018 = CARTESIAN_POINT ( 'NONE',  ( -99.40830359821914897, -278.8240376995777297, -224.8033809663859017 ) ) ;
#16019 = CARTESIAN_POINT ( 'NONE',  ( -2.312924976743116812, -282.5169013330373105, -204.2178230401108294 ) ) ;
#16020 = CARTESIAN_POINT ( 'NONE',  ( 140.7620216225690513, 178.5875772026313655, -240.1871175959595917 ) ) ;
#16021 = CARTESIAN_POINT ( 'NONE',  ( -110.9289524669257503, -282.8670230415570472, -290.9407823859006612 ) ) ;
#16022 = CARTESIAN_POINT ( 'NONE',  ( -14.02889745157004597, -284.3760360332855726, -199.3959674231889210 ) ) ;
#16023 = CARTESIAN_POINT ( 'NONE',  ( -1.900611152839966067, -276.3769347467678017, -203.3966894039688214 ) ) ;
#16024 = CARTESIAN_POINT ( 'NONE',  ( -37.15574612518469166, -298.5468983951584505, -197.2967118480558781 ) ) ;
#16025 = CARTESIAN_POINT ( 'NONE',  ( -7.805381360236214761, -293.3416322997192651, -337.6715115575364052 ) ) ;
#16026 = CARTESIAN_POINT ( 'NONE',  ( -114.1297772558595369, -279.1520765492772398, -274.4725650905581915 ) ) ;
#16027 = CARTESIAN_POINT ( 'NONE',  ( 13.73132837925489191, -276.3121239811382566, -322.5903691034905023 ) ) ;
#16028 = CARTESIAN_POINT ( 'NONE',  ( -97.57884793293831649, -274.2691969759052313, -222.8955669411934082 ) ) ;
#16029 = CARTESIAN_POINT ( 'NONE',  ( -34.31710452439213554, -275.9352915484344066, -346.9923409395666454 ) ) ;
#16030 = CARTESIAN_POINT ( 'NONE',  ( 44.71985729433082923, 12.68782823267609317, -331.8881429784909756 ) ) ;
#16031 = CARTESIAN_POINT ( 'NONE',  ( 37.45749664270536528, -273.4730664455656779, -264.2145073729544151 ) ) ;
#16032 = CARTESIAN_POINT ( 'NONE',  ( -79.13936011121289482, -297.0295013246803819, -334.3264360214186581 ) ) ;
#16033 = CARTESIAN_POINT ( 'NONE',  ( 35.77081079830085031, -277.8376638359845288, -253.6410175316879361 ) ) ;
#16034 = CARTESIAN_POINT ( 'NONE',  ( -75.88346903603265048, -208.4961600436150491, -353.2410745688453062 ) ) ;
#16035 = CARTESIAN_POINT ( 'NONE',  ( -92.78392803130417121, -284.9511082673145665, -318.3425501721818023 ) ) ;
#16036 = CARTESIAN_POINT ( 'NONE',  ( -96.37083773251768548, -285.6617165488259502, -318.2306435912695406 ) ) ;
#16037 = CARTESIAN_POINT ( 'NONE',  ( -79.49530807252376974, -277.8719472713040091, -209.7846064390230936 ) ) ;
#16038 = CARTESIAN_POINT ( 'NONE',  ( -94.21645785844144427, -287.0787547989395989, -222.6523408437553542 ) ) ;
#16039 = CARTESIAN_POINT ( 'NONE',  ( -70.03057599244034748, -278.0933810515128926, -204.3006055294051464 ) ) ;
#16040 = CARTESIAN_POINT ( 'NONE',  ( 29.44149659727181856, -277.0376205212172067, -300.5973662254262422 ) ) ;
#16041 = CARTESIAN_POINT ( 'NONE',  ( 199.3803347170859865, 17.19615242270662847, 9.999999999999996447 ) ) ;
#16042 = CARTESIAN_POINT ( 'NONE',  ( -63.33447121381287559, -274.1965124705897097, -202.0661048834799658 ) ) ;
#16043 = CIRCLE ( 'NONE', #75048, 1.999999999999988454 ) ;
#16044 = CARTESIAN_POINT ( 'NONE',  ( 27.70918862855555886, -281.8172271736654011, -229.3647172867792960 ) ) ;
#16045 = CARTESIAN_POINT ( 'NONE',  ( 39.21753779596305378, -282.1464396975984528, -278.5057770675436473 ) ) ;
#16046 = ORIENTED_EDGE ( 'NONE', *, *, #85141, .T. ) ;
#16047 = EDGE_LOOP ( 'NONE', ( #11098, #86357 ) ) ;
#16048 = CARTESIAN_POINT ( 'NONE',  ( 200.7741138073446621, 15.52361751443386950, -10.00000000000000178 ) ) ;
#16049 = CARTESIAN_POINT ( 'NONE',  ( 37.74787919503628331, -289.2842867356879424, -260.2685188536830765 ) ) ;
#16050 = CARTESIAN_POINT ( 'NONE',  ( -110.3728692653498769, -295.8067645240708430, -265.9964804282588489 ) ) ;
#16051 = CARTESIAN_POINT ( 'NONE',  ( -44.87878834859591848, -291.3078362498685010, -193.7804598259594115 ) ) ;
#16052 = CARTESIAN_POINT ( 'NONE',  ( 30.05134854030556824, -286.4309944584211962, -300.3018195713866021 ) ) ;
#16053 = CARTESIAN_POINT ( 'NONE',  ( -73.85295584869059837, -288.1218602330084195, -334.2685510387424870 ) ) ;
#16054 = CARTESIAN_POINT ( 'NONE',  ( 2.650589609416499570, -287.8068680873333278, -208.8164409923248002 ) ) ;
#16055 = CARTESIAN_POINT ( 'NONE',  ( -98.84052424263423120, -275.9694145365216968, -313.2900742052197529 ) ) ;
#16056 = CARTESIAN_POINT ( 'NONE',  ( -5.974618698033269837, -287.0465638603076854, -339.8056758700995488 ) ) ;
#16057 = CARTESIAN_POINT ( 'NONE',  ( 35.42991462233113253, -289.3192266963542352, -252.2146930160136833 ) ) ;
#16058 = CARTESIAN_POINT ( 'NONE',  ( -36.14226692367611804, -287.0370230906651159, -345.5310172501127681 ) ) ;
#16059 = CARTESIAN_POINT ( 'NONE',  ( -37.52912586339792256, -283.9958444141489622, -343.6086424470119027 ) ) ;
#16060 = CARTESIAN_POINT ( 'NONE',  ( -100.7409079118262980, -292.0089555227912115, -310.8371557114539883 ) ) ;
#16061 = CARTESIAN_POINT ( 'NONE',  ( 82.17387051439972367, -297.5899665652531212, -194.8765235847432109 ) ) ;
#16062 = LINE ( 'NONE', #2779, #64023 ) ;
#16063 = CARTESIAN_POINT ( 'NONE',  ( -36.23581135676069920, -299.9860413745942083, -194.8007515470732187 ) ) ;
#16064 = CARTESIAN_POINT ( 'NONE',  ( 15.38283133894301891, -280.0178999546803880, -219.5666926775269303 ) ) ;
#16065 = CARTESIAN_POINT ( 'NONE',  ( 35.25312124887982890, -279.7946907519416300, -289.2534509245011805 ) ) ;
#16066 = CARTESIAN_POINT ( 'NONE',  ( 37.60607962888355615, -292.5363440170551712, -253.3613360465822382 ) ) ;
#16067 = CARTESIAN_POINT ( 'NONE',  ( -40.53238431738569147, -296.4112665006975931, -196.6174343441556118 ) ) ;
#16068 = CARTESIAN_POINT ( 'NONE',  ( -4.451425840511100240, -274.6952289539471508, -337.1550983218368742 ) ) ;
#16069 = CARTESIAN_POINT ( 'NONE',  ( -96.79757616207875515, -297.2665270595649076, -313.5826181306987905 ) ) ;
#16070 = CARTESIAN_POINT ( 'NONE',  ( -147.0026986695710320, 31.65052214425349675, 22.50000000000000000 ) ) ;
#16071 = CARTESIAN_POINT ( 'NONE',  ( -64.67224439009181935, -272.2769405454720300, -198.9912602122829810 ) ) ;
#16072 = CARTESIAN_POINT ( 'NONE',  ( -95.74712210801881440, -294.1293270918399685, -318.9898003738420016 ) ) ;
#16073 = CARTESIAN_POINT ( 'NONE',  ( 27.68719393287989305, -295.4442033218020356, -304.9173770732336379 ) ) ;
#16074 = EDGE_CURVE ( 'NONE', #23459, #55526, #38030, .T. ) ;
#16075 = LINE ( 'NONE', #30744, #38434 ) ;
#16076 = CARTESIAN_POINT ( 'NONE',  ( -5.461923765841955714, -295.4245150839213352, -336.2254089208943242 ) ) ;
#16077 = FACE_OUTER_BOUND ( 'NONE', #57601, .T. ) ;
#16079 = CARTESIAN_POINT ( 'NONE',  ( -107.9695772386578199, -296.3078622881507727, -288.8686819391106724 ) ) ;
#16078 = CARTESIAN_POINT ( 'NONE',  ( -102.6030942302557065, -283.0739400894740356, -232.5830511604771971 ) ) ;
#16080 = CARTESIAN_POINT ( 'NONE',  ( -110.2246821559504895, -284.2391628523432701, -295.2020304200150349 ) ) ;
#16081 = CARTESIAN_POINT ( 'NONE',  ( -60.76167112943635829, -285.2737026592313327, -342.2545956808456822 ) ) ;
#16082 = CARTESIAN_POINT ( 'NONE',  ( -95.79772248370970544, -284.8955784066761225, -220.1948713567610696 ) ) ;
#16083 = CARTESIAN_POINT ( 'NONE',  ( -58.14066155079859755, -289.7827586593165847, -198.4220689122026897 ) ) ;
#16084 = CARTESIAN_POINT ( 'NONE',  ( 21.27581636871891391, -273.6952119285918457, -317.1477375740089997 ) ) ;
#16085 = CARTESIAN_POINT ( 'NONE',  ( 154.7659666677267580, 19.56018909072085066, 12.94946946941272437 ) ) ;
#16086 = CARTESIAN_POINT ( 'NONE',  ( -25.04291726254466255, -284.8969545776492396, -197.8527026799237660 ) ) ;
#16087 = CARTESIAN_POINT ( 'NONE',  ( -97.05808429791169090, -288.8246426337437356, -318.5009133096664868 ) ) ;
#16088 = DIRECTION ( 'NONE',  ( 1.000000000000000000, 0.000000000000000000, 0.000000000000000000 ) ) ;
#16089 = CARTESIAN_POINT ( 'NONE',  ( -109.5662386839992166, -298.3509779018197037, -255.1326617795067762 ) ) ;
#16090 = CARTESIAN_POINT ( 'NONE',  ( -113.1791059691529284, -279.8544022416588746, -280.1223710940091678 ) ) ;
#16092 = CARTESIAN_POINT ( 'NONE',  ( 17.08140358048866148, -280.5225550356768167, -221.6762818470592151 ) ) ;
#16091 = CARTESIAN_POINT ( 'NONE',  ( -61.09747669634701595, -293.3790022065677476, -341.9283988016326816 ) ) ;
#16093 = CARTESIAN_POINT ( 'NONE',  ( -11.05521348601741671, -294.8856093736546313, -342.7918589543522785 ) ) ;
#16094 = CARTESIAN_POINT ( 'NONE',  ( -80.10275740121561228, -283.5585783044428467, -208.0018590886799643 ) ) ;
#16095 = EDGE_CURVE ( 'NONE', #35594, #57506, #9303, .T. ) ;
#16096 = CARTESIAN_POINT ( 'NONE',  ( -72.84204861055374636, -281.5820908615443159, -204.2804810407856166 ) ) ;
#16097 = CARTESIAN_POINT ( 'NONE',  ( -59.53141437658843671, -295.7647791016218548, -198.6647581677904952 ) ) ;
#16098 = VERTEX_POINT ( 'NONE', #52392 ) ;
#16099 = DIRECTION ( 'NONE',  ( 1.000000000000000000, -0.000000000000000000, -0.000000000000000000 ) ) ;
#16100 = CARTESIAN_POINT ( 'NONE',  ( -4.865155017680591776, -282.4618619047147945, -203.1515887103534510 ) ) ;
#16101 = CARTESIAN_POINT ( 'NONE',  ( -63.59695877118431895, -294.9113420021631100, -338.5957313310985910 ) ) ;
#16102 = DIRECTION ( 'NONE',  ( 0.000000000000000000, 1.000000000000000000, 0.000000000000000000 ) ) ;
#16103 = CARTESIAN_POINT ( 'NONE',  ( -114.2704648735229114, -276.0523547857348490, -270.3284710469133074 ) ) ;
#16104 = CARTESIAN_POINT ( 'NONE',  ( -81.14991594156447263, -272.6709884484788518, -207.1697987114992259 ) ) ;
#16105 = CARTESIAN_POINT ( 'NONE',  ( -69.01568047157188346, -291.4570071418833663, -204.5768126635960868 ) ) ;
#16106 = CARTESIAN_POINT ( 'NONE',  ( -66.36038006800242783, -281.1853093273176682, -202.6079648835188038 ) ) ;
#16107 = CARTESIAN_POINT ( 'NONE',  ( -83.70885577685095313, -275.0035149987531327, -212.9457255338397772 ) ) ;
#16108 = CARTESIAN_POINT ( 'NONE',  ( -38.69766541833456586, -284.6690149806497061, -346.5490551911209423 ) ) ;
#16109 = EDGE_CURVE ( 'NONE', #36642, #59451, #59215, .T. ) ;
#16110 = CARTESIAN_POINT ( 'NONE',  ( -94.23866423185275210, -277.9998722057171676, -223.9944706818797329 ) ) ;
#16111 = CARTESIAN_POINT ( 'NONE',  ( -41.95483215792304321, -279.1104285126171476, -345.2320561957508289 ) ) ;
#16112 = VERTEX_POINT ( 'NONE', #23977 ) ;
#16113 = CARTESIAN_POINT ( 'NONE',  ( -63.55509974514872340, -273.5530578305539393, -197.9604433654228046 ) ) ;
#16114 = CARTESIAN_POINT ( 'NONE',  ( -44.46181446769116974, -293.8816772640726640, -196.2105912024025258 ) ) ;
#16115 = FACE_OUTER_BOUND ( 'NONE', #976, .T. ) ;
#16116 = DIRECTION ( 'NONE',  ( -0.9693563597868444237, -0.2456588035076248677, 0.000000000000000000 ) ) ;
#16117 = CARTESIAN_POINT ( 'NONE',  ( -34.91826982551637570, -293.1616009775517000, -346.0871535881247496 ) ) ;
#16118 = CARTESIAN_POINT ( 'NONE',  ( -52.63537675050562825, -297.5176346686349689, -198.9076008994401548 ) ) ;
#16119 = FACE_OUTER_BOUND ( 'NONE', #93470, .T. ) ;
#16120 = CARTESIAN_POINT ( 'NONE',  ( -19.56723662603547709, -293.7967052494137192, -196.0991370707760382 ) ) ;
#16121 = CARTESIAN_POINT ( 'NONE',  ( -106.6662871844225293, -275.4805209788417528, -237.0123917617630980 ) ) ;
#16122 = CARTESIAN_POINT ( 'NONE',  ( 21.77363748050969150, -288.9218133094374252, -224.4764223860316008 ) ) ;
#16123 = CARTESIAN_POINT ( 'NONE',  ( 25.51069872189556165, -274.1016340840220664, -311.0719376254648978 ) ) ;
#16124 = CARTESIAN_POINT ( 'NONE',  ( 36.26187065873975257, -277.3272472470691241, -259.1477087954085050 ) ) ;
#16125 = CARTESIAN_POINT ( 'NONE',  ( -4.936319404313901593, -292.7019694950465123, -337.3916552285003263 ) ) ;
#16126 = CARTESIAN_POINT ( 'NONE',  ( -76.86865594529287193, -281.3896297829937794, -205.6635001278857544 ) ) ;
#16127 = ORIENTED_EDGE ( 'NONE', *, *, #65170, .F. ) ;
#16128 = CARTESIAN_POINT ( 'NONE',  ( -10.97209389845760619, -282.3655270742172547, -338.5082610651087975 ) ) ;
#16129 = CARTESIAN_POINT ( 'NONE',  ( -107.2885073356802792, -279.2270999094243962, -301.9376500331092643 ) ) ;
#16130 = CARTESIAN_POINT ( 'NONE',  ( 1.877597072067028749, -281.3345076314728317, -336.1627550862185672 ) ) ;
#16131 = CARTESIAN_POINT ( 'NONE',  ( -54.06826681389222955, -278.2029686009424836, -345.3358283903361325 ) ) ;
#16132 = CARTESIAN_POINT ( 'NONE',  ( 38.05380001206331997, -277.2248352481663005, -282.4502466002586516 ) ) ;
#16133 = CARTESIAN_POINT ( 'NONE',  ( 17.36665895637874613, -283.4090924074130839, -226.6919474004047572 ) ) ;
#16134 = ORIENTED_EDGE ( 'NONE', *, *, #58215, .F. ) ;
#16135 = CARTESIAN_POINT ( 'NONE',  ( -104.3298507207468475, -298.9992136834750909, -236.5172525613756704 ) ) ;
#16136 = CARTESIAN_POINT ( 'NONE',  ( -109.5837590857027806, -291.7993450544401526, -257.6085902228123814 ) ) ;
#16137 = CARTESIAN_POINT ( 'NONE',  ( -111.2467396229617691, -276.7121135475974256, -259.5203760085709064 ) ) ;
#16138 = CARTESIAN_POINT ( 'NONE',  ( -105.5933421259349956, -291.8762641739260175, -303.8825561424387161 ) ) ;
#16139 = CARTESIAN_POINT ( 'NONE',  ( -67.83615987349411114, -290.9896026955631214, -203.9095704579743540 ) ) ;
#16140 = CARTESIAN_POINT ( 'NONE',  ( 38.23091782796835503, -286.8791606111798274, -255.9282970985375414 ) ) ;
#16141 = CARTESIAN_POINT ( 'NONE',  ( 197.5379522065468052, 275.5000000000000568, -11.97918851819043873 ) ) ;
#16142 = CARTESIAN_POINT ( 'NONE',  ( -111.1194504936760552, -282.9090520012756542, -273.6537263002545615 ) ) ;
#16143 = CARTESIAN_POINT ( 'NONE',  ( -111.2042228462525912, -292.5089467253582711, -262.9319042489740355 ) ) ;
#16144 = CARTESIAN_POINT ( 'NONE',  ( -65.33886147741188211, -284.1594353396785664, -202.1388762867762807 ) ) ;
#16145 = CARTESIAN_POINT ( 'NONE',  ( 34.97368775861869494, -283.0399653335376229, -283.5362312299162681 ) ) ;
#16146 = CARTESIAN_POINT ( 'NONE',  ( -73.05374079550901456, -290.4549140917231398, -338.3277993792888196 ) ) ;
#16147 = CARTESIAN_POINT ( 'NONE',  ( -97.69613262048412139, -278.4721298600538262, -311.5355143986197390 ) ) ;
#16148 = CARTESIAN_POINT ( 'NONE',  ( -58.81261158464429428, -290.5753408759996432, -196.8287531433772983 ) ) ;
#16149 = CARTESIAN_POINT ( 'NONE',  ( 39.47839147570288532, -288.3338913960093919, -268.6781604700288426 ) ) ;
#16150 = CARTESIAN_POINT ( 'NONE',  ( 35.01673811254666191, -288.3767458938384607, -296.6654093139031829 ) ) ;
#16151 = CARTESIAN_POINT ( 'NONE',  ( -10.75194963637617995, -286.5754825251138413, -202.3624088034963791 ) ) ;
#16152 = ORIENTED_EDGE ( 'NONE', *, *, #87773, .F. ) ;
#16153 = AXIS2_PLACEMENT_3D ( 'NONE', #89926, #25082, #53956 ) ;
#16154 = CARTESIAN_POINT ( 'NONE',  ( 113.5000000000000568, -298.0521521680024080, -397.9547385950631337 ) ) ;
#16155 = CARTESIAN_POINT ( 'NONE',  ( -40.60334466124434982, -293.8719852272722619, -194.6535824823055236 ) ) ;
#16156 = CARTESIAN_POINT ( 'NONE',  ( -110.3343596821110850, -294.9466120360130503, -293.3259483935088383 ) ) ;
#16157 = CARTESIAN_POINT ( 'NONE',  ( -70.57023658465119809, -276.5603056892726954, -335.6242225191335251 ) ) ;
#16158 = CARTESIAN_POINT ( 'NONE',  ( -36.88926682509398347, -297.4062679019811526, -193.4630985363918114 ) ) ;
#16159 = CARTESIAN_POINT ( 'NONE',  ( 16.65409918822919266, -292.7461211028290791, -320.5125028983997026 ) ) ;
#16160 = CARTESIAN_POINT ( 'NONE',  ( -110.2705752990698471, -294.9562527459866033, -257.7376010002607245 ) ) ;
#16161 = CARTESIAN_POINT ( 'NONE',  ( -75.19748937292605717, -292.7409352337436985, -207.4203806474900489 ) ) ;
#16162 = CARTESIAN_POINT ( 'NONE',  ( 35.84231423949732687, -294.5651007754024704, -265.2812828875474906 ) ) ;
#16163 = CARTESIAN_POINT ( 'NONE',  ( 209.2250871165752244, 35.77521060175700995, 15.12480380946217728 ) ) ;
#16164 = CARTESIAN_POINT ( 'NONE',  ( 5.546545866062435159, -292.4731416880759411, -332.1547990540379942 ) ) ;
#16165 = CARTESIAN_POINT ( 'NONE',  ( 194.5881128153456814, -26.00396092263537895, 22.08578643762690419 ) ) ;
#16166 = CARTESIAN_POINT ( 'NONE',  ( -92.58133364584938363, -290.8093285287337721, -318.5200577232094474 ) ) ;
#16167 = CARTESIAN_POINT ( 'NONE',  ( -45.08875949535130445, -295.4861018686797252, -343.0206345511993504 ) ) ;
#16168 = CARTESIAN_POINT ( 'NONE',  ( -3.441966035370155996, -278.5868235652208682, -337.6749259665084537 ) ) ;
#16169 = CARTESIAN_POINT ( 'NONE',  ( -59.14547265703046719, -278.4605304936694665, -197.0269937622997816 ) ) ;
#16170 = CARTESIAN_POINT ( 'NONE',  ( -104.1368711729147947, -272.3974756500696799, -232.1528593825767643 ) ) ;
#16171 = CARTESIAN_POINT ( 'NONE',  ( 35.75279077991758925, -279.4488606623720557, -256.2045091629522062 ) ) ;
#16172 = CARTESIAN_POINT ( 'NONE',  ( -112.0138065052718304, -276.7593384483882915, -285.6084693395042109 ) ) ;
#16173 = EDGE_CURVE ( 'NONE', #25647, #60166, #23043, .T. ) ;
#16174 = CARTESIAN_POINT ( 'NONE',  ( -104.9136139498326656, -271.5169231970756414, -241.0873924013882004 ) ) ;
#16175 = DIRECTION ( 'NONE',  ( -1.000000000000000000, -0.000000000000000000, -0.000000000000000000 ) ) ;
#16176 = CARTESIAN_POINT ( 'NONE',  ( -24.58679142903325499, -274.8705162094104821, -198.3288709757293873 ) ) ;
#16177 = DIRECTION ( 'NONE',  ( -1.000000000000000000, 0.000000000000000000, 0.000000000000000000 ) ) ;
#16178 = CARTESIAN_POINT ( 'NONE',  ( -103.7193022270699316, -288.1010246806885675, -306.0321249717113119 ) ) ;
#16179 = CARTESIAN_POINT ( 'NONE',  ( -93.59279552133443758, -289.8344171345688096, -323.0194624958240865 ) ) ;
#16180 = CARTESIAN_POINT ( 'NONE',  ( 29.60560757263339937, -277.1013848020385808, -236.1838387586753925 ) ) ;
#16181 = CARTESIAN_POINT ( 'NONE',  ( -72.50447677735419916, -295.5854839531740481, -204.2889578663002226 ) ) ;
#16182 = CARTESIAN_POINT ( 'NONE',  ( -97.05338876062029385, -283.0991579572161072, -318.7416268297466786 ) ) ;
#16183 = FACE_OUTER_BOUND ( 'NONE', #49908, .T. ) ;
#16184 = CARTESIAN_POINT ( 'NONE',  ( -39.31963172620219638, -281.0767920152613897, -345.3475872961309960 ) ) ;
#16185 = CARTESIAN_POINT ( 'NONE',  ( 175.2296996224750103, 21.00000000000000000, 0.000000000000000000 ) ) ;
#16186 = CARTESIAN_POINT ( 'NONE',  ( -44.32277655854829135, -290.7569513922284159, -197.2457026574006704 ) ) ;
#16187 = CARTESIAN_POINT ( 'NONE',  ( -16.80785697581064753, -284.4596247870989032, -198.9685542838419110 ) ) ;
#16188 = CARTESIAN_POINT ( 'NONE',  ( 143.6449502718966755, -26.00396092263537540, 21.50000000000000000 ) ) ;
#16189 = PLANE ( 'NONE',  #56384 ) ;
#16190 = CARTESIAN_POINT ( 'NONE',  ( 37.62112559894191577, -291.5216695801286733, -267.9998884703254589 ) ) ;
#16191 = CARTESIAN_POINT ( 'NONE',  ( -72.01218930523641859, -279.1186947887292149, -335.5244118700737204 ) ) ;
#16192 = CARTESIAN_POINT ( 'NONE',  ( 17.55250178850824838, -283.4942067149600575, -323.8657153245350173 ) ) ;
#16194 = CARTESIAN_POINT ( 'NONE',  ( -97.35594067751075897, -285.1314461345691598, -228.7783325186550769 ) ) ;
#16193 = CARTESIAN_POINT ( 'NONE',  ( -66.94844769653154515, -271.7469969881652219, -200.8431009058678001 ) ) ;
#16195 = CARTESIAN_POINT ( 'NONE',  ( 31.82173572921842464, -277.3114026359232298, -295.6448123121249409 ) ) ;
#16196 = CARTESIAN_POINT ( 'NONE',  ( 3.232133999101723276, -277.2942152897651908, -331.2410466198245445 ) ) ;
#16197 = EDGE_CURVE ( 'NONE', #62648, #6475, #75899, .T. ) ;
#16198 = ADVANCED_FACE ( 'NONE', ( #59989 ), #48651, .F. ) ;
#16199 = CARTESIAN_POINT ( 'NONE',  ( -111.9125248323765192, -286.4494415208300779, -278.3731558253541039 ) ) ;
#16200 = B_SPLINE_CURVE_WITH_KNOTS ( 'NONE', 3,
 ( #90920, #24697, #61172, #61627, #4783, #70141, #32738, #4319, #76296, #54975, #41204, #55457, #90460, #33663, #76759, #10471, #47383, #84308, #40736, #46454, #82455, #82907, #19460, #17603, #75815, #39337, #83851, #26086, #68255, #11421 ),
 .UNSPECIFIED., .F., .F.,
 ( 4, 2, 2, 2, 2, 2, 2, 2, 2, 2, 2, 2, 2, 2, 4 ),
 ( 0.006252914598272697050, 0.006643633568813113281, 0.007034352539353530380, 0.007815790480434363710, 0.008206509450974808564, 0.008597228421515255153, 0.008987947392055700008, 0.009378666362596146597, 0.009769385333136593186, 0.01016010430367703804, 0.01055082327421748463, 0.01094154224475792948, 0.01133226121529837607, 0.01172298018583882093, 0.01250441812691963604 ),
 .UNSPECIFIED. ) ;
#16201 = ORIENTED_EDGE ( 'NONE', *, *, #67721, .F. ) ;
#16202 = CARTESIAN_POINT ( 'NONE',  ( 201.0776230153480526, -142.7221692137691775, -8.778910157967986905 ) ) ;
#16203 = CARTESIAN_POINT ( 'NONE',  ( -98.27576076257273030, -295.7571164019763614, -317.4359547759470388 ) ) ;
#16204 = CARTESIAN_POINT ( 'NONE',  ( -37.30481570147205161, -288.0324695876779515, -195.7036035952458235 ) ) ;
#16205 = CARTESIAN_POINT ( 'NONE',  ( 223.4306832106270804, -141.7221692137691775, 22.50000000000000000 ) ) ;
#16206 = CARTESIAN_POINT ( 'NONE',  ( -72.02372285203398405, -289.1237833571631768, -198.2697987213421698 ) ) ;
#16207 = CARTESIAN_POINT ( 'NONE',  ( -114.0758385261368204, -277.4570555674865773, -271.5896671702783465 ) ) ;
#16208 = CARTESIAN_POINT ( 'NONE',  ( -83.76268854326333724, -289.8271663497507689, -209.8667194249643728 ) ) ;
#16209 = CARTESIAN_POINT ( 'NONE',  ( -44.10711869349033520, -287.4851838300175473, -196.9789889320526299 ) ) ;
#16210 = CARTESIAN_POINT ( 'NONE',  ( -96.43415456614472703, -280.9299376153308003, -225.7748866482500603 ) ) ;
#16211 = CARTESIAN_POINT ( 'NONE',  ( 32.33507018767577534, -289.3811310049298982, -301.7259704401269573 ) ) ;
#16212 = CARTESIAN_POINT ( 'NONE',  ( 36.01621212100327796, -283.3511463465368365, -254.6917799651908751 ) ) ;
#16213 = CARTESIAN_POINT ( 'NONE',  ( 24.36893000848480284, -276.3314503300293836, -316.4132420668246368 ) ) ;
#16214 = CARTESIAN_POINT ( 'NONE',  ( -100.8225511167938748, -271.0855457991739286, -230.7352428114152190 ) ) ;
#16215 = CARTESIAN_POINT ( 'NONE',  ( -99.42660992820020738, -278.9906119139737939, -224.7925820697931556 ) ) ;
#16216 = CARTESIAN_POINT ( 'NONE',  ( -40.60509971707764265, -299.9309800837078228, -195.9798848392087791 ) ) ;
#16217 = CARTESIAN_POINT ( 'NONE',  ( 164.7123623445222904, 2.999999999999999112, 9.000000000000001776 ) ) ;
#16218 = CARTESIAN_POINT ( 'NONE',  ( 21.27581636871892101, -277.4090924074130839, -223.5744983911110353 ) ) ;
#16219 = CARTESIAN_POINT ( 'NONE',  ( 4.326475101195915940, -272.8451434100428514, -206.7554865447235102 ) ) ;
#16220 = CARTESIAN_POINT ( 'NONE',  ( 198.1329898669367253, 69.92583464099142532, -8.330337636095675791 ) ) ;
#16221 = CARTESIAN_POINT ( 'NONE',  ( -66.08814367457807748, -279.1731653676085330, -203.1787966177181772 ) ) ;
#16222 = CARTESIAN_POINT ( 'NONE',  ( 11.52055205328863252, -275.9173801307104554, -211.2965318148598044 ) ) ;
#16223 = CARTESIAN_POINT ( 'NONE',  ( 30.86258623263275069, -281.0663989921815187, -305.5888845073152424 ) ) ;
#16224 = CARTESIAN_POINT ( 'NONE',  ( -70.40525860662425828, -291.2542283555349059, -336.5928013246248156 ) ) ;
#16225 = CARTESIAN_POINT ( 'NONE',  ( -91.16036202305879499, -298.8240437947548571, -216.2662070974320727 ) ) ;
#16226 = CARTESIAN_POINT ( 'NONE',  ( -75.59499989865737746, -298.7590619768773763, -203.9323675152541568 ) ) ;
#16227 = CARTESIAN_POINT ( 'NONE',  ( -67.32135804686434710, -293.6582444485196106, -201.7954666681785625 ) ) ;
#16228 = CARTESIAN_POINT ( 'NONE',  ( 36.37741274987858020, -279.3864321965698423, -257.4956283005761293 ) ) ;
#16229 = CARTESIAN_POINT ( 'NONE',  ( 35.74345521235762391, -283.2885479010608378, -256.1563880442284926 ) ) ;
#16230 = CARTESIAN_POINT ( 'NONE',  ( -90.39384897476784886, -271.3166666430514056, -217.8509636826366886 ) ) ;
#16231 = CARTESIAN_POINT ( 'NONE',  ( -85.02828893770877983, -287.0065637658222499, -210.9268714483122551 ) ) ;
#16232 = CARTESIAN_POINT ( 'NONE',  ( -8.107814036573927297, -287.5804713050972055, -337.6433954937228918 ) ) ;
#16233 = CARTESIAN_POINT ( 'NONE',  ( 186.7139198192865592, 262.6718262295162276, -153.2124302575201682 ) ) ;
#16234 = VERTEX_POINT ( 'NONE', #2680 ) ;
#16235 = CARTESIAN_POINT ( 'NONE',  ( 2.854613614107779807, -287.0990706900261102, -335.4067355553528387 ) ) ;
#16236 = CARTESIAN_POINT ( 'NONE',  ( -68.77092333638108812, -289.1438262966360639, -336.2723568982559641 ) ) ;
#16237 = ORIENTED_EDGE ( 'NONE', *, *, #26328, .F. ) ;
#16238 = CARTESIAN_POINT ( 'NONE',  ( -106.4067259682112194, -286.0612920057370161, -237.0217311469999117 ) ) ;
#16239 = CARTESIAN_POINT ( 'NONE',  ( 27.87826845832727329, -275.4398567214372520, -237.5214592713778927 ) ) ;
#16240 = CARTESIAN_POINT ( 'NONE',  ( 25.45361613320665128, -293.0572667345268769, -314.4094868430897236 ) ) ;
#16241 = CARTESIAN_POINT ( 'NONE',  ( 39.51818539664289176, -282.2339068755487119, -272.7840879383237507 ) ) ;
#16242 = CARTESIAN_POINT ( 'NONE',  ( 39.01653097125057457, -283.0666411534982103, -269.9148259015853455 ) ) ;
#16243 = CARTESIAN_POINT ( 'NONE',  ( 9.199394841453944593, -282.7656273979195021, -331.6772722200328758 ) ) ;
#16244 = CARTESIAN_POINT ( 'NONE',  ( 18.84965566818484817, -281.2240649149354113, -223.7089026532827063 ) ) ;
#16245 = CARTESIAN_POINT ( 'NONE',  ( -112.3417001280813707, -270.0523547857347353, -270.3292895737510548 ) ) ;
#16246 = CARTESIAN_POINT ( 'NONE',  ( 190.2525334769776180, 271.2110853878423882, -139.6778337214551300 ) ) ;
#16247 = ORIENTED_EDGE ( 'NONE', *, *, #15163, .F. ) ;
#16248 = CARTESIAN_POINT ( 'NONE',  ( -6.735091568210989976, -278.6495834679942050, -338.6492131537686419 ) ) ;
#16249 = CARTESIAN_POINT ( 'NONE',  ( -49.07113805792994299, -154.4069795088023511, -364.5415411693985561 ) ) ;
#16250 = CARTESIAN_POINT ( 'NONE',  ( -65.60447484896799608, -297.0210948122020227, -202.9437001037192090 ) ) ;
#16251 = CARTESIAN_POINT ( 'NONE',  ( 34.40771299638171143, -292.7059853519118064, -242.4370930409610594 ) ) ;
#16252 = CARTESIAN_POINT ( 'NONE',  ( -54.76359932913371864, -169.9329552033845516, -360.8268486737666194 ) ) ;
#16254 = CARTESIAN_POINT ( 'NONE',  ( -34.56812770239302779, -287.4167306199391305, -344.1591099195398442 ) ) ;
#16253 = CARTESIAN_POINT ( 'NONE',  ( -57.21880872032244980, -296.3754306481411049, -196.5261409564130304 ) ) ;
#16255 = CARTESIAN_POINT ( 'NONE',  ( -31.48160652108500912, -296.8379384946323967, -344.4156246562875481 ) ) ;
#16256 = CARTESIAN_POINT ( 'NONE',  ( -60.14745262134368176, -287.0654195245782603, -200.4959540560353446 ) ) ;
#16257 = ORIENTED_EDGE ( 'NONE', *, *, #63294, .T. ) ;
#16258 = CARTESIAN_POINT ( 'NONE',  ( 11.05927667204722020, -295.3424024451439323, -330.0128941925360664 ) ) ;
#16259 = CARTESIAN_POINT ( 'NONE',  ( -92.60156605940046859, -284.3638789883883078, -318.1748787456050991 ) ) ;
#16260 = CARTESIAN_POINT ( 'NONE',  ( -23.43396497331633910, -297.0175644046451566, -193.7609613474342041 ) ) ;
#16261 = CARTESIAN_POINT ( 'NONE',  ( -22.23556206878428299, -293.0435875689218506, -194.9679170069993859 ) ) ;
#16262 = CARTESIAN_POINT ( 'NONE',  ( 26.46421620400243668, -294.6113789652583250, -313.3533491906871404 ) ) ;
#16263 = CARTESIAN_POINT ( 'NONE',  ( -99.71270950028346647, -291.2412504672337263, -232.4288468353344115 ) ) ;
#16264 = VERTEX_POINT ( 'NONE', #72781 ) ;
#16265 = FACE_BOUND ( 'NONE', #80655, .T. ) ;
#16266 = CARTESIAN_POINT ( 'NONE',  ( -112.1228431768507505, -274.6147742318615883, -259.1824232462478790 ) ) ;
#16267 = CARTESIAN_POINT ( 'NONE',  ( 37.25179132366939427, -274.1273084720768907, -252.8735815603266417 ) ) ;
#16268 = ADVANCED_FACE ( 'NONE', ( #2218 ), #22578, .F. ) ;
#16269 = VERTEX_POINT ( 'NONE', #74646 ) ;
#16270 = CARTESIAN_POINT ( 'NONE',  ( 16.90738480389926579, -275.8124252127422551, -324.9933978776310823 ) ) ;
#16271 = CARTESIAN_POINT ( 'NONE',  ( -44.61846469467364784, -296.4384195630203180, -196.9770698065047725 ) ) ;
#16272 = CARTESIAN_POINT ( 'NONE',  ( -110.1025740669333999, -280.6043674298349515, -255.5757484245055764 ) ) ;
#16273 = CARTESIAN_POINT ( 'NONE',  ( -54.25804351974434070, -275.4111532736019399, -342.6962504152160705 ) ) ;
#16274 = CARTESIAN_POINT ( 'NONE',  ( -107.8450367566909023, -298.0256707143407198, -249.9549907261361170 ) ) ;
#16275 = CARTESIAN_POINT ( 'NONE',  ( -108.7670278209491102, -273.7061770371675493, -254.1799247962115942 ) ) ;
#16276 = CARTESIAN_POINT ( 'NONE',  ( -89.48402620175262712, -275.0901107349373547, -215.0158144447745485 ) ) ;
#16277 = CARTESIAN_POINT ( 'NONE',  ( -43.87448814499236249, -271.9902098740429892, -195.2374532410689483 ) ) ;
#16278 = CARTESIAN_POINT ( 'NONE',  ( -95.68067244368005220, -296.5853736950767825, -314.4323543006391901 ) ) ;
#16279 = CARTESIAN_POINT ( 'NONE',  ( -19.91516919216364556, -290.8551404308154247, -198.8123333606396557 ) ) ;
#16280 = DIRECTION ( 'NONE',  ( 0.000000000000000000, 1.000000000000000000, -0.000000000000000000 ) ) ;
#16281 = CARTESIAN_POINT ( 'NONE',  ( -38.53771001915254857, -277.5591169839955796, -347.2902832181782173 ) ) ;
#16282 = CARTESIAN_POINT ( 'NONE',  ( 32.06115075511849710, -275.4165693455886412, -247.5657063917959704 ) ) ;
#16283 = CARTESIAN_POINT ( 'NONE',  ( -87.41445348585385489, -284.0558691444924193, -212.4462236600289771 ) ) ;
#16284 = CARTESIAN_POINT ( 'NONE',  ( -100.0835885964505110, -297.9936164148354010, -311.8494529010843053 ) ) ;
#16285 = CARTESIAN_POINT ( 'NONE',  ( 208.8440659120965108, 36.55262022383305975, 14.73366904486404572 ) ) ;
#16286 = CARTESIAN_POINT ( 'NONE',  ( -85.82552796069502676, -284.5577152500976013, -215.5036335218603369 ) ) ;
#16287 = CARTESIAN_POINT ( 'NONE',  ( -110.4423378051600508, -282.3270707865679015, -287.9178278497233805 ) ) ;
#16288 = CARTESIAN_POINT ( 'NONE',  ( -100.0453493371967397, -276.2553354315428464, -309.7789801721383469 ) ) ;
#16289 = CARTESIAN_POINT ( 'NONE',  ( -83.38948806981899509, -276.2719699245692482, -327.8285966362729482 ) ) ;
#16290 = CARTESIAN_POINT ( 'NONE',  ( -81.50644578307097277, -281.4518903907718368, -209.6801187859854281 ) ) ;
#16291 = CARTESIAN_POINT ( 'NONE',  ( 22.59627237185681992, -276.1688468478930645, -227.9770027233890914 ) ) ;
#16292 = CARTESIAN_POINT ( 'NONE',  ( 17.06571399127465583, -89.54582641780471874, -21.50000000000000000 ) ) ;
#16293 = CARTESIAN_POINT ( 'NONE',  ( -107.3345166760472438, -271.3413186390429246, -240.1039143176219000 ) ) ;
#16294 = CARTESIAN_POINT ( 'NONE',  ( -100.3682369741816416, -281.1044126406736723, -229.3073459555960767 ) ) ;
#16295 = DIRECTION ( 'NONE',  ( -1.000000000000000000, 0.000000000000000000, 0.000000000000000000 ) ) ;
#16296 = CARTESIAN_POINT ( 'NONE',  ( 4.364098886497129293, -288.5295649036525560, -207.2913468105184904 ) ) ;
#16297 = SURFACE_SIDE_STYLE ('',( #9168 ) ) ;
#16298 = CARTESIAN_POINT ( 'NONE',  ( -79.68695810032636473, -287.6238753389943099, -332.3254821489668984 ) ) ;
#16299 = DIRECTION ( 'NONE',  ( -0.3994899938747897283, 0.000000000000000000, 0.9167375550253848981 ) ) ;
#16300 = CARTESIAN_POINT ( 'NONE',  ( -88.39095327756177767, -296.1125388482879544, -217.5539986676623414 ) ) ;
#16301 = CARTESIAN_POINT ( 'NONE',  ( -111.5724348540797735, -288.6811625316134950, -271.1756727572679324 ) ) ;
#16302 = CARTESIAN_POINT ( 'NONE',  ( -47.20788896421541381, -156.8319029772612225, -362.3615984655540387 ) ) ;
#16303 = CARTESIAN_POINT ( 'NONE',  ( 200.4816938276917995, 61.72811464988816965, -9.999999999999998224 ) ) ;
#16304 = CARTESIAN_POINT ( 'NONE',  ( 38.88616731575952912, -285.9754619152517421, -265.8785973540325926 ) ) ;
#16305 = CARTESIAN_POINT ( 'NONE',  ( -59.16547274837295589, -284.9393466231269940, -340.9142227803303626 ) ) ;
#16306 = CARTESIAN_POINT ( 'NONE',  ( -109.2727562147464937, -282.4793054143922291, -294.8539165807092672 ) ) ;
#16307 = CARTESIAN_POINT ( 'NONE',  ( -91.67315886739584130, -291.2500997714784035, -221.5869846503155713 ) ) ;
#16308 = CARTESIAN_POINT ( 'NONE',  ( 18.39906502073738537, -282.2984139532649692, -222.2965724808200321 ) ) ;
#16309 = CARTESIAN_POINT ( 'NONE',  ( 33.91534250338784062, -282.1366924023305387, -253.7769205953290736 ) ) ;
#16310 = CARTESIAN_POINT ( 'NONE',  ( -110.9530855807429361, -292.3260695792760089, -286.4785228289846941 ) ) ;
#16311 = CARTESIAN_POINT ( 'NONE',  ( -54.59722990014531518, -298.0029883143106986, -195.3194848928578438 ) ) ;
#16312 = CARTESIAN_POINT ( 'NONE',  ( -38.91516943878473711, -287.1515998151572262, -345.9047371424738913 ) ) ;
#16313 = CARTESIAN_POINT ( 'NONE',  ( 22.64100153086099709, -276.1994314979034471, -318.6631865093805800 ) ) ;
#16314 = CARTESIAN_POINT ( 'NONE',  ( -64.69735070395229570, -293.6731113546075562, -200.8957466590317154 ) ) ;
#16315 = CARTESIAN_POINT ( 'NONE',  ( 189.9243309297870610, 275.5000000000000568, 20.22542485937349355 ) ) ;
#16316 = CARTESIAN_POINT ( 'NONE',  ( 31.95455697924148097, -289.6233781216988064, -236.9535640164627637 ) ) ;
#16317 = CARTESIAN_POINT ( 'NONE',  ( -70.77876011418413782, -275.4920321172583613, -337.6811852012679651 ) ) ;
#16318 = CARTESIAN_POINT ( 'NONE',  ( -57.23711263161519724, -285.8906705383787994, 47.50000000000000000 ) ) ;
#16319 = CARTESIAN_POINT ( 'NONE',  ( -97.58878990773281714, -295.5816866356868218, -223.6846435349226283 ) ) ;
#16320 = CARTESIAN_POINT ( 'NONE',  ( -96.35875916494275373, -272.5049752317430602, -227.1391175805158014 ) ) ;
#16321 = CARTESIAN_POINT ( 'NONE',  ( -104.6733955762617825, -291.6713406214026350, -300.4395371104528749 ) ) ;
#16322 = PRODUCT_DEFINITION_SHAPE ( 'NONE', 'NONE',  #9377 ) ;
#16323 = CARTESIAN_POINT ( 'NONE',  ( -34.86128085730018711, -293.0253279964703097, -197.1678398149136910 ) ) ;
#16325 = EDGE_CURVE ( 'NONE', #71428, #12480, #67085, .T. ) ;
#16324 = CARTESIAN_POINT ( 'NONE',  ( -86.41455260513905046, -287.1202765448499008, -214.8865596164082206 ) ) ;
#16326 = CARTESIAN_POINT ( 'NONE',  ( -2.342030346994991685, -293.9312962688777020, -202.4227520566249723 ) ) ;
#16327 = CARTESIAN_POINT ( 'NONE',  ( 20.92392625531129369, -294.1942918371789801, -220.7587026231051652 ) ) ;
#16328 = CARTESIAN_POINT ( 'NONE',  ( 35.29555480958364200, -293.2831422041878113, -262.6040241040332717 ) ) ;
#16329 = CARTESIAN_POINT ( 'NONE',  ( 37.11265630975704255, -289.6682648502039683, -279.3915916932880918 ) ) ;
#16330 = CARTESIAN_POINT ( 'NONE',  ( 38.87156924947326786, -281.8561386452170154, -281.3400785568035758 ) ) ;
#16331 = CARTESIAN_POINT ( 'NONE',  ( -34.09893422739740743, -296.1722966420492753, -194.8021611526462777 ) ) ;
#16332 = CARTESIAN_POINT ( 'NONE',  ( -113.9040879143121003, -284.2829502187655635, -278.5587262293210529 ) ) ;
#16333 = CARTESIAN_POINT ( 'NONE',  ( -0.6400002919494620635, -278.5422975026340282, -335.4183253151110193 ) ) ;
#16334 = EDGE_CURVE ( 'NONE', #22603, #68073, #41056, .T. ) ;
#16335 = CARTESIAN_POINT ( 'NONE',  ( -44.04544713944608958, -284.7604256844923043, -197.2708294291886943 ) ) ;
#16336 = CARTESIAN_POINT ( 'NONE',  ( 35.86699938998306436, -285.7619569205180028, -286.7134317703620923 ) ) ;
#16337 = CARTESIAN_POINT ( 'NONE',  ( -61.62888077925511965, -277.8796278114597271, -198.5392395433031254 ) ) ;
#16338 = CARTESIAN_POINT ( 'NONE',  ( -91.56268290671289378, -284.7612444521975021, -221.3166591200748883 ) ) ;
#16339 = CARTESIAN_POINT ( 'NONE',  ( -1.335711987239448284, -281.7240120381648012, -202.7476759949971665 ) ) ;
#16340 = CARTESIAN_POINT ( 'NONE',  ( -95.28858787518115037, -288.9282944163298339, -320.7096871167536278 ) ) ;
#16341 = CARTESIAN_POINT ( 'NONE',  ( -17.93349189183457071, -296.5586122712506381, -341.7844717555098555 ) ) ;
#16342 = CARTESIAN_POINT ( 'NONE',  ( -104.2631767810817252, -279.6757331693218589, -306.8022537521929962 ) ) ;
#16343 = CARTESIAN_POINT ( 'NONE',  ( -5.474815611269156612, -277.9567955228624214, -339.9154129302462479 ) ) ;
#16344 = CARTESIAN_POINT ( 'NONE',  ( -99.17622246392538443, -277.8485398082911502, -309.2562126029421847 ) ) ;
#16345 = CARTESIAN_POINT ( 'NONE',  ( -39.23973409271948043, -300.0284663701080490, -195.5391343674373559 ) ) ;
#16346 = CARTESIAN_POINT ( 'NONE',  ( 18.26968700832773607, -284.8524379816008718, -220.2680141096455770 ) ) ;
#16347 = CARTESIAN_POINT ( 'NONE',  ( -62.48029895242832055, -290.9738467421628343, -342.3508475376461320 ) ) ;
#16348 = CARTESIAN_POINT ( 'NONE',  ( -67.43461775610808218, -294.3767146558628269, -337.2227883698180904 ) ) ;
#16349 = ORIENTED_EDGE ( 'NONE', *, *, #87626, .F. ) ;
#16350 = CARTESIAN_POINT ( 'NONE',  ( -13.00519557605837306, -294.3938750924319834, -339.2607555079485451 ) ) ;
#16351 = CARTESIAN_POINT ( 'NONE',  ( -108.5064889487205875, -291.2675865707088292, -298.9454728142289355 ) ) ;
#16352 = CARTESIAN_POINT ( 'NONE',  ( -110.3816463245337332, -279.1639205000208790, -273.3709232058374710 ) ) ;
#16353 = CARTESIAN_POINT ( 'NONE',  ( -95.84057788451019633, -272.2832339461539277, -220.6347312962411138 ) ) ;
#16354 = CARTESIAN_POINT ( 'NONE',  ( 39.47532038430919243, -288.1466475145248296, -265.8161411878350577 ) ) ;
#16355 = CARTESIAN_POINT ( 'NONE',  ( -6.924373560759228496, -288.9970583541010569, -341.0897840895344189 ) ) ;
#16357 = CARTESIAN_POINT ( 'NONE',  ( -94.14116556072769981, -285.5344308015914976, -224.4511234692889161 ) ) ;
#16356 = AXIS2_PLACEMENT_3D ( 'NONE', #64007, #51607, #50705 ) ;
#16358 = CARTESIAN_POINT ( 'NONE',  ( 138.6539576904058606, 275.5000000000000568, -10.49999999999999822 ) ) ;
#16359 = CARTESIAN_POINT ( 'NONE',  ( 101.6393219532830017, 116.6108303934152559, -281.7644831123793665 ) ) ;
#16360 = CARTESIAN_POINT ( 'NONE',  ( -107.7063693688264578, -264.2743598394135915, -305.3713782035580948 ) ) ;
#16361 = CARTESIAN_POINT ( 'NONE',  ( 13.83699699917069914, -275.5094207430456663, -322.7130432056569020 ) ) ;
#16362 = CARTESIAN_POINT ( 'NONE',  ( -108.9055166516405677, -277.6820436282390574, -254.4025626319421747 ) ) ;
#16363 = CARTESIAN_POINT ( 'NONE',  ( -106.8223142620483515, -272.6438231725377932, -237.2221899521937303 ) ) ;
#16364 = CARTESIAN_POINT ( 'NONE',  ( 7.303344965765894869, -59.94948904379861432, -351.8522816994340587 ) ) ;
#16365 = CARTESIAN_POINT ( 'NONE',  ( -105.9108815046298275, -276.7966955586236963, -304.4150898271585106 ) ) ;
#16366 = CARTESIAN_POINT ( 'NONE',  ( -58.54675827214202855, -297.0826488908067518, -343.3838887269895963 ) ) ;
#16367 = CARTESIAN_POINT ( 'NONE',  ( -89.86491333119911928, -291.7777575810740132, -219.5743035867909327 ) ) ;
#16368 = CARTESIAN_POINT ( 'NONE',  ( -98.11256362570412648, -297.9842581717509233, -223.3179591224055400 ) ) ;
#16369 = CARTESIAN_POINT ( 'NONE',  ( -114.2400753769498323, -273.2393221503794507, -267.5057244075153449 ) ) ;
#16370 = CARTESIAN_POINT ( 'NONE',  ( -92.74579171207487605, -297.3956677056554554, -222.8088843005247384 ) ) ;
#16371 = ORIENTED_EDGE ( 'NONE', *, *, #47694, .T. ) ;
#16372 = CARTESIAN_POINT ( 'NONE',  ( 186.6539576904058890, 293.9636489450775230, 0.000000000000000000 ) ) ;
#16373 = CARTESIAN_POINT ( 'NONE',  ( -110.4282333791863238, -280.2271201044817985, -289.5866907514853210 ) ) ;
#16374 = CARTESIAN_POINT ( 'NONE',  ( -33.06843756209846674, -282.5073680209209783, -347.1939413502580010 ) ) ;
#16375 = B_SPLINE_CURVE_WITH_KNOTS ( 'NONE', 3,
 ( #17516, #46367, #75269, #10383, #39251, #68166, #17971, #61542 ),
 .UNSPECIFIED., .F., .F.,
 ( 4, 2, 2, 4 ),
 ( -4.472612521061044141E-06, 0.0004667749420422289872, 0.0007023987193238740313, 0.0009380224966055190211 ),
 .UNSPECIFIED. ) ;
#16376 = CARTESIAN_POINT ( 'NONE',  ( -102.4366631083095314, -280.0897522725324507, -236.5330680631435314 ) ) ;
#16377 = CARTESIAN_POINT ( 'NONE',  ( -73.59341721139551851, -279.2865404823958784, -337.1575573643905841 ) ) ;
#16378 = CARTESIAN_POINT ( 'NONE',  ( -3.771726761362441227, -272.9832408635779188, -204.7438661822537824 ) ) ;
#16379 = DIRECTION ( 'NONE',  ( 0.000000000000000000, 0.000000000000000000, 1.000000000000000000 ) ) ;
#16380 = CARTESIAN_POINT ( 'NONE',  ( 202.9738562182569694, 295.9636489450776367, -54.00000000004089173 ) ) ;
#16381 = CARTESIAN_POINT ( 'NONE',  ( -39.70335924761886304, -280.1883842873778576, -197.3868097963167543 ) ) ;
#16382 = CARTESIAN_POINT ( 'NONE',  ( 26.00564014826802861, -275.7795570244337569, -226.8490291283033855 ) ) ;
#16383 = CARTESIAN_POINT ( 'NONE',  ( 35.98450153386072969, -277.3492191523527026, -254.5439510777742100 ) ) ;
#16384 = CARTESIAN_POINT ( 'NONE',  ( 5.525604941588728281, -275.0586695930691121, -333.6145799252662414 ) ) ;
#16385 = ORIENTED_EDGE ( 'NONE', *, *, #44575, .F. ) ;
#16386 = CARTESIAN_POINT ( 'NONE',  ( 197.8233505269066370, 40.71551520756617037, 11.52974254711199364 ) ) ;
#16387 = CARTESIAN_POINT ( 'NONE',  ( 37.54518467823262995, -283.4190283348060007, -261.5174182045536782 ) ) ;
#16388 = CARTESIAN_POINT ( 'NONE',  ( -108.5823706773655033, -289.9692508772018300, -253.6521297974555011 ) ) ;
#16389 = CARTESIAN_POINT ( 'NONE',  ( -64.50341495112634504, -285.0553511108719817, -198.4056462179503910 ) ) ;
#16390 = CARTESIAN_POINT ( 'NONE',  ( -109.4171676094219237, -282.5724361356600980, -287.2421713934564309 ) ) ;
#16392 = CARTESIAN_POINT ( 'NONE',  ( 34.05796650964800421, -285.3582323336006539, -249.2589922416829040 ) ) ;
#16391 = CARTESIAN_POINT ( 'NONE',  ( 3.703943885315436280, -281.0629207807710372, -331.5016306394239223 ) ) ;
#16393 = CARTESIAN_POINT ( 'NONE',  ( -19.45255041007359154, -281.4923699012830980, -199.1249191239672598 ) ) ;
#16394 = CARTESIAN_POINT ( 'NONE',  ( -112.3407539019156900, -270.5881751857016297, -267.5427233129597084 ) ) ;
#16395 = CARTESIAN_POINT ( 'NONE',  ( 4.093413111189980746, -280.9041483905016889, -334.3732316026350873 ) ) ;
#16396 = CARTESIAN_POINT ( 'NONE',  ( 19.85925050791570712, -296.2235695291658999, -318.8693842686535049 ) ) ;
#16397 = CARTESIAN_POINT ( 'NONE',  ( -85.16567056974426464, -278.3843260780103037, -325.7161428276451716 ) ) ;
#16398 = CARTESIAN_POINT ( 'NONE',  ( -75.20577320404669308, -287.5493480377762694, -205.3678154330653740 ) ) ;
#16399 = CARTESIAN_POINT ( 'NONE',  ( 211.1232656141943949, 1.000000000000000000, -7.000000000000000888 ) ) ;
#16400 = CARTESIAN_POINT ( 'NONE',  ( -97.22235877942109994, -293.0991270643964413, -224.2574108282517216 ) ) ;
#16401 = CARTESIAN_POINT ( 'NONE',  ( 36.11849887208956034, -273.7461268645795371, -285.4806356723203180 ) ) ;
#16402 = CARTESIAN_POINT ( 'NONE',  ( -4.411556307768401020, -287.8263332408782844, -339.8000893942184462 ) ) ;
#16403 = CARTESIAN_POINT ( 'NONE',  ( 4.978900444463637776, -291.0342278158880163, -209.8384981112743333 ) ) ;
#16404 = CARTESIAN_POINT ( 'NONE',  ( -48.18343439339133027, -275.2947406849283425, -436.6688341897090595 ) ) ;
#16405 = CARTESIAN_POINT ( 'NONE',  ( -83.32829433658616836, -276.3820504910677869, -327.7544270997032640 ) ) ;
#16406 = CARTESIAN_POINT ( 'NONE',  ( -84.84740977078065782, -295.5289858015545406, -213.2495379198569765 ) ) ;
#16407 = CARTESIAN_POINT ( 'NONE',  ( -108.1967933285187229, -291.6090009648519867, -290.0625747719290075 ) ) ;
#16408 = DIRECTION ( 'NONE',  ( 1.000000000000000000, 0.000000000000000000, 0.000000000000000000 ) ) ;
#16409 = CARTESIAN_POINT ( 'NONE',  ( 175.2296996224750103, 15.00000000000000000, -15.00000000000000000 ) ) ;
#16410 = CARTESIAN_POINT ( 'NONE',  ( 25.13574854362705935, -292.6168872873300302, -314.1934580407796034 ) ) ;
#16411 = CARTESIAN_POINT ( 'NONE',  ( 33.03035483248249449, -288.8602792956152712, -248.0879171870295181 ) ) ;
#16412 = CARTESIAN_POINT ( 'NONE',  ( -112.8099185932005639, -288.6741950223462254, -279.6577538929920479 ) ) ;
#16413 = CARTESIAN_POINT ( 'NONE',  ( 35.34405464604518698, -289.1289174953184897, -281.9374564280342952 ) ) ;
#16414 = CARTESIAN_POINT ( 'NONE',  ( 157.7374095173865385, 14.19731191252289015, 10.00000000000000000 ) ) ;
#16415 = CARTESIAN_POINT ( 'NONE',  ( 34.68245126903803310, -288.5241268484272155, -283.2111507764303724 ) ) ;
#16416 = CARTESIAN_POINT ( 'NONE',  ( -67.54331271831900096, -297.4262855566577741, -339.3992914978597355 ) ) ;
#16417 = DIRECTION ( 'NONE',  ( 0.5000000000000032196, -0.8660254037844368202, 0.000000000000000000 ) ) ;
#16418 = AXIS2_PLACEMENT_3D ( 'NONE', #54705, #5002, #26307 ) ;
#16419 = CARTESIAN_POINT ( 'NONE',  ( -36.07792257828234028, -290.2417407020392375, -346.9666639826853611 ) ) ;
#16420 = CARTESIAN_POINT ( 'NONE',  ( -8.150367190403326134, -278.4526473076394950, -200.8757362775862418 ) ) ;
#16421 = CARTESIAN_POINT ( 'NONE',  ( -110.6452279083395780, -278.5879157333712328, -294.0345653154408865 ) ) ;
#16422 = CARTESIAN_POINT ( 'NONE',  ( -91.04037723865688747, -278.9815942206272439, -215.1307013957088259 ) ) ;
#16423 = CARTESIAN_POINT ( 'NONE',  ( -85.14714502091128168, -299.3686759873275491, -212.9657288373902873 ) ) ;
#16424 = CARTESIAN_POINT ( 'NONE',  ( -109.9589137582513132, -282.7929746611975474, -251.6063602795169345 ) ) ;
#16425 = CARTESIAN_POINT ( 'NONE',  ( -110.4232819666299292, -271.9154740667189003, -270.3530115452461473 ) ) ;
#16426 = CARTESIAN_POINT ( 'NONE',  ( -30.11901669293905570, -278.2839448855958722, -196.4269062987093548 ) ) ;
#16427 = CARTESIAN_POINT ( 'NONE',  ( -102.6873169358189699, -282.0604138633944444, -307.2760261478925372 ) ) ;
#16428 = CARTESIAN_POINT ( 'NONE',  ( -93.16753622582476169, -239.2408764263383887, -338.7286017555671265 ) ) ;
#16429 = CARTESIAN_POINT ( 'NONE',  ( 21.18627014143743281, -274.6969471670539633, -319.3221683276909744 ) ) ;
#16430 = CARTESIAN_POINT ( 'NONE',  ( -93.59926889214534640, -297.4019141856183523, -317.9810143550502630 ) ) ;
#16431 = CARTESIAN_POINT ( 'NONE',  ( 36.88913658842953680, -280.7146235228121895, -289.6296257362170081 ) ) ;
#16432 = CARTESIAN_POINT ( 'NONE',  ( -108.5248874333462226, -297.2663434550825627, -287.6291426650424796 ) ) ;
#16433 = CARTESIAN_POINT ( 'NONE',  ( 98.08324619808344380, -301.0295057411529456, -193.8246312193383289 ) ) ;
#16434 = CARTESIAN_POINT ( 'NONE',  ( -32.68544533119239048, -273.7791351950536978, -197.4760501967423920 ) ) ;
#16435 = CARTESIAN_POINT ( 'NONE',  ( 26.13315106313796221, -296.0905427342914891, -310.4079913028380702 ) ) ;
#16436 = CARTESIAN_POINT ( 'NONE',  ( 16.29766802551027993, -286.9554033782414990, -215.1178542431868550 ) ) ;
#16437 = CARTESIAN_POINT ( 'NONE',  ( -33.95488338532514661, -278.1742984622959511, -194.8770556098618272 ) ) ;
#16438 = CARTESIAN_POINT ( 'NONE',  ( -93.59424724881260715, -289.6677639854623862, -323.0179119074566074 ) ) ;
#16439 = CARTESIAN_POINT ( 'NONE',  ( -70.08840475228363687, -288.5532730354867113, -335.8812196734693885 ) ) ;
#16440 = CARTESIAN_POINT ( 'NONE',  ( -19.82841323456613125, -290.2769892473327786, -197.3811393204888702 ) ) ;
#16441 = VERTEX_POINT ( 'NONE', #52851 ) ;
#16442 = CARTESIAN_POINT ( 'NONE',  ( 199.1087447750284980, 64.61450673763174279, 10.46317447812566392 ) ) ;
#16443 = CARTESIAN_POINT ( 'NONE',  ( -108.4859596646804931, -290.2796859565485192, -253.6788072434247852 ) ) ;
#16444 = LINE ( 'NONE', #9318, #70127 ) ;
#16445 = CARTESIAN_POINT ( 'NONE',  ( 20.10267974825305970, -287.8007702458906465, -219.3615160238268231 ) ) ;
#16446 = CARTESIAN_POINT ( 'NONE',  ( 27.33386217378599881, -289.6233781216987495, -239.1787733560258573 ) ) ;
#16447 = CARTESIAN_POINT ( 'NONE',  ( -39.11445639276230679, -294.1326430087868857, -347.1053526129744569 ) ) ;
#16448 = CARTESIAN_POINT ( 'NONE',  ( -16.26153551749690607, -284.1005004927590107, -343.9614473518827253 ) ) ;
#16449 = CARTESIAN_POINT ( 'NONE',  ( -54.75428191579339199, -285.6554974714052832, -199.4159294301886405 ) ) ;
#16450 = CARTESIAN_POINT ( 'NONE',  ( 33.72330486385948234, -277.1130583691019638, -289.0963400157307319 ) ) ;
#16451 = CARTESIAN_POINT ( 'NONE',  ( 12.03735191561217910, -290.7623452765506613, -214.3139498349991641 ) ) ;
#16452 = CARTESIAN_POINT ( 'NONE',  ( 0.8320156675063714591, -273.3686904842926992, -207.6722200255360349 ) ) ;
#16453 = ORIENTED_EDGE ( 'NONE', *, *, #88447, .F. ) ;
#16454 = CARTESIAN_POINT ( 'NONE',  ( -114.4693268140674434, -273.6886850827510216, -284.2063049943780015 ) ) ;
#16455 = CARTESIAN_POINT ( 'NONE',  ( -3.970510213944848932, -288.4159819672958065, -203.8203193325850862 ) ) ;
#16456 = CARTESIAN_POINT ( 'NONE',  ( -87.27147981212841898, -298.4550727300872381, -212.0801943329517485 ) ) ;
#16457 = CARTESIAN_POINT ( 'NONE',  ( -46.74619177966876293, -286.5811557660247217, -197.8158011370420297 ) ) ;
#16458 = CARTESIAN_POINT ( 'NONE',  ( -103.4094153688019162, -277.0989664413390869, -309.5534556415274210 ) ) ;
#16459 = CARTESIAN_POINT ( 'NONE',  ( 21.22741372987772834, -293.5306383462622648, -220.5115782348033235 ) ) ;
#16460 = CARTESIAN_POINT ( 'NONE',  ( 38.36874495764529058, -285.7428343245421729, -274.3813994664754432 ) ) ;
#16461 = CARTESIAN_POINT ( 'NONE',  ( -30.58857772933567531, -295.3022437969684688, -347.0431864821463819 ) ) ;
#16462 = CARTESIAN_POINT ( 'NONE',  ( -96.78104473609431579, -291.4788819079716973, -227.8603537622912540 ) ) ;
#16463 = CYLINDRICAL_SURFACE ( 'NONE', #70181, 5.000000000000004441 ) ;
#16464 = DIRECTION ( 'NONE',  ( 1.000000000000000000, 0.000000000000000000, 0.000000000000000000 ) ) ;
#16465 = FACE_OUTER_BOUND ( 'NONE', #40184, .T. ) ;
#16466 = CARTESIAN_POINT ( 'NONE',  ( -93.42344398682644169, -286.7838328139675355, -218.5386496676854335 ) ) ;
#16467 = CARTESIAN_POINT ( 'NONE',  ( -19.05039376806006857, -271.7666405000204009, -190.3683826091709363 ) ) ;
#16468 = ORIENTED_EDGE ( 'NONE', *, *, #58978, .F. ) ;
#16469 = CARTESIAN_POINT ( 'NONE',  ( -90.97695450167036313, -282.7568732130407057, -320.3359672776710454 ) ) ;
#16470 = CARTESIAN_POINT ( 'NONE',  ( -97.67767780035426028, -278.8587599411739575, -222.5561591393152696 ) ) ;
#16471 = CARTESIAN_POINT ( 'NONE',  ( 28.47939625975084610, -284.0261726326654639, -305.9646528356768158 ) ) ;
#16472 = CARTESIAN_POINT ( 'NONE',  ( -20.11176207632858137, -109.5359415251419506, -361.5385522582666340 ) ) ;
#16473 = CARTESIAN_POINT ( 'NONE',  ( -35.92843382695069465, -281.6095211396936406, -346.7718374575732128 ) ) ;
#16474 = CARTESIAN_POINT ( 'NONE',  ( -3.834117088620982994, -284.5165667996649290, -203.6596286045912052 ) ) ;
#16475 = CARTESIAN_POINT ( 'NONE',  ( -34.17885669190302167, -275.9519435702060832, -194.6623603719603182 ) ) ;
#16476 = CARTESIAN_POINT ( 'NONE',  ( -93.66502482366470872, -297.7038360009959206, -223.8048774715532545 ) ) ;
#16477 = CARTESIAN_POINT ( 'NONE',  ( -34.29741842752031999, -293.6979010685468552, -343.7911923928651277 ) ) ;
#16478 = CARTESIAN_POINT ( 'NONE',  ( -114.2827779164243935, -279.1878616153184112, -271.6150246088460563 ) ) ;
#16479 = CARTESIAN_POINT ( 'NONE',  ( 20.02246176103595587, -276.1892285223080989, -315.5293710900151041 ) ) ;
#16480 = CARTESIAN_POINT ( 'NONE',  ( -93.92652099347314731, -274.3388772928976209, -218.5763831155590537 ) ) ;
#16481 = CARTESIAN_POINT ( 'NONE',  ( 8.047007390352755252, -275.3685137908680076, -332.2439903706264204 ) ) ;
#16482 = CARTESIAN_POINT ( 'NONE',  ( 202.9738562182569694, 295.9636489450776367, -54.00000000004089173 ) ) ;
#16483 = CARTESIAN_POINT ( 'NONE',  ( -39.18398525744974137, -275.0750839925356672, -345.3511302715397733 ) ) ;
#16484 = CARTESIAN_POINT ( 'NONE',  ( -36.26440983036671639, -296.4641969178428553, -346.7773000663530070 ) ) ;
#16485 = CARTESIAN_POINT ( 'NONE',  ( 150.4957602436334412, 20.99999999999998934, 3.637614988394418880 ) ) ;
#16486 = VECTOR ( 'NONE', #91022, 1000.000000000000000 ) ;
#16487 = LINE ( 'NONE', #80886, #41179 ) ;
#16488 = CARTESIAN_POINT ( 'NONE',  ( -110.6271891850301330, -285.5884205087698433, -273.6657232316608770 ) ) ;
#16489 = CARTESIAN_POINT ( 'NONE',  ( -49.90361924240939118, -284.9702995300782504, -345.3554070977949095 ) ) ;
#16490 = CARTESIAN_POINT ( 'NONE',  ( -4.541398034956920959, -285.8448308217389240, -205.0309346739786349 ) ) ;
#16491 = CARTESIAN_POINT ( 'NONE',  ( -85.99648656322791851, -277.7642414396756294, -214.8710092223476522 ) ) ;
#16492 = CARTESIAN_POINT ( 'NONE',  ( -110.6445316755044246, -286.5657634965576221, -258.5518267821323661 ) ) ;
#16493 = CARTESIAN_POINT ( 'NONE',  ( -49.23491877125587024, -278.3776952845079222, -197.6338252979622609 ) ) ;
#16494 = EDGE_CURVE ( 'NONE', #44867, #75656, #74170, .T. ) ;
#16495 = CARTESIAN_POINT ( 'NONE',  ( -66.91480399848555294, -278.5287697493715768, -337.4406051737995540 ) ) ;
#16496 = EDGE_CURVE ( 'NONE', #16264, #51979, #10861, .T. ) ;
#16497 = CARTESIAN_POINT ( 'NONE',  ( 207.2816333161762543, 35.50654163870040492, 14.49999997652496475 ) ) ;
#16498 = CARTESIAN_POINT ( 'NONE',  ( -40.78411110627732228, -274.5001739641683685, -197.3309793621284882 ) ) ;
#16499 = CARTESIAN_POINT ( 'NONE',  ( 37.39371018297305937, -282.5793987640058162, -288.2716080552581275 ) ) ;
#16500 = CARTESIAN_POINT ( 'NONE',  ( 37.27004240184719208, -281.8093584697490428, -251.5830781455788951 ) ) ;
#16501 = VERTEX_POINT ( 'NONE', #9773 ) ;
#16502 = ORIENTED_EDGE ( 'NONE', *, *, #67573, .T. ) ;
#16503 = CARTESIAN_POINT ( 'NONE',  ( 196.2760846862214805, 19.11198087481130514, -12.12215979492470552 ) ) ;
#16504 = CARTESIAN_POINT ( 'NONE',  ( 23.69391603993715378, -288.8065495477807758, -225.4728228318831214 ) ) ;
#16505 = CARTESIAN_POINT ( 'NONE',  ( -110.2101549340380018, -295.8426013340413760, -263.2738676620968477 ) ) ;
#16506 = CARTESIAN_POINT ( 'NONE',  ( -39.20090162447199589, -291.3780169100749049, -193.4725110917958091 ) ) ;
#16507 = CARTESIAN_POINT ( 'NONE',  ( 33.70278637241463571, -285.7757349934631748, -250.7808041061944664 ) ) ;
#16509 = CARTESIAN_POINT ( 'NONE',  ( -22.51603766146757124, -290.4844075091629065, -197.8478520005486985 ) ) ;
#16508 = CARTESIAN_POINT ( 'NONE',  ( 21.63491651461685450, -286.7397549024686896, -314.3950853371051153 ) ) ;
#16510 = CARTESIAN_POINT ( 'NONE',  ( -2.008638853555458681, -287.7357984502024237, -205.9713285316565532 ) ) ;
#16511 = CARTESIAN_POINT ( 'NONE',  ( -112.0882334939014982, -276.4651448873058257, -277.1246959048369263 ) ) ;
#16512 = CARTESIAN_POINT ( 'NONE',  ( -54.34315832023415282, -287.6667457335944960, -344.6944057267452308 ) ) ;
#16513 = CARTESIAN_POINT ( 'NONE',  ( -16.00740602988867778, -288.3280766878202712, -198.4055119750116774 ) ) ;
#16514 = CARTESIAN_POINT ( 'NONE',  ( -98.39638342483668509, -287.9564642696454371, -314.2278384150113766 ) ) ;
#16515 = CARTESIAN_POINT ( 'NONE',  ( -53.73070220970032551, -284.2087921836017017, -341.7912992270585164 ) ) ;
#16516 = CARTESIAN_POINT ( 'NONE',  ( -87.44682410682791840, -293.3551532500932240, -214.3298323020380280 ) ) ;
#16517 = CARTESIAN_POINT ( 'NONE',  ( 196.7806748523260012, 214.5000000000000568, -12.67104836398113576 ) ) ;
#16518 = CARTESIAN_POINT ( 'NONE',  ( 169.2494399300530290, -11.64849832608277325, 10.00000000000000000 ) ) ;
#16519 = CARTESIAN_POINT ( 'NONE',  ( -110.2394469566807516, -298.7282720623109071, -250.2870842909765088 ) ) ;
#16520 = CARTESIAN_POINT ( 'NONE',  ( -16.86675146023991800, -279.5206228940199935, -200.1231068804207496 ) ) ;
#16521 = CARTESIAN_POINT ( 'NONE',  ( 26.86120017710582886, -279.0314419258011753, -231.4920272185184444 ) ) ;
#16522 = CARTESIAN_POINT ( 'NONE',  ( -30.61529171246746017, -294.1663133068984735, -346.9046627805101366 ) ) ;
#16523 = CARTESIAN_POINT ( 'NONE',  ( -65.86327945056973476, -296.0725328974735362, -202.2952680342497729 ) ) ;
#16524 = CARTESIAN_POINT ( 'NONE',  ( 37.03950442556730849, -273.6844341870293533, -274.4149561970679656 ) ) ;
#16525 = CARTESIAN_POINT ( 'NONE',  ( -103.2027118377443173, -297.4268339773159937, -303.0884990067556828 ) ) ;
#16526 = CARTESIAN_POINT ( 'NONE',  ( -112.4854464783379626, -271.3050811119263699, -256.2217232971853491 ) ) ;
#16527 = CARTESIAN_POINT ( 'NONE',  ( -76.57844423901413222, -293.8089776510904585, -335.4950088749483257 ) ) ;
#16528 = CARTESIAN_POINT ( 'NONE',  ( -4.586988783727667496, -293.9176255201798540, -204.4494055515882849 ) ) ;
#16529 = DIRECTION ( 'NONE',  ( 0.9951408606192333473, 1.205805641958531838E-17, 0.09846150276129089773 ) ) ;
#16530 = CARTESIAN_POINT ( 'NONE',  ( 24.56934635180464355, -294.8934078116631667, -309.4386580128612536 ) ) ;
#16531 = DIRECTION ( 'NONE',  ( 0.000000000000000000, 0.000000000000000000, 1.000000000000000000 ) ) ;
#16533 = CARTESIAN_POINT ( 'NONE',  ( -5.541508154679747555, -294.6218125527207121, -336.0845001079460985 ) ) ;
#16532 = CARTESIAN_POINT ( 'NONE',  ( -65.24437450696409257, -283.7094306740340244, -200.3483568676285813 ) ) ;
#16534 = CARTESIAN_POINT ( 'NONE',  ( 25.10728869895594784, -282.1496775971746160, -315.4292963384559698 ) ) ;
#16535 = CARTESIAN_POINT ( 'NONE',  ( 3.031495501927004455, -282.5094396885168067, -206.4297773827819071 ) ) ;
#16536 = CARTESIAN_POINT ( 'NONE',  ( -100.9766187974619669, -284.7913280814240125, -226.9502066504495019 ) ) ;
#16537 = CARTESIAN_POINT ( 'NONE',  ( -95.70513171976759281, -289.1979716331697432, -223.5034035790035034 ) ) ;
#16538 = FACE_OUTER_BOUND ( 'NONE', #79504, .T. ) ;
#16539 = CARTESIAN_POINT ( 'NONE',  ( -33.19418945550215483, -284.7901519432418809, -196.9349329425350561 ) ) ;
#16540 = CARTESIAN_POINT ( 'NONE',  ( -95.23403138546342461, -288.7898973745052444, -320.6599300160514190 ) ) ;
#16541 = DIRECTION ( 'NONE',  ( 0.000000000000000000, 0.000000000000000000, -1.000000000000000000 ) ) ;
#16542 = CARTESIAN_POINT ( 'NONE',  ( 10.82893419783008149, -295.9728759983894975, -326.2720328544501740 ) ) ;
#16543 = CARTESIAN_POINT ( 'NONE',  ( -109.1765605292114572, -279.6441607903888098, -296.5611266592933362 ) ) ;
#16545 = CARTESIAN_POINT ( 'NONE',  ( 18.50778624523281124, -281.8871264321269337, -317.4222352571952115 ) ) ;
#16544 = CARTESIAN_POINT ( 'NONE',  ( -25.19826087222318378, -292.9183127822433903, -344.7843406239869637 ) ) ;
#16546 = CARTESIAN_POINT ( 'NONE',  ( -4.500606725706624900, -294.7979782817109253, -340.0208505656364082 ) ) ;
#16547 = CARTESIAN_POINT ( 'NONE',  ( -36.55538718224669736, -284.1417995229576263, -194.7924098791358745 ) ) ;
#16548 = CARTESIAN_POINT ( 'NONE',  ( -59.06085132000310978, -279.3333775742248122, -342.1474615160801704 ) ) ;
#16550 = CARTESIAN_POINT ( 'NONE',  ( 12.50628232010619989, -293.3960107692028032, -324.0830788710815682 ) ) ;
#16549 = AXIS2_PLACEMENT_3D ( 'NONE', #92578, #13541, #18767 ) ;
#16551 = CARTESIAN_POINT ( 'NONE',  ( -34.81716171435881790, -296.0835975648974454, -195.3619699642200658 ) ) ;
#16552 = EDGE_LOOP ( 'NONE', ( #48242, #79857, #31588, #59612 ) ) ;
#16553 = CARTESIAN_POINT ( 'NONE',  ( 203.5977283565847529, 62.01285785379746329, -9.999999999999998224 ) ) ;
#16554 = CARTESIAN_POINT ( 'NONE',  ( 8.124655973759523420, -282.6567890757721671, -211.0955899426531630 ) ) ;
#16555 = CARTESIAN_POINT ( 'NONE',  ( -101.5243624944597656, -295.5837371900188373, -305.2692014740655395 ) ) ;
#16556 = DIRECTION ( 'NONE',  ( -0.9849620900324524975, 0.000000000000000000, 0.1727706028203382094 ) ) ;
#16557 = CIRCLE ( 'NONE', #51353, 4.999999999999990230 ) ;
#16558 = CARTESIAN_POINT ( 'NONE',  ( 39.58706461736021254, -273.0523547857348490, -270.3937649182068981 ) ) ;
#16559 = CARTESIAN_POINT ( 'NONE',  ( -90.04465218943455795, -272.5275496901165297, -214.3728379144395149 ) ) ;
#16560 = CARTESIAN_POINT ( 'NONE',  ( 38.86185206922998958, -288.7745188734546105, -262.9880217815069159 ) ) ;
#16561 = CARTESIAN_POINT ( 'NONE',  ( -108.7101204244019215, -290.5879318778430616, -255.0135256976755045 ) ) ;
#16562 = CARTESIAN_POINT ( 'NONE',  ( -83.89053372344525883, -280.9198625248510552, -213.1643822479373682 ) ) ;
#16563 = CARTESIAN_POINT ( 'NONE',  ( -77.01123119773561143, -275.1110247544981462, -208.1295446531418634 ) ) ;
#16564 = CARTESIAN_POINT ( 'NONE',  ( -99.79758790485261954, -277.8769892727284514, -231.7104296342984355 ) ) ;
#16565 = CARTESIAN_POINT ( 'NONE',  ( -40.56695969248433897, -279.0928470236354428, -345.3045476445147415 ) ) ;
#16566 = ORIENTED_EDGE ( 'NONE', *, *, #40929, .T. ) ;
#16567 = CARTESIAN_POINT ( 'NONE',  ( -35.52165913859401059, -273.9076877626553141, -193.3695008561130635 ) ) ;
#16568 = CARTESIAN_POINT ( 'NONE',  ( -55.38459516852005038, -293.7383635643948878, -198.1408428965641519 ) ) ;
#16569 = DIRECTION ( 'NONE',  ( -1.000000000000000000, 0.000000000000000000, -0.000000000000000000 ) ) ;
#16570 = CARTESIAN_POINT ( 'NONE',  ( 196.7672805984238096, 69.63494095281957641, 10.95706626401136141 ) ) ;
#16571 = CARTESIAN_POINT ( 'NONE',  ( 36.56180181112865313, -291.4789319421396954, -253.6122142194242599 ) ) ;
#16572 = CARTESIAN_POINT ( 'NONE',  ( -35.14269840491157026, -297.7471451163913798, -197.3401024252837033 ) ) ;
#16573 = CARTESIAN_POINT ( 'NONE',  ( 104.1717476309105166, -299.5541904835127980, -195.3611179825600175 ) ) ;
#16574 = CARTESIAN_POINT ( 'NONE',  ( -111.2456487715862750, -291.8317643424948642, -289.4110771189849629 ) ) ;
#16575 = CARTESIAN_POINT ( 'NONE',  ( -99.86837403722181250, -286.4090924074130839, -320.2651865833026363 ) ) ;
#16576 = CARTESIAN_POINT ( 'NONE',  ( 27.95493599005039087, -289.0632564934966240, -233.6986580070584694 ) ) ;
#16577 = CARTESIAN_POINT ( 'NONE',  ( -43.37978663416922132, -275.1284415255420868, -344.9504599700417771 ) ) ;
#16578 = CARTESIAN_POINT ( 'NONE',  ( 23.65966024366784737, -278.0567709715322167, -313.1128473509648416 ) ) ;
#16579 = CARTESIAN_POINT ( 'NONE',  ( -84.72723957118482474, -289.4729267960509560, -212.9509721318022173 ) ) ;
#16580 = CARTESIAN_POINT ( 'NONE',  ( -95.87847397356016188, -281.0693824707078647, -222.2394647571321968 ) ) ;
#16581 = EDGE_LOOP ( 'NONE', ( #87257, #17416, #90395, #69752, #9102 ) ) ;
#16582 = CARTESIAN_POINT ( 'NONE',  ( 19.42595148636108959, -281.5517253892375038, -316.4387056566170031 ) ) ;
#16583 = CARTESIAN_POINT ( 'NONE',  ( -111.7891843422113567, -279.8637154166078744, -251.8934921609886146 ) ) ;
#16584 = CARTESIAN_POINT ( 'NONE',  ( 6.684191623652922409, -281.2633642591031844, -333.1135284865397921 ) ) ;
#16585 = CARTESIAN_POINT ( 'NONE',  ( -96.86432128102880768, -278.8406832494876539, -318.8572366785006125 ) ) ;
#16586 = ADVANCED_FACE ( 'NONE', ( #24439 ), #21427, .T. ) ;
#16587 = DIRECTION ( 'NONE',  ( 0.000000000000000000, 0.000000000000000000, 1.000000000000000000 ) ) ;
#16588 = CARTESIAN_POINT ( 'NONE',  ( 38.69130997034513797, -277.1537561154045761, -276.8178297470652751 ) ) ;
#16589 = CARTESIAN_POINT ( 'NONE',  ( -53.35057174420112602, -288.3376638359845288, -200.3683826091709648 ) ) ;
#16590 = VERTEX_POINT ( 'NONE', #67551 ) ;
#16591 = EDGE_LOOP ( 'NONE', ( #27881, #14423, #27408, #13486 ) ) ;
#16592 = CARTESIAN_POINT ( 'NONE',  ( -98.80827511514078765, -297.9690220871698330, -313.3362364723429891 ) ) ;
#16593 = CARTESIAN_POINT ( 'NONE',  ( -13.17305126566774653, -289.8103282580185009, -339.5716842676411602 ) ) ;
#16594 = CARTESIAN_POINT ( 'NONE',  ( -4.361561768623137603, -274.6355004930742894, -337.3391700317607160 ) ) ;
#16595 = CARTESIAN_POINT ( 'NONE',  ( -106.7959276644553483, -291.9122061246599742, -301.3138820116714669 ) ) ;
#16596 = CARTESIAN_POINT ( 'NONE',  ( -12.21739217684053180, -291.7363020262033046, -201.6583328883540389 ) ) ;
#16597 = CARTESIAN_POINT ( 'NONE',  ( 38.72568047040571315, -286.9142102136819403, -258.7286358004117233 ) ) ;
#16598 = CARTESIAN_POINT ( 'NONE',  ( 208.9422428205583344, 36.81742993605089964, 13.19543921975815692 ) ) ;
#16599 = CARTESIAN_POINT ( 'NONE',  ( -43.01452379734985954, -281.5246725783801480, -343.9934050351565133 ) ) ;
#16600 = CARTESIAN_POINT ( 'NONE',  ( -75.32794126452058947, -291.4247122553418876, -334.1562276091738113 ) ) ;
#16601 = CARTESIAN_POINT ( 'NONE',  ( -107.6531208500526446, -282.7422845002179770, -292.4294633829376266 ) ) ;
#16602 = ADVANCED_FACE ( 'NONE', ( #87432 ), #82205, .T. ) ;
#16603 = CARTESIAN_POINT ( 'NONE',  ( 35.19296310955536455, -283.0223503051468583, -282.1918452448913399 ) ) ;
#16604 = CARTESIAN_POINT ( 'NONE',  ( 5.436172385197808765, -289.4295337490643192, -334.1017944435105846 ) ) ;
#16605 = CARTESIAN_POINT ( 'NONE',  ( -68.55526625356546333, -280.1228635531553550, -204.3027972984460803 ) ) ;
#16606 = CARTESIAN_POINT ( 'NONE',  ( -69.44269181578539474, -290.4339844571298386, -200.7944607697111792 ) ) ;
#16607 = CARTESIAN_POINT ( 'NONE',  ( -10.06087450454213084, -287.2021139036569366, -198.4718885790336458 ) ) ;
#16608 = CARTESIAN_POINT ( 'NONE',  ( -17.73395569408640071, -289.2981579022102778, -344.7591237439553424 ) ) ;
#16609 = CARTESIAN_POINT ( 'NONE',  ( -67.78243368195637686, -283.6298482048885603, -336.7114137259426343 ) ) ;
#16610 = VERTEX_POINT ( 'NONE', #17359 ) ;
#16611 = CARTESIAN_POINT ( 'NONE',  ( 76.08708295871279859, -296.0521521680024080, -465.6442049081569508 ) ) ;
#16612 = CARTESIAN_POINT ( 'NONE',  ( 8.090996660351315484, -294.5258976937257671, -209.6641808921635004 ) ) ;
#16613 = CARTESIAN_POINT ( 'NONE',  ( 1.504518319981962282, -293.2291034164159669, -336.2721912929378618 ) ) ;
#16614 = CARTESIAN_POINT ( 'NONE',  ( -11.18115149360161986, -275.7613903733028451, -338.7645838548054940 ) ) ;
#16615 = CARTESIAN_POINT ( 'NONE',  ( -85.14656004788000132, -296.7601281949540066, -210.1281689071860797 ) ) ;
#16616 = AXIS2_PLACEMENT_3D ( 'NONE', #60693, #6682, #70610 ) ;
#16617 = CARTESIAN_POINT ( 'NONE',  ( 20.22333621356631284, -292.6760857553618393, -316.3918166350993033 ) ) ;
#16618 = CARTESIAN_POINT ( 'NONE',  ( -108.4264476208809214, -295.0609326531775309, -249.7472224644902212 ) ) ;
#16619 = CARTESIAN_POINT ( 'NONE',  ( -106.0879254558679463, -292.1000972868071699, -244.5052073947672113 ) ) ;
#16620 = CARTESIAN_POINT ( 'NONE',  ( 4.002002081043565695, -295.5601881082467912, -330.8997367362131854 ) ) ;
#16621 = CARTESIAN_POINT ( 'NONE',  ( 10.02285351824489545, -292.4014632715156381, -328.7944964748160714 ) ) ;
#16622 = AXIS2_PLACEMENT_3D ( 'NONE', #76693, #61108, #4254 ) ;
#16623 = CARTESIAN_POINT ( 'NONE',  ( -54.95338414395156690, -299.8260138613728714, -197.4054602042285183 ) ) ;
#16624 = CARTESIAN_POINT ( 'NONE',  ( 32.05975957181172475, -288.1837494451146426, -246.9763828001674995 ) ) ;
#16625 = CARTESIAN_POINT ( 'NONE',  ( -45.44709109661332036, -279.1341254417251889, -345.3310606528314679 ) ) ;
#16626 = CARTESIAN_POINT ( 'NONE',  ( -4.180698034977837096, -275.4195821011981025, -339.4288288812909968 ) ) ;
#16627 = CARTESIAN_POINT ( 'NONE',  ( -13.08676520435249735, -273.7078072724917206, -197.3884455754348153 ) ) ;
#16628 = CARTESIAN_POINT ( 'NONE',  ( 35.16851085794340293, -279.4141466836844643, -253.5211801947434083 ) ) ;
#16629 = CARTESIAN_POINT ( 'NONE',  ( -86.59380599429820791, -276.1228346574709462, -328.5737064726159815 ) ) ;
#16630 = CARTESIAN_POINT ( 'NONE',  ( -101.9085013149341137, -294.7610428254607768, -305.4662694744997111 ) ) ;
#16631 = DIRECTION ( 'NONE',  ( 0.000000000000000000, 0.000000000000000000, 1.000000000000000000 ) ) ;
#16632 = CARTESIAN_POINT ( 'NONE',  ( -41.88856856187663880, -298.7962259635968962, -197.3410678961627980 ) ) ;
#16633 = CYLINDRICAL_SURFACE ( 'NONE', #9581, 7.500000000000007105 ) ;
#16634 = CARTESIAN_POINT ( 'NONE',  ( -112.7445743867030501, -288.5617275316047881, -271.1850599948281229 ) ) ;
#16635 = CARTESIAN_POINT ( 'NONE',  ( -95.45830251453908488, -289.8693943026705142, -320.8731019769981572 ) ) ;
#16636 = CARTESIAN_POINT ( 'NONE',  ( -90.88152259847159087, -275.2946102171149505, -217.6020824004652354 ) ) ;
#16637 = CARTESIAN_POINT ( 'NONE',  ( -104.4225965765146213, -294.1120329240526985, -303.6472851570148350 ) ) ;
#16638 = CARTESIAN_POINT ( 'NONE',  ( -27.40313773521852170, -282.1262361771995302, -346.6074359898632338 ) ) ;
#16639 = CYLINDRICAL_SURFACE ( 'NONE', #27507, 4.999999999999986677 ) ;
#16640 = CARTESIAN_POINT ( 'NONE',  ( -3.309959604635070107, -280.6026638383646628, -337.2097237280163995 ) ) ;
#16641 = CARTESIAN_POINT ( 'NONE',  ( 197.8939195897753223, 25.00231265943466497, 11.19330938564888100 ) ) ;
#16642 = CARTESIAN_POINT ( 'NONE',  ( -104.4167981935732854, -288.9465814387197042, -300.2870565187305374 ) ) ;
#16643 = CARTESIAN_POINT ( 'NONE',  ( -65.81094376173723504, -281.5681259760785338, -338.9341761079012940 ) ) ;
#16644 = CARTESIAN_POINT ( 'NONE',  ( 200.1223792991399364, 214.7033776542919270, -2.619521892235705973 ) ) ;
#16645 = CARTESIAN_POINT ( 'NONE',  ( -6.024775384615294271, -229.5268262511776527, 21.50000000000000000 ) ) ;
#16646 = CARTESIAN_POINT ( 'NONE',  ( 34.66336099941894133, -291.8226894915986804, -291.3898781576239685 ) ) ;
#16647 = CARTESIAN_POINT ( 'NONE',  ( -79.26526013879282573, -274.9954010433622216, -209.6928279343022439 ) ) ;
#16648 = CARTESIAN_POINT ( 'NONE',  ( -96.85415627650654358, -285.1067409886590553, -318.6132130463360568 ) ) ;
#16650 = CARTESIAN_POINT ( 'NONE',  ( -35.93346748634294840, -286.0703032089222120, -197.3747022545168761 ) ) ;
#16649 = CARTESIAN_POINT ( 'NONE',  ( -57.70949575392910447, -271.8711450248882215, -197.5436457669048025 ) ) ;
#16651 = CARTESIAN_POINT ( 'NONE',  ( -13.57809017561891451, -278.1629319208394691, -340.0614111827846386 ) ) ;
#16652 = CARTESIAN_POINT ( 'NONE',  ( 16.65722802147351445, -277.0616961827885802, -319.7429250538532983 ) ) ;
#16653 = CARTESIAN_POINT ( 'NONE',  ( -109.1846454337006236, -286.2743845888787746, -291.9368457786694080 ) ) ;
#16654 = ORIENTED_EDGE ( 'NONE', *, *, #82838, .F. ) ;
#16655 = DIRECTION ( 'NONE',  ( 0.000000000000000000, 0.000000000000000000, 1.000000000000000000 ) ) ;
#16656 = CARTESIAN_POINT ( 'NONE',  ( -64.26817501740804062, -295.2273115250155229, -342.4996302664839618 ) ) ;
#16657 = CARTESIAN_POINT ( 'NONE',  ( -46.96127114263693869, -287.9094207338338265, -196.2868315012454445 ) ) ;
#16658 = DIRECTION ( 'NONE',  ( 0.000000000000000000, 0.000000000000000000, -1.000000000000000000 ) ) ;
#16659 = CARTESIAN_POINT ( 'NONE',  ( 25.18497378105905682, -291.6952119285918457, -320.2651865833026363 ) ) ;
#16660 = CARTESIAN_POINT ( 'NONE',  ( -113.9240673415976914, -277.4212706380361624, -274.4395418132581312 ) ) ;
#16661 = CARTESIAN_POINT ( 'NONE',  ( -14.09096378886128953, -290.7485566597673028, -197.7395863940748200 ) ) ;
#16662 = CARTESIAN_POINT ( 'NONE',  ( -110.1806611274039653, -285.9217952942664169, -281.8769456942854390 ) ) ;
#16663 = CARTESIAN_POINT ( 'NONE',  ( -111.4058787188907900, -280.3083569482387247, -270.6642684498999643 ) ) ;
#16664 = CARTESIAN_POINT ( 'NONE',  ( -57.61719115473270847, -287.2207739247929794, -196.6345448348295122 ) ) ;
#16665 = CARTESIAN_POINT ( 'NONE',  ( 32.19820235310088918, -283.9184661564850671, -298.4538681008904746 ) ) ;
#16666 = CARTESIAN_POINT ( 'NONE',  ( 29.09701888490610955, -276.2254497171056755, -309.2827908706128142 ) ) ;
#16667 = CARTESIAN_POINT ( 'NONE',  ( -58.34395346716120656, -295.7994415028941262, -198.7318491403834742 ) ) ;
#16668 = CARTESIAN_POINT ( 'NONE',  ( -62.04562041376767212, -279.5730908147767764, -197.3753562166192523 ) ) ;
#16669 = CARTESIAN_POINT ( 'NONE',  ( -110.7796133457702581, -298.3148300733818132, -282.5343304283009047 ) ) ;
#16670 = CARTESIAN_POINT ( 'NONE',  ( 158.9078607026168868, 16.88031981475927878, 10.36078569760431201 ) ) ;
#16671 = CARTESIAN_POINT ( 'NONE',  ( -20.25526795762937127, -282.7662352645560304, -195.3538533559490702 ) ) ;
#16672 = VECTOR ( 'NONE', #88753, 1000.000000000000114 ) ;
#16673 = CARTESIAN_POINT ( 'NONE',  ( -67.66103878417175110, -295.7982870827341344, -200.8715086904071825 ) ) ;
#16674 = CARTESIAN_POINT ( 'NONE',  ( -29.71322858056420912, -276.4607539649181263, -343.0742634720691058 ) ) ;
#16675 = CARTESIAN_POINT ( 'NONE',  ( 2.199830783842639192, -275.7744776916161982, -204.7526120442273054 ) ) ;
#16676 = AXIS2_PLACEMENT_3D ( 'NONE', #6426, #35301, #19223 ) ;
#16677 = CARTESIAN_POINT ( 'NONE',  ( 34.36343591443964840, -280.9589614345642303, -297.7690306647259035 ) ) ;
#16678 = CARTESIAN_POINT ( 'NONE',  ( -76.38451919106526589, -291.3422354525838500, -333.2390337592499350 ) ) ;
#16679 = CARTESIAN_POINT ( 'NONE',  ( -70.44592109806045244, -299.1437502742176662, -201.6092575717512432 ) ) ;
#16680 = CARTESIAN_POINT ( 'NONE',  ( -113.2106445988670345, -297.8914079548573568, -259.6872502846215980 ) ) ;
#16681 = CARTESIAN_POINT ( 'NONE',  ( 36.00856305734165375, -295.3615418228174008, -255.5365667100240046 ) ) ;
#16682 = CARTESIAN_POINT ( 'NONE',  ( 21.60986937353373349, -280.1858429268737609, -316.4560296767756427 ) ) ;
#16683 = CARTESIAN_POINT ( 'NONE',  ( -13.87771831593073024, -282.2790091167194646, -199.6613498208154169 ) ) ;
#16684 = CARTESIAN_POINT ( 'NONE',  ( -68.63093441433395014, -295.7175919946152476, -202.8024002807403861 ) ) ;
#16685 = CARTESIAN_POINT ( 'NONE',  ( -100.3466352374932598, -286.7244256683174513, -227.4097521604752501 ) ) ;
#16686 = CARTESIAN_POINT ( 'NONE',  ( -34.58007291766566027, -287.9371034895813182, -343.6679884395664999 ) ) ;
#16687 = CARTESIAN_POINT ( 'NONE',  ( -88.66512920003211207, -231.2529867285488194, -347.6922890233383328 ) ) ;
#16688 = ORIENTED_EDGE ( 'NONE', *, *, #47145, .T. ) ;
#16689 = CARTESIAN_POINT ( 'NONE',  ( -20.64298893186897388, -287.4166789574570657, -344.9791576148476224 ) ) ;
#16690 = CARTESIAN_POINT ( 'NONE',  ( -4.581271205340105901, -286.1629113725178399, -205.1013157788832757 ) ) ;
#16691 = EDGE_LOOP ( 'NONE', ( #38062, #78353, #27341, #48439 ) ) ;
#16692 = CARTESIAN_POINT ( 'NONE',  ( -31.64547412384881397, -284.0615321495145054, -346.8533855063180340 ) ) ;
#16693 = CARTESIAN_POINT ( 'NONE',  ( -11.48670431295657401, -274.7315812325054480, -202.0164529802044342 ) ) ;
#16694 = CARTESIAN_POINT ( 'NONE',  ( -106.9739778131460355, -289.8866986808618549, -238.0968387838896945 ) ) ;
#16695 = CARTESIAN_POINT ( 'NONE',  ( 29.19422860332015901, -281.7015377682966459, -231.8087772729147957 ) ) ;
#16696 = EDGE_CURVE ( 'NONE', #7995, #73033, #74335, .T. ) ;
#16697 = CARTESIAN_POINT ( 'NONE',  ( 3.434962784590767093, -282.1094720554947912, -205.8008718855227528 ) ) ;
#16698 = CARTESIAN_POINT ( 'NONE',  ( -13.42447551844505860, -283.0831286378585787, -343.5301733163346398 ) ) ;
#16699 = CARTESIAN_POINT ( 'NONE',  ( -92.20843863198294343, -279.2396207305267808, -222.1898333213904380 ) ) ;
#16700 = CARTESIAN_POINT ( 'NONE',  ( -4.829096099716524648, -274.1237833571632905, -337.9475929042657754 ) ) ;
#16701 = CARTESIAN_POINT ( 'NONE',  ( 25.85751915286289560, -23.12262787077664328, -345.2578353262790074 ) ) ;
#16702 = ORIENTED_EDGE ( 'NONE', *, *, #63505, .F. ) ;
#16703 = CARTESIAN_POINT ( 'NONE',  ( 36.83446597737987815, -277.4249723051858609, -260.4654215366804806 ) ) ;
#16704 = CARTESIAN_POINT ( 'NONE',  ( -71.84640263648488201, -195.7149973669283725, -359.9635178732972918 ) ) ;
#16705 = CARTESIAN_POINT ( 'NONE',  ( -79.78049287100706977, -296.8096649928742750, -210.8393443328074284 ) ) ;
#16706 = CARTESIAN_POINT ( 'NONE',  ( 13.35056665728578551, -293.8731082478913095, -328.3093890327222084 ) ) ;
#16707 = CARTESIAN_POINT ( 'NONE',  ( -104.8259698489561345, -260.7805594622520857, -315.6649111131378049 ) ) ;
#16709 = CARTESIAN_POINT ( 'NONE',  ( -96.42086381693505359, -288.3377235919174950, -314.6099530810120655 ) ) ;
#16708 = CARTESIAN_POINT ( 'NONE',  ( -54.44549071380331640, -296.4112921872676907, -195.8891995241350799 ) ) ;
#16710 = CARTESIAN_POINT ( 'NONE',  ( -93.10309196270191023, -297.7246057258181509, -319.3665530137477617 ) ) ;
#16711 = CARTESIAN_POINT ( 'NONE',  ( -25.07589121249525377, -287.5268792226348751, -197.8471162547541553 ) ) ;
#16712 = ORIENTED_EDGE ( 'NONE', *, *, #44600, .T. ) ;
#16713 = CARTESIAN_POINT ( 'NONE',  ( 4.004675341371077835, -293.5354031762456657, -205.6197010608642302 ) ) ;
#16714 = CARTESIAN_POINT ( 'NONE',  ( -100.4511374388943921, -284.5396802038633837, -307.1739875236188482 ) ) ;
#16715 = CARTESIAN_POINT ( 'NONE',  ( -62.69906395948762423, -296.5242179048408957, -198.0768678473976649 ) ) ;
#16716 = CARTESIAN_POINT ( 'NONE',  ( -58.90318746132933114, -292.5829258906816221, -196.6097716623713723 ) ) ;
#16717 = CARTESIAN_POINT ( 'NONE',  ( 23.92242080290800388, -293.4235278237208604, -223.7966170806500656 ) ) ;
#16718 = CARTESIAN_POINT ( 'NONE',  ( -98.10949659709513071, -290.1570345452356605, -310.8347689664057043 ) ) ;
#16719 = EDGE_LOOP ( 'NONE', ( #73303, #35182, #69696, #45107, #41644 ) ) ;
#16720 = CARTESIAN_POINT ( 'NONE',  ( 157.3189109369757546, 16.43186977800927906, 7.221609175748572973 ) ) ;
#16721 = CARTESIAN_POINT ( 'NONE',  ( -62.45826993683399309, -299.5892154304821702, -198.8806073488312052 ) ) ;
#16722 = CARTESIAN_POINT ( 'NONE',  ( -52.45220064248928793, -272.6578244031910572, -195.2091471230187949 ) ) ;
#16723 = EDGE_CURVE ( 'NONE', #24735, #4620, #27515, .T. ) ;
#16724 = CARTESIAN_POINT ( 'NONE',  ( -34.85050550056043051, -282.0788736089846793, -343.5665070048286225 ) ) ;
#16725 = VERTEX_POINT ( 'NONE', #61393 ) ;
#16726 = VERTEX_POINT ( 'NONE', #82666 ) ;
#16727 = CARTESIAN_POINT ( 'NONE',  ( -41.38748410006525802, -276.6094357507039945, -347.2063312859026496 ) ) ;
#16728 = CARTESIAN_POINT ( 'NONE',  ( -94.38387301484451086, -271.6083786179167987, -223.5158270825274656 ) ) ;
#16729 = CARTESIAN_POINT ( 'NONE',  ( -95.77761551949956242, -281.0475114866662238, -224.5573629264747240 ) ) ;
#16730 = CARTESIAN_POINT ( 'NONE',  ( -36.47513038266711760, -275.1807984567030871, -344.6039423210291943 ) ) ;
#16731 = CARTESIAN_POINT ( 'NONE',  ( -77.74328183935186587, -298.7017095745386541, -209.0232651112983717 ) ) ;
#16732 = CARTESIAN_POINT ( 'NONE',  ( -68.39321470884395637, -274.5752097577409359, -204.0208202654678757 ) ) ;
#16733 = CARTESIAN_POINT ( 'NONE',  ( -95.26991934793608152, -274.9841904082319388, -221.1649092872881965 ) ) ;
#16734 = CARTESIAN_POINT ( 'NONE',  ( 12.88730599588936521, -272.7688335467515799, -214.1179405367782351 ) ) ;
#16735 = CARTESIAN_POINT ( 'NONE',  ( 34.16902223195484112, -294.4041884905151960, -285.5905447135049258 ) ) ;
#16736 = CARTESIAN_POINT ( 'NONE',  ( 20.65842752542369709, -291.4933828295686453, -225.0487686505224474 ) ) ;
#16737 = CARTESIAN_POINT ( 'NONE',  ( 144.2857639756989272, -299.5541904835127980, -201.0153591320744226 ) ) ;
#16738 = CARTESIAN_POINT ( 'NONE',  ( 1.021794398023314177, -277.0471486556504601, -337.1131479218443019 ) ) ;
#16739 = CARTESIAN_POINT ( 'NONE',  ( 2.928171180536085494, -274.7757281860425564, -209.4127974005153590 ) ) ;
#16740 = FACE_OUTER_BOUND ( 'NONE', #82408, .T. ) ;
#16741 =( BOUNDED_SURFACE ( )  B_SPLINE_SURFACE ( 3, 3, ( 
 ( #25860, #40515, #17846, #75599, #81757, #83151, #76069, #18302, #82233, #83620, #24469, #46697, #45766, #60478, #39123, #47160, #74676, #89314, #18781, #11199, #76543, #17390, #46239, #68035 ),
 ( #32046, #2707, #3636, #60940, #10722, #9800, #47640, #32527, #68502, #61421, #90253, #24005, #25402, #40059, #68976, #4106, #11666, #10255, #32978, #69433, #4563, #38674, #67579, #31589 ),
 ( #75143, #63765, #48103, #91664, #19702, #92595, #92129, #26818, #28231, #57119, #27764, #56171, #78872, #62830, #56659, #20655, #41461, #49059, #77955, #85028, #27284, #85508, #55704, #70393 ),
 ( #34853, #5041, #14021, #5521, #48572, #13556, #34391, #20179, #21111, #64247, #93077, #63298, #71795, #13098, #69902, #49525, #26347, #84555, #41936, #71316, #6917, #70848, #5981, #78418 ),
 ( #62340, #42406, #55240, #12135, #12616, #84096, #19245, #91181, #6447, #77007, #35322, #77473, #85960, #40980, #49979, #33921, #42882, #1201, #93531, #80266, #8751, #746, #74090, #51837 ),
 ( #86418, #35791, #73180, #50457, #79807, #29151, #59440, #28689, #50923, #21575, #58967, #30083, #57575, #15402, #37630, #29630, #64704, #79360, #36712, #269, #14495, #43353, #86899, #65633 ),
 ( #22963, #87814, #58048, #66539, #65165, #58509, #72249, #7366, #14949, #80730, #36247, #22054, #1659, #15883, #23446, #43803, #72703, #7822, #52314, #87354, #22504, #88291, #81191, #51375 ) ),
 .UNSPECIFIED., .T., .F., .F. ) 
 B_SPLINE_SURFACE_WITH_KNOTS ( ( 4, 3, 4 ),
 ( 4, 2, 2, 2, 2, 2, 2, 2, 2, 2, 2, 4 ),
 ( 0.000000000000000000, 0.5000000000000000000, 1.000000000000000000 ),
 ( 0.000000000000000000, 0.06250000000000000000, 0.1250000000000000000, 0.2500000000000000000, 0.3750000000000000000, 0.5000000000000000000, 0.6250000000000000000, 0.7500000000000000000, 0.8125000000000000000, 0.8750000000000000000, 0.9375000000000000000, 1.000000000000000000 ),
 .UNSPECIFIED. ) 
 GEOMETRIC_REPRESENTATION_ITEM ( )  RATIONAL_B_SPLINE_SURFACE ( (
 ( 1.000000000000000000, 1.000000000000000000, 1.000000000000000000, 1.000000000000000000, 1.000000000000000000, 1.000000000000000000, 1.000000000000000000, 1.000000000000000000, 1.000000000000000000, 1.000000000000000000, 1.000000000000000000, 1.000000000000000000, 1.000000000000000000, 1.000000000000000000, 1.000000000000000000, 1.000000000000000000, 1.000000000000000000, 1.000000000000000000, 1.000000000000000000, 1.000000000000000000, 1.000000000000000000, 1.000000000000000000, 1.000000000000000000, 1.000000000000000000),
 ( 0.3333333333333333703, 0.3333333333333333703, 0.3333333333333333703, 0.3333333333333333703, 0.3333333333333333703, 0.3333333333333333703, 0.3333333333333333703, 0.3333333333333333703, 0.3333333333333333703, 0.3333333333333333703, 0.3333333333333333703, 0.3333333333333333703, 0.3333333333333333703, 0.3333333333333333703, 0.3333333333333333703, 0.3333333333333333703, 0.3333333333333333703, 0.3333333333333333703, 0.3333333333333333703, 0.3333333333333333703, 0.3333333333333333703, 0.3333333333333333703, 0.3333333333333333703, 0.3333333333333333703),
 ( 0.3333333333333333703, 0.3333333333333333703, 0.3333333333333333703, 0.3333333333333333703, 0.3333333333333333703, 0.3333333333333333703, 0.3333333333333333703, 0.3333333333333333703, 0.3333333333333333703, 0.3333333333333333703, 0.3333333333333333703, 0.3333333333333333703, 0.3333333333333333703, 0.3333333333333333703, 0.3333333333333333703, 0.3333333333333333703, 0.3333333333333333703, 0.3333333333333333703, 0.3333333333333333703, 0.3333333333333333703, 0.3333333333333333703, 0.3333333333333333703, 0.3333333333333333703, 0.3333333333333333703),
 ( 1.000000000000000000, 1.000000000000000000, 1.000000000000000000, 1.000000000000000000, 1.000000000000000000, 1.000000000000000000, 1.000000000000000000, 1.000000000000000000, 1.000000000000000000, 1.000000000000000000, 1.000000000000000000, 1.000000000000000000, 1.000000000000000000, 1.000000000000000000, 1.000000000000000000, 1.000000000000000000, 1.000000000000000000, 1.000000000000000000, 1.000000000000000000, 1.000000000000000000, 1.000000000000000000, 1.000000000000000000, 1.000000000000000000, 1.000000000000000000),
 ( 0.3333333333333333703, 0.3333333333333333703, 0.3333333333333333703, 0.3333333333333333703, 0.3333333333333333703, 0.3333333333333333703, 0.3333333333333333703, 0.3333333333333333703, 0.3333333333333333703, 0.3333333333333333703, 0.3333333333333333703, 0.3333333333333333703, 0.3333333333333333703, 0.3333333333333333703, 0.3333333333333333703, 0.3333333333333333703, 0.3333333333333333703, 0.3333333333333333703, 0.3333333333333333703, 0.3333333333333333703, 0.3333333333333333703, 0.3333333333333333703, 0.3333333333333333703, 0.3333333333333333703),
 ( 0.3333333333333333703, 0.3333333333333333703, 0.3333333333333333703, 0.3333333333333333703, 0.3333333333333333703, 0.3333333333333333703, 0.3333333333333333703, 0.3333333333333333703, 0.3333333333333333703, 0.3333333333333333703, 0.3333333333333333703, 0.3333333333333333703, 0.3333333333333333703, 0.3333333333333333703, 0.3333333333333333703, 0.3333333333333333703, 0.3333333333333333703, 0.3333333333333333703, 0.3333333333333333703, 0.3333333333333333703, 0.3333333333333333703, 0.3333333333333333703, 0.3333333333333333703, 0.3333333333333333703),
 ( 1.000000000000000000, 1.000000000000000000, 1.000000000000000000, 1.000000000000000000, 1.000000000000000000, 1.000000000000000000, 1.000000000000000000, 1.000000000000000000, 1.000000000000000000, 1.000000000000000000, 1.000000000000000000, 1.000000000000000000, 1.000000000000000000, 1.000000000000000000, 1.000000000000000000, 1.000000000000000000, 1.000000000000000000, 1.000000000000000000, 1.000000000000000000, 1.000000000000000000, 1.000000000000000000, 1.000000000000000000, 1.000000000000000000, 1.000000000000000000) ) ) 
 REPRESENTATION_ITEM ( '' )  SURFACE ( )  );
#16742 = CARTESIAN_POINT ( 'NONE',  ( -96.79979644121846150, -282.5868995251412912, -318.5276663424640446 ) ) ;
#16743 = CARTESIAN_POINT ( 'NONE',  ( -5.261297044893791686, -296.6311619340227708, -338.3522728317411747 ) ) ;
#16744 = DIRECTION ( 'NONE',  ( 1.000000000000000000, 0.000000000000000000, 0.000000000000000000 ) ) ;
#16745 =( BOUNDED_SURFACE ( )  B_SPLINE_SURFACE ( 3, 2, ( 
 ( #36205, #29106, #65123 ),
 ( #58000, #86856, #22012 ),
 ( #50882, #14906, #43762 ),
 ( #72662, #703, #44694 ),
 ( #82069, #30497, #23402 ),
 ( #9162, #87769, #66495 ) ),
 .UNSPECIFIED., .F., .F., .F. ) 
 B_SPLINE_SURFACE_WITH_KNOTS ( ( 4, 2, 4 ),
 ( 3, 3 ),
 ( 0.000000000000000000, 0.001526582434089618920, 0.003053164868179237840 ),
 ( 0.000000000000000000, 1.000000000000000000 ),
 .UNSPECIFIED. ) 
 GEOMETRIC_REPRESENTATION_ITEM ( )  RATIONAL_B_SPLINE_SURFACE ( (
 ( 1.000000000000000000, 0.7071067811865475727, 1.000000000000000000),
 ( 1.000000000000000000, 0.7219865977747690344, 1.000000000000000000),
 ( 1.000000000000000000, 0.7353530398652478040, 1.000000000000000000),
 ( 1.000000000000000000, 0.7593109839642017134, 1.000000000000000000),
 ( 1.000000000000000000, 0.7699014431358252031, 1.000000000000000000),
 ( 1.000000000000000000, 0.7791885400064315625, 1.000000000000000000) ) ) 
 REPRESENTATION_ITEM ( '' )  SURFACE ( )  );
#16746 = CARTESIAN_POINT ( 'NONE',  ( -52.11156656865038883, -285.0553676782051298, -198.7060220593892836 ) ) ;
#16747 = CARTESIAN_POINT ( 'NONE',  ( -16.67104662481317945, -280.7856996581161297, -342.6836949580940654 ) ) ;
#16748 = CARTESIAN_POINT ( 'NONE',  ( 3.445730556832286684, -275.0664693080626648, -331.6127335879007205 ) ) ;
#16749 = CARTESIAN_POINT ( 'NONE',  ( 37.56384445359252311, -283.4922763771189125, -265.6850453032252517 ) ) ;
#16750 = CARTESIAN_POINT ( 'NONE',  ( 34.50690351078471707, -276.5596619019306672, -255.3028668267381533 ) ) ;
#16751 = CARTESIAN_POINT ( 'NONE',  ( 85.55100297371598117, -298.0521521680024080, -413.1172536214571096 ) ) ;
#16752 = CARTESIAN_POINT ( 'NONE',  ( 194.7272697300732887, 19.95005744978422157, 14.17304058800352884 ) ) ;
#16753 = CARTESIAN_POINT ( 'NONE',  ( -32.71064855606142174, -272.5094457136060555, -194.2889575220754068 ) ) ;
#16754 = AXIS2_PLACEMENT_3D ( 'NONE', #10130, #59890, #83025 ) ;
#16755 = CARTESIAN_POINT ( 'NONE',  ( -105.7611832317066671, -280.9612874902786075, -239.1101099601321778 ) ) ;
#16756 = CARTESIAN_POINT ( 'NONE',  ( 195.2310442527411567, 19.79200657291019283, 13.55662862596270557 ) ) ;
#16757 = CARTESIAN_POINT ( 'NONE',  ( -33.81938370745150024, -288.0163015749246256, -194.8832570773436430 ) ) ;
#16758 = CARTESIAN_POINT ( 'NONE',  ( -43.18343439339132317, -296.0521521680024080, -430.6442049081568939 ) ) ;
#16759 = CARTESIAN_POINT ( 'NONE',  ( -68.88567014012960499, -287.4666953059623893, -338.4189669717387687 ) ) ;
#16760 = FACE_OUTER_BOUND ( 'NONE', #43472, .T. ) ;
#16761 = CARTESIAN_POINT ( 'NONE',  ( -99.07554989433847936, -294.7995410783873922, -310.1539037320321768 ) ) ;
#16762 = CARTESIAN_POINT ( 'NONE',  ( -95.07968986657911614, -288.0427851802686519, -317.0214868709439884 ) ) ;
#16763 = CARTESIAN_POINT ( 'NONE',  ( 202.9739649223127742, 291.4636489454787807, -68.19743562414970484 ) ) ;
#16764 = CARTESIAN_POINT ( 'NONE',  ( 129.8483263487583201, -299.5541904835127980, -189.0224624687345454 ) ) ;
#16765 = CARTESIAN_POINT ( 'NONE',  ( 37.34888832384107360, -285.8340964401198221, -254.6765161786775877 ) ) ;
#16766 = CARTESIAN_POINT ( 'NONE',  ( -76.25843857654081148, -281.8042925996973054, -335.6866834723716124 ) ) ;
#16767 = CARTESIAN_POINT ( 'NONE',  ( -41.59283723867329741, -291.9972612993083771, -197.4351586069549569 ) ) ;
#16768 = CARTESIAN_POINT ( 'NONE',  ( -2.889172598860140884, -281.9421060549499316, -205.3206921130092724 ) ) ;
#16769 = CARTESIAN_POINT ( 'NONE',  ( 34.10030408254412038, -282.5625386368658951, -286.1294965268039618 ) ) ;
#16770 = CARTESIAN_POINT ( 'NONE',  ( -98.51985169744814641, -291.9358739821950053, -314.3791311382445315 ) ) ;
#16771 = CARTESIAN_POINT ( 'NONE',  ( -57.39176424503054363, -297.9671267714110741, -195.9620771260187837 ) ) ;
#16772 = CARTESIAN_POINT ( 'NONE',  ( 13.61422578358280866, -286.4253054320082015, -326.2245411479219683 ) ) ;
#16773 = CARTESIAN_POINT ( 'NONE',  ( 37.90567700378380778, -275.7572143237819091, -286.7577216399399163 ) ) ;
#16774 = CARTESIAN_POINT ( 'NONE',  ( 19.71796841307034498, -294.8633254982221388, -222.2358540173663641 ) ) ;
#16775 = CARTESIAN_POINT ( 'NONE',  ( 165.2494399300530290, 8.542400036368780647, 25.74970488511327815 ) ) ;
#16776 = CARTESIAN_POINT ( 'NONE',  ( -95.99890600148557951, -287.6948066931273615, -223.6242672951989618 ) ) ;
#16777 = CARTESIAN_POINT ( 'NONE',  ( -39.92605506531148052, -275.0843633310311134, -345.4961034227234222 ) ) ;
#16778 = DIRECTION ( 'NONE',  ( 0.000000000000000000, 0.000000000000000000, 1.000000000000000000 ) ) ;
#16779 = CARTESIAN_POINT ( 'NONE',  ( -100.8713423401653984, -295.5116062250157256, -228.2609491121374958 ) ) ;
#16780 = CARTESIAN_POINT ( 'NONE',  ( -91.35848012726836487, -292.8676168670893958, -220.0569634975500719 ) ) ;
#16781 = CARTESIAN_POINT ( 'NONE',  ( -68.31823121472450566, -272.9828026897678797, -204.1329984060267293 ) ) ;
#16782 = CARTESIAN_POINT ( 'NONE',  ( -77.65042997564236771, -293.0202398442989420, -208.6690273261512800 ) ) ;
#16783 = CARTESIAN_POINT ( 'NONE',  ( -72.75119327194146024, -292.5125589461138702, -206.1981504475794509 ) ) ;
#16784 = CARTESIAN_POINT ( 'NONE',  ( -111.0052614399945696, -286.4124124059106862, -262.6666796976148817 ) ) ;
#16785 = CARTESIAN_POINT ( 'NONE',  ( 31.64610811718649686, -294.5516605770150704, -237.3856881399447616 ) ) ;
#16786 = CARTESIAN_POINT ( 'NONE',  ( -14.03273931990282541, -293.6633895292018792, -197.4358232659970724 ) ) ;
#16787 = CARTESIAN_POINT ( 'NONE',  ( -5.543426997267379086, -294.4551595132879811, -336.0854284948061945 ) ) ;
#16788 = CARTESIAN_POINT ( 'NONE',  ( 12.44313600156455202, -288.7453289588218581, -214.1979508259490501 ) ) ;
#16789 = CARTESIAN_POINT ( 'NONE',  ( 39.52931511702630729, -281.7850864424011661, -275.6587838214941826 ) ) ;
#16790 = CARTESIAN_POINT ( 'NONE',  ( -86.50640122769459595, -295.4557300401680209, -212.9149341202095513 ) ) ;
#16791 = CARTESIAN_POINT ( 'NONE',  ( -109.9765517385676219, -284.7078811437680770, -244.8037641285303323 ) ) ;
#16792 = CARTESIAN_POINT ( 'NONE',  ( -8.070970862483065389, -278.6467689774736982, -339.0413441852196570 ) ) ;
#16793 = EDGE_CURVE ( 'NONE', #82488, #77986, #33410, .T. ) ;
#16794 = CARTESIAN_POINT ( 'NONE',  ( -102.5843778676272962, -283.8016949323858853, -236.7378595884887602 ) ) ;
#16795 = CARTESIAN_POINT ( 'NONE',  ( 11.10403059602818487, -286.3811501681469736, -327.6150420434058788 ) ) ;
#16796 = CARTESIAN_POINT ( 'NONE',  ( -96.71393925998886232, -277.3318724533035606, -223.2947530770346702 ) ) ;
#16797 = CARTESIAN_POINT ( 'NONE',  ( 184.7149167944524493, 8.542400036368780647, 9.000000000000001776 ) ) ;
#16798 = CARTESIAN_POINT ( 'NONE',  ( -80.66766575671326223, -283.1651613856255949, -329.2530483675810729 ) ) ;
#16799 = CARTESIAN_POINT ( 'NONE',  ( -14.36157602354539797, -281.5485847477190191, -197.2307357035033704 ) ) ;
#16800 = CARTESIAN_POINT ( 'NONE',  ( 38.74365601144216953, -286.4830707033471526, -260.1709857979043932 ) ) ;
#16801 = CARTESIAN_POINT ( 'NONE',  ( -41.06812608781837781, -296.8598007078484784, -344.2933279348607698 ) ) ;
#16802 = CARTESIAN_POINT ( 'NONE',  ( -31.49114240818673238, -278.5797074884438871, -346.3882651543132170 ) ) ;
#16803 = CARTESIAN_POINT ( 'NONE',  ( 20.45874714393577065, -277.5491765082449547, -320.5048635039091209 ) ) ;
#16804 = CARTESIAN_POINT ( 'NONE',  ( -105.2685743126416469, -278.0278963736250262, -297.0994755986157543 ) ) ;
#16805 = CARTESIAN_POINT ( 'NONE',  ( -111.8320046657852771, -274.6035893181807523, -264.8158203631756464 ) ) ;
#16806 = CARTESIAN_POINT ( 'NONE',  ( 5.802637724076443959, -284.6378285760636686, -209.1536450596883583 ) ) ;
#16807 = CARTESIAN_POINT ( 'NONE',  ( -69.00608872204273325, -291.0617430368794203, -339.6848905027318324 ) ) ;
#16808 = CARTESIAN_POINT ( 'NONE',  ( 30.86814163362985042, -292.8318591819682979, -297.3633658816049774 ) ) ;
#16809 = EDGE_LOOP ( 'NONE', ( #41523, #65504, #55717, #80992 ) ) ;
#16810 = CARTESIAN_POINT ( 'NONE',  ( 21.34092943668413866, -293.8279985027817247, -313.8172622455487613 ) ) ;
#16811 = ORIENTED_EDGE ( 'NONE', *, *, #41200, .T. ) ;
#16812 = CARTESIAN_POINT ( 'NONE',  ( -89.27203257531260761, -290.8426749485843743, -326.7945573688728018 ) ) ;
#16813 = CARTESIAN_POINT ( 'NONE',  ( -95.69812702311496366, -279.8213889121909688, -226.3128444855985606 ) ) ;
#16814 = CARTESIAN_POINT ( 'NONE',  ( -62.72970323182380525, -296.6496020223606251, -197.9944004408036164 ) ) ;
#16815 = CARTESIAN_POINT ( 'NONE',  ( 38.68353979674457577, -288.0577860275657258, -258.7203405092957951 ) ) ;
#16816 = EDGE_CURVE ( 'NONE', #18158, #59842, #42574, .T. ) ;
#16817 = CARTESIAN_POINT ( 'NONE',  ( -4.338279829644617003, -288.9622630877383358, -339.9206767323568670 ) ) ;
#16818 = CARTESIAN_POINT ( 'NONE',  ( -80.63526020985034393, -283.9906568960454933, -329.2267048159183673 ) ) ;
#16819 = CARTESIAN_POINT ( 'NONE',  ( 167.6033460894835514, 232.7025357865791761, -192.5994064317780499 ) ) ;
#16820 = CARTESIAN_POINT ( 'NONE',  ( -40.96029181214492354, -138.9527141626594471, -363.1313459277565698 ) ) ;
#16821 = CARTESIAN_POINT ( 'NONE',  ( 25.13358130842753013, -23.89985919551285320, -341.3865608528514031 ) ) ;
#16822 = VECTOR ( 'NONE', #52194, 1000.000000000000000 ) ;
#16823 = CARTESIAN_POINT ( 'NONE',  ( -7.451012908818240632, -275.8470437144422931, -337.1379743399647282 ) ) ;
#16824 = CARTESIAN_POINT ( 'NONE',  ( -108.7906236507094206, -277.2561894567026002, -286.8264685628327015 ) ) ;
#16825 = CARTESIAN_POINT ( 'NONE',  ( -63.54590728247134734, -273.3864835554318802, -197.9796022558082882 ) ) ;
#16826 = CARTESIAN_POINT ( 'NONE',  ( 203.9605994126933695, 292.2036918473053220, -68.32866313698069405 ) ) ;
#16827 = CARTESIAN_POINT ( 'NONE',  ( -38.55404822206283910, -275.7518882384251810, -346.8583629442123311 ) ) ;
#16828 = CARTESIAN_POINT ( 'NONE',  ( -80.43875371432221755, -290.1461233899415788, -329.4209539967401383 ) ) ;
#16829 = CARTESIAN_POINT ( 'NONE',  ( -35.48704261382476943, -298.8776464955855658, -193.5223475898178549 ) ) ;
#16830 = CARTESIAN_POINT ( 'NONE',  ( 34.48912959104492160, -286.4413584485577076, -285.9627722571166828 ) ) ;
#16831 = CARTESIAN_POINT ( 'NONE',  ( 99.04417061415693979, -300.2092272999767033, -193.4114905176868149 ) ) ;
#16832 = CARTESIAN_POINT ( 'NONE',  ( -110.0505154012976163, -296.8119577760729726, -263.3017666189052193 ) ) ;
#16833 = VERTEX_POINT ( 'NONE', #62309 ) ;
#16834 = CARTESIAN_POINT ( 'NONE',  ( 198.6353741166566920, 66.99406408877143804, -8.405752120499668578 ) ) ;
#16835 = CARTESIAN_POINT ( 'NONE',  ( -53.79344272909299463, -279.1817131675209680, -344.1619658531067216 ) ) ;
#16836 = ADVANCED_FACE ( 'NONE', ( #48073 ), #84065, .F. ) ;
#16837 = CARTESIAN_POINT ( 'NONE',  ( -1.668243368071833821, -282.0998355195338831, -338.5295225861873405 ) ) ;
#16838 = CARTESIAN_POINT ( 'NONE',  ( -108.7844176582288327, -279.4151824684268490, -286.8533776154830548 ) ) ;
#16839 = CARTESIAN_POINT ( 'NONE',  ( -95.36076508472488911, -279.6421329664875657, -319.4501461133698967 ) ) ;
#16840 = CARTESIAN_POINT ( 'NONE',  ( -94.05615359452258417, -295.7865274240317035, -223.4496692724162870 ) ) ;
#16841 = CARTESIAN_POINT ( 'NONE',  ( 159.4851178187871312, 15.00000000000000000, -10.00000000000000000 ) ) ;
#16842 = CARTESIAN_POINT ( 'NONE',  ( -70.94355735715795674, -279.7625603924687425, -205.5402776106506622 ) ) ;
#16843 = CARTESIAN_POINT ( 'NONE',  ( -93.06212646645815312, -274.0797348978318269, -217.4326247039715270 ) ) ;
#16844 = CARTESIAN_POINT ( 'NONE',  ( -99.56392702124611560, -275.1197216753007524, -228.3950538420398004 ) ) ;
#16845 = CARTESIAN_POINT ( 'NONE',  ( 39.03359027425954508, -274.1731683567476807, -274.0338826733132578 ) ) ;
#16846 = ORIENTED_EDGE ( 'NONE', *, *, #91011, .T. ) ;
#16847 = CARTESIAN_POINT ( 'NONE',  ( 196.5738014817347334, 41.11195847892594202, 11.18394375856346556 ) ) ;
#16848 = CARTESIAN_POINT ( 'NONE',  ( -20.02404909225396779, -291.4774799949723274, -199.2263798403705266 ) ) ;
#16849 = EDGE_CURVE ( 'NONE', #70876, #81433, #33514, .T. ) ;
#16850 = CARTESIAN_POINT ( 'NONE',  ( -114.2387934545425736, -283.9055874384102935, -269.9740466585116110 ) ) ;
#16851 = CARTESIAN_POINT ( 'NONE',  ( 36.14312662533373555, -279.9123008192329962, -279.6067568330414019 ) ) ;
#16853 = CARTESIAN_POINT ( 'NONE',  ( -65.61799331073812880, -283.7594678311130565, -201.4457799542879286 ) ) ;
#16852 = CARTESIAN_POINT ( 'NONE',  ( 27.36459976079593659, -280.6012912615097434, -305.4106496532297683 ) ) ;
#16854 = CARTESIAN_POINT ( 'NONE',  ( -84.11119433614436502, -291.6947761890994002, -329.0579476218634909 ) ) ;
#16855 = CARTESIAN_POINT ( 'NONE',  ( 34.95558081160879027, -282.5911506183376218, -257.7027739279262732 ) ) ;
#16856 = CARTESIAN_POINT ( 'NONE',  ( -106.2301241842228308, -270.9413509115434522, -240.5754438293160149 ) ) ;
#16857 = CARTESIAN_POINT ( 'NONE',  ( -55.53116528385956485, -281.6823283391320842, -344.3583055693906658 ) ) ;
#16858 = CARTESIAN_POINT ( 'NONE',  ( 36.11698851220483419, -295.7465373086176328, -285.4879721039424680 ) ) ;
#16859 = CARTESIAN_POINT ( 'NONE',  ( -108.6474046387803440, -277.1300437811896700, -243.9515604728954656 ) ) ;
#16860 = CARTESIAN_POINT ( 'NONE',  ( -109.1418353169747064, -279.0217701751894310, -284.1616016910651297 ) ) ;
#16861 = CARTESIAN_POINT ( 'NONE',  ( -106.2557460714628661, -286.9457713853567498, -240.2161653820762695 ) ) ;
#16862 = CARTESIAN_POINT ( 'NONE',  ( 199.4767649826798674, 24.99747890858082044, 8.999999999999998224 ) ) ;
#16863 = CARTESIAN_POINT ( 'NONE',  ( -40.59535378736537581, -293.9317136983653427, -194.8582630164650880 ) ) ;
#16864 = CARTESIAN_POINT ( 'NONE',  ( 35.83930168603148303, -273.7635456023746201, -286.8371525849747741 ) ) ;
#16865 = CARTESIAN_POINT ( 'NONE',  ( -37.51151711632554253, -288.2513631695539971, -347.2124989055708397 ) ) ;
#16866 = CARTESIAN_POINT ( 'NONE',  ( -19.86314770634546534, -290.6803124781857832, -198.6079194367765695 ) ) ;
#16867 = CARTESIAN_POINT ( 'NONE',  ( -43.29218995563469718, -273.4472827993805595, -431.9929295280254564 ) ) ;
#16868 = CARTESIAN_POINT ( 'NONE',  ( -56.74639997845254413, -275.9923087602757619, -341.2991004499526753 ) ) ;
#16869 = CARTESIAN_POINT ( 'NONE',  ( -98.20951097852338307, -294.1090690068904792, -312.8578835477728717 ) ) ;
#16870 = CARTESIAN_POINT ( 'NONE',  ( -87.05069338917586208, -291.0766277584838235, -324.5620117508524913 ) ) ;
#16871 = CARTESIAN_POINT ( 'NONE',  ( 201.2104617360081704, 15.00000000000000000, 9.000000000000001776 ) ) ;
#16872 = FACE_OUTER_BOUND ( 'NONE', #14287, .T. ) ;
#16873 = CARTESIAN_POINT ( 'NONE',  ( 34.82432513934203655, -292.3492107278763683, -295.3175258151670732 ) ) ;
#16874 = CARTESIAN_POINT ( 'NONE',  ( -4.253955750511765110, -288.0960080642899470, -204.3941445083287078 ) ) ;
#16875 = CARTESIAN_POINT ( 'NONE',  ( 20.70030373011753255, -286.4615711264362972, -319.4029348769312264 ) ) ;
#16876 = CARTESIAN_POINT ( 'NONE',  ( -46.81859243323795994, -287.3548901905036246, -197.3334738958409105 ) ) ;
#16877 = DIRECTION ( 'NONE',  ( 0.000000000000000000, 0.000000000000000000, 1.000000000000000000 ) ) ;
#16878 = CARTESIAN_POINT ( 'NONE',  ( 34.15162943915060367, -288.1505195896593250, -254.8271051424618179 ) ) ;
#16879 = CARTESIAN_POINT ( 'NONE',  ( -27.92776968259137504, -296.9132276242093553, -345.1781358930899728 ) ) ;
#16880 = LINE ( 'NONE', #44817, #38249 ) ;
#16881 = CARTESIAN_POINT ( 'NONE',  ( 18.05369029194578445, -288.0292381278296716, -217.3756621137121385 ) ) ;
#16882 = CARTESIAN_POINT ( 'NONE',  ( -98.49891727662877372, -276.0318235976262713, -314.7577717115177052 ) ) ;
#16883 = CIRCLE ( 'NONE', #15403, 4.003189038634634045 ) ;
#16884 = CARTESIAN_POINT ( 'NONE',  ( -20.12670252300265261, -277.1702008765964251, -345.4450711649213304 ) ) ;
#16885 = VECTOR ( 'NONE', #65285, 1000.000000000000000 ) ;
#16886 = CARTESIAN_POINT ( 'NONE',  ( -38.16542169287795616, -279.7088143624405348, -193.3866691411668057 ) ) ;
#16887 = CARTESIAN_POINT ( 'NONE',  ( -109.4305729840638719, -298.7827682100736411, -250.9458196565193475 ) ) ;
#16888 = CARTESIAN_POINT ( 'NONE',  ( -38.63451889773383385, -284.0358156024701657, -195.3594330193917017 ) ) ;
#16889 = CARTESIAN_POINT ( 'NONE',  ( -147.8070425842520308, 32.24468615100210656, -21.49999999999998579 ) ) ;
#16890 = CARTESIAN_POINT ( 'NONE',  ( -86.28100845742068259, -277.5039957914335673, -214.5416807046806582 ) ) ;
#16891 = CARTESIAN_POINT ( 'NONE',  ( -94.75614194888153463, -281.8847434534070544, -318.6363861277664000 ) ) ;
#16892 = CYLINDRICAL_SURFACE ( 'NONE', #3355, 1.000000000000000888 ) ;
#16893 = CARTESIAN_POINT ( 'NONE',  ( 35.39582863089869846, -274.3245680970852050, -293.4253687317366825 ) ) ;
#16894 = AXIS2_PLACEMENT_3D ( 'NONE', #14111, #43433, #70477 ) ;
#16895 = CARTESIAN_POINT ( 'NONE',  ( -110.9330423195532802, -298.0216338201580584, -274.2369540547595648 ) ) ;
#16896 = CARTESIAN_POINT ( 'NONE',  ( 9.011003509519834864, -281.3529022378045283, -331.4587396578206722 ) ) ;
#16897 = CARTESIAN_POINT ( 'NONE',  ( -108.7090245018078605, -297.7095169347002184, -253.9259891209473210 ) ) ;
#16898 = CARTESIAN_POINT ( 'NONE',  ( -30.55593340486651499, -299.4506030025160044, -193.8527844494389853 ) ) ;
#16899 = CARTESIAN_POINT ( 'NONE',  ( 7.347200606675306389, -274.3476551295489116, -212.6117488275851883 ) ) ;
#16900 = CARTESIAN_POINT ( 'NONE',  ( -8.994538752723119757, -294.4228991626841321, -200.8692857695782834 ) ) ;
#16901 = CARTESIAN_POINT ( 'NONE',  ( 35.84836915531595025, -287.4159530325503624, -246.2696239121606823 ) ) ;
#16902 = CARTESIAN_POINT ( 'NONE',  ( -66.77848234817165007, -277.7493132929823787, -200.7709602571649725 ) ) ;
#16903 = CARTESIAN_POINT ( 'NONE',  ( -111.9940479367977133, -290.6221652319840132, -251.4393380131373306 ) ) ;
#16904 = ADVANCED_FACE ( 'NONE', ( #25374 ), #51681, .T. ) ;
#16905 = CARTESIAN_POINT ( 'NONE',  ( -37.27981480475732212, -288.1101049069158648, -343.5963869393783057 ) ) ;
#16906 = CARTESIAN_POINT ( 'NONE',  ( 36.10666853762655393, -291.7468634865115291, -285.5380014803782842 ) ) ;
#16907 = ORIENTED_EDGE ( 'NONE', *, *, #19092, .T. ) ;
#16908 = CARTESIAN_POINT ( 'NONE',  ( 191.4749582765727212, -21.37379927922774314, 10.00000000000000000 ) ) ;
#16909 = CARTESIAN_POINT ( 'NONE',  ( -83.86340288714998792, -290.9005038762270487, -214.0253423701204269 ) ) ;
#16910 = DIRECTION ( 'NONE',  ( 1.000000000000000000, 0.000000000000000000, 0.000000000000000000 ) ) ;
#16911 = CARTESIAN_POINT ( 'NONE',  ( -114.0918971416658962, -285.5338572645170530, -267.1362844392434113 ) ) ;
#16912 = CARTESIAN_POINT ( 'NONE',  ( 15.28560599361442485, -291.8322407444836131, -214.4026413756341185 ) ) ;
#16913 = CARTESIAN_POINT ( 'NONE',  ( -21.80963834105200050, -284.1722620795108014, -345.2747571151184047 ) ) ;
#16914 = CARTESIAN_POINT ( 'NONE',  ( 5.590377952295035868, -282.2854313356813805, -329.4020925357089027 ) ) ;
#16915 = CARTESIAN_POINT ( 'NONE',  ( -73.28062652725911619, -297.5893465982373982, -202.2038613488620911 ) ) ;
#16916 = CARTESIAN_POINT ( 'NONE',  ( 7.619485114162730000, -275.9958450415558673, -212.2256271169063098 ) ) ;
#16917 = CARTESIAN_POINT ( 'NONE',  ( -52.68374753490112994, -289.8748662645199374, -197.2569162825540730 ) ) ;
#16918 = CARTESIAN_POINT ( 'NONE',  ( -0.3328679173530076918, -273.3509390518309488, -206.9628769600639941 ) ) ;
#16919 = ORIENTED_EDGE ( 'NONE', *, *, #31936, .T. ) ;
#16920 = DIRECTION ( 'NONE',  ( 1.110223024625156343E-15, 0.000000000000000000, 1.000000000000000000 ) ) ;
#16921 = CARTESIAN_POINT ( 'NONE',  ( -27.67326489559168223, -288.0960660726323681, -196.5516635986635947 ) ) ;
#16922 = CARTESIAN_POINT ( 'NONE',  ( -112.8969232000900007, -297.4629437503029976, -283.8100765555144562 ) ) ;
#16923 = CARTESIAN_POINT ( 'NONE',  ( -110.1966776930315461, -285.1244803057439867, -276.3648594812455599 ) ) ;
#16924 = CARTESIAN_POINT ( 'NONE',  ( -109.5196416438047891, -277.2780177737372469, -296.6541101900322133 ) ) ;
#16925 = CARTESIAN_POINT ( 'NONE',  ( 38.71695036450618232, -294.3454622809013586, -281.6922464279305700 ) ) ;
#16926 = CARTESIAN_POINT ( 'NONE',  ( 38.11510842493029827, -285.7784793148747440, -277.1857441102209236 ) ) ;
#16927 = CARTESIAN_POINT ( 'NONE',  ( 22.27295568578142237, -294.5395298214356217, -319.0833229039461116 ) ) ;
#16928 = CARTESIAN_POINT ( 'NONE',  ( -104.7242202130908453, -291.2643261286660277, -242.0926473140400788 ) ) ;
#16929 = DIRECTION ( 'NONE',  ( 0.9951408606192334583, 0.000000000000000000, -0.09846150276129006507 ) ) ;
#16930 = DIRECTION ( 'NONE',  ( 0.000000000000000000, -0.000000000000000000, -1.000000000000000000 ) ) ;
#16931 = CARTESIAN_POINT ( 'NONE',  ( 138.9826652911064855, 178.1392901162842577, -238.3061235048771778 ) ) ;
#16932 = CARTESIAN_POINT ( 'NONE',  ( -108.3900794218999692, -286.4299457453257673, -242.3814567359070509 ) ) ;
#16933 = CARTESIAN_POINT ( 'NONE',  ( 13.84574458161073807, -278.1952119285919025, -206.2264541496106460 ) ) ;
#16934 = EDGE_LOOP ( 'NONE', ( #71702, #31600, #15810, #82519 ) ) ;
#16935 = CARTESIAN_POINT ( 'NONE',  ( -71.56532022638916146, -282.4358446507671374, -335.1914342064756624 ) ) ;
#16936 = CARTESIAN_POINT ( 'NONE',  ( -100.4506040249524261, -277.6360247024985597, -314.4407112256638470 ) ) ;
#16937 = CARTESIAN_POINT ( 'NONE',  ( 14.58947640107679078, -282.7847647473660686, -216.4077518846299881 ) ) ;
#16938 = CARTESIAN_POINT ( 'NONE',  ( -28.98919269380465735, -125.6596419279838699, -362.8013170975748949 ) ) ;
#16939 = CARTESIAN_POINT ( 'NONE',  ( -8.279932611388820973, -281.2538601208498221, -341.0855979981232053 ) ) ;
#16940 = CARTESIAN_POINT ( 'NONE',  ( 21.65582614244480553, -284.9424047584124082, -224.6321479469126245 ) ) ;
#16941 = CARTESIAN_POINT ( 'NONE',  ( -24.39437530483978733, -276.0760082679493053, -195.6574900559521382 ) ) ;
#16942 = CARTESIAN_POINT ( 'NONE',  ( -34.29235569821962315, -295.5051301439532381, -343.3589942553924743 ) ) ;
#16943 = CARTESIAN_POINT ( 'NONE',  ( 19.73933626591457369, -291.5862391993420601, -224.0486734630941328 ) ) ;
#16944 = CARTESIAN_POINT ( 'NONE',  ( -113.1972525816878345, -279.0455311966885006, -282.9804661692281798 ) ) ;
#16945 = CARTESIAN_POINT ( 'NONE',  ( -1.470229989576658847, -276.5627249245064263, -333.9969134662892429 ) ) ;
#16946 = CARTESIAN_POINT ( 'NONE',  ( 23.39648751719547803, -273.8448675966208157, -223.5170397119977963 ) ) ;
#16947 = CARTESIAN_POINT ( 'NONE',  ( 24.96937360118007021, -22.70870616268144815, -344.9910381550471925 ) ) ;
#16948 = CARTESIAN_POINT ( 'NONE',  ( -66.11645737103935971, -275.4285525426614640, -339.6353506295643001 ) ) ;
#16949 = CARTESIAN_POINT ( 'NONE',  ( -58.66931876783620226, -296.7478338671903657, -343.7902274546861463 ) ) ;
#16950 = CARTESIAN_POINT ( 'NONE',  ( 156.5440870305766055, 214.9910457053126720, 17.21343741151179429 ) ) ;
#16951 = AXIS2_PLACEMENT_3D ( 'NONE', #37573, #10094, #53666 ) ;
#16952 = DIRECTION ( 'NONE',  ( 1.000000000000000000, -0.000000000000000000, -0.000000000000000000 ) ) ;
#16953 = CIRCLE ( 'NONE', #71386, 0.5000000000000004441 ) ;
#16954 = CARTESIAN_POINT ( 'NONE',  ( -109.2801883229806776, -285.4464827773321076, -284.4706888701941807 ) ) ;
#16955 = CARTESIAN_POINT ( 'NONE',  ( -102.0433469577533856, -285.7845322712520328, -310.2067063202604800 ) ) ;
#16956 = CARTESIAN_POINT ( 'NONE',  ( 16.97190299059360896, -286.2009674662938892, -221.4146730290349012 ) ) ;
#16957 = CARTESIAN_POINT ( 'NONE',  ( -3.518778747445463928, -274.9977535096032852, -335.9541847371747849 ) ) ;
#16958 = CARTESIAN_POINT ( 'NONE',  ( 34.52517894979501278, -283.6546429237428697, -289.0133525352189281 ) ) ;
#16959 = CARTESIAN_POINT ( 'NONE',  ( -83.45555153473983978, -276.1771355168610853, -327.9091566341014641 ) ) ;
#16960 = CARTESIAN_POINT ( 'NONE',  ( -45.93072475215929273, -278.2431532691024927, -343.2161796017575170 ) ) ;
#16961 = DIRECTION ( 'NONE',  ( 0.000000000000000000, 0.000000000000000000, -1.000000000000000000 ) ) ;
#16962 = CIRCLE ( 'NONE', #45663, 1.000000000000009104 ) ;
#16963 = CARTESIAN_POINT ( 'NONE',  ( 39.24993377288539875, -282.2778480708300890, -264.2064095004320734 ) ) ;
#16964 = CARTESIAN_POINT ( 'NONE',  ( -11.53590649010932090, -280.8716521232119021, -197.8235441082313457 ) ) ;
#16965 = ORIENTED_EDGE ( 'NONE', *, *, #73478, .F. ) ;
#16966 = ORIENTED_EDGE ( 'NONE', *, *, #38034, .T. ) ;
#16967 = FACE_OUTER_BOUND ( 'NONE', #31728, .T. ) ;
#16968 = CARTESIAN_POINT ( 'NONE',  ( -13.12136136878560677, -288.2239406534709474, -198.5719776515869341 ) ) ;
#16969 = CARTESIAN_POINT ( 'NONE',  ( -55.32348060182023630, -297.0121430608490414, -199.3914370556261986 ) ) ;
#16970 = EDGE_CURVE ( 'NONE', #52528, #68989, #68235, .T. ) ;
#16971 = CARTESIAN_POINT ( 'NONE',  ( -66.96849824421387609, -291.0224863172368828, -199.3993985831009752 ) ) ;
#16972 = CARTESIAN_POINT ( 'NONE',  ( 32.94061699415235722, -285.7405323709311915, -248.1579772003571804 ) ) ;
#16974 = CARTESIAN_POINT ( 'NONE',  ( -25.22137191851076921, -290.4484896307543522, -197.2947342759682954 ) ) ;
#16973 = CARTESIAN_POINT ( 'NONE',  ( -13.11084249534434676, -287.3057883155887566, -339.8466593202759327 ) ) ;
#16975 = CARTESIAN_POINT ( 'NONE',  ( -73.76594619740265557, -286.7621236417540445, -206.6252358071488970 ) ) ;
#16976 = CARTESIAN_POINT ( 'NONE',  ( -70.70467126983730566, -275.4920321204199922, -337.5318914601073175 ) ) ;
#16977 = CARTESIAN_POINT ( 'NONE',  ( 34.31315527711925739, -286.2846074382899815, -296.4379081585745439 ) ) ;
#16978 = CARTESIAN_POINT ( 'NONE',  ( 32.97016659585824527, -289.2135120769601144, -244.2605041038906108 ) ) ;
#16979 = CARTESIAN_POINT ( 'NONE',  ( -100.7683000735515861, -288.0092793921699013, -310.7942131821229168 ) ) ;
#16980 = CARTESIAN_POINT ( 'NONE',  ( 34.17276622843636602, -282.7009356366545489, -286.1436890870045318 ) ) ;
#16981 = CARTESIAN_POINT ( 'NONE',  ( -111.3242141045046907, -292.3811216812559906, -283.7233813739512129 ) ) ;
#16982 = CARTESIAN_POINT ( 'NONE',  ( 82.12627345295348391, -301.3282310295588218, -194.4389801081340750 ) ) ;
#16983 = DIRECTION ( 'NONE',  ( -0.000000000000000000, -0.000000000000000000, 1.000000000000000000 ) ) ;
#16984 = CARTESIAN_POINT ( 'NONE',  ( -108.5030666233512591, -298.7990811821818511, -244.9569034656359747 ) ) ;
#16985 = CARTESIAN_POINT ( 'NONE',  ( -30.23654905568832874, -279.3413577191250852, -197.4950036532778768 ) ) ;
#16986 = CARTESIAN_POINT ( 'NONE',  ( 37.42051237654314377, -279.6366088439660871, -276.9515588317134416 ) ) ;
#16987 = CARTESIAN_POINT ( 'NONE',  ( 39.07534425039197856, -292.8561752934695619, -278.8871293087453864 ) ) ;
#16988 = CARTESIAN_POINT ( 'NONE',  ( -55.47068109827161919, -296.2149755502882158, -198.7695741559975886 ) ) ;
#16989 = CARTESIAN_POINT ( 'NONE',  ( 8.447282414967718367, -274.4999384803279554, -329.1182074055128055 ) ) ;
#16990 = CARTESIAN_POINT ( 'NONE',  ( -42.40710803614312852, -296.4325490641732017, -343.6794998601117186 ) ) ;
#16991 = CARTESIAN_POINT ( 'NONE',  ( 154.5816620007682047, 19.45641339818851279, 12.71868198592549781 ) ) ;
#16992 = CARTESIAN_POINT ( 'NONE',  ( -106.3035797775020939, -271.5520077986109868, -237.4541970312146475 ) ) ;
#16993 = CARTESIAN_POINT ( 'NONE',  ( -53.10126226642907454, -293.4912341868555359, -344.7493952095852023 ) ) ;
#16994 = CARTESIAN_POINT ( 'NONE',  ( 4.826547729575792367, -294.0591414711578864, -209.9893452760917683 ) ) ;
#16995 = CARTESIAN_POINT ( 'NONE',  ( 61.37083282337847123, -250.8548725835408391, -22.50000000000000000 ) ) ;
#16996 = CARTESIAN_POINT ( 'NONE',  ( -5.981666331252039726, -293.2780588215939588, -204.2477605534664633 ) ) ;
#16997 = FACE_OUTER_BOUND ( 'NONE', #53513, .T. ) ;
#16999 = CARTESIAN_POINT ( 'NONE',  ( -31.60235537226621716, -294.9778227182930550, -343.1852644781941422 ) ) ;
#16998 = CARTESIAN_POINT ( 'NONE',  ( -112.6958619816320777, -282.5773222533448461, -269.9647708052559665 ) ) ;
#17000 = CARTESIAN_POINT ( 'NONE',  ( -41.56913770093522942, -283.1038741220709767, -347.2973100054052793 ) ) ;
#17001 = CARTESIAN_POINT ( 'NONE',  ( 37.74880882459412135, -283.3592998368132498, -261.4942062133706600 ) ) ;
#17002 = CARTESIAN_POINT ( 'NONE',  ( -3.494824020551794419, -286.1534599689020411, -201.2080857129227809 ) ) ;
#17003 = CARTESIAN_POINT ( 'NONE',  ( -109.5134422913925221, -288.8069350189473425, -250.5806209750258233 ) ) ;
#17004 = CARTESIAN_POINT ( 'NONE',  ( 6.510594546088531942, -280.9483687434054673, -332.8731700484629528 ) ) ;
#17005 = CARTESIAN_POINT ( 'NONE',  ( 20.74062453112327731, -285.6070153726224703, -225.3312718612742742 ) ) ;
#17006 = CARTESIAN_POINT ( 'NONE',  ( 38.67072726555026208, -286.3446736192034336, -260.1825428703251646 ) ) ;
#17007 = DIRECTION ( 'NONE',  ( 0.8620390091940267618, 0.000000000000000000, -0.5068419345592672931 ) ) ;
#17008 = CARTESIAN_POINT ( 'NONE',  ( -73.67874856097451186, -297.1432550405769462, -334.5955271957656123 ) ) ;
#17009 = CARTESIAN_POINT ( 'NONE',  ( -94.75596750805311785, -279.2898065592671628, -320.7814332830569128 ) ) ;
#17011 = CARTESIAN_POINT ( 'NONE',  ( -98.00880881844318537, -278.7842456769117234, -229.6315892427783751 ) ) ;
#17010 = CARTESIAN_POINT ( 'NONE',  ( 35.85614590610301633, -291.8017124174068613, -288.3170494176977741 ) ) ;
#17012 = CARTESIAN_POINT ( 'NONE',  ( 24.81319831579656210, -293.1153996583991557, -224.9103907721864459 ) ) ;
#17013 = CARTESIAN_POINT ( 'NONE',  ( -57.35062240519914667, -283.8758860046265227, -197.4442149746326436 ) ) ;
#17014 = CARTESIAN_POINT ( 'NONE',  ( -20.54848316024892085, -278.8368119783942802, -343.5101689620825596 ) ) ;
#17015 = CARTESIAN_POINT ( 'NONE',  ( -86.65723617984265559, -294.8168589714524046, -324.5033967625814171 ) ) ;
#17016 = CIRCLE ( 'NONE', #1944, 2.000000000000001776 ) ;
#17017 = CARTESIAN_POINT ( 'NONE',  ( -62.15860923440826014, -295.7292613177100975, -199.5859693065293925 ) ) ;
#17018 = ORIENTED_EDGE ( 'NONE', *, *, #20108, .F. ) ;
#17019 = CARTESIAN_POINT ( 'NONE',  ( 199.7648473163356186, 63.23516263142278859, -10.15923027031813675 ) ) ;
#17021 = CARTESIAN_POINT ( 'NONE',  ( 16.42706245153227584, -282.8001759990223150, -218.5111828052056069 ) ) ;
#17020 = AXIS2_PLACEMENT_3D ( 'NONE', #45280, #46225, #9785 ) ;
#17022 = CARTESIAN_POINT ( 'NONE',  ( -110.3034514814425933, -296.0094886284684321, -274.1783527068847661 ) ) ;
#17023 = CARTESIAN_POINT ( 'NONE',  ( 160.5350683151633291, 276.0000000000000568, 20.22542485937379908 ) ) ;
#17024 = CARTESIAN_POINT ( 'NONE',  ( 35.77081079830085031, -273.2666405000204009, -287.0812184334320705 ) ) ;
#17025 = CARTESIAN_POINT ( 'NONE',  ( 7.149834651440080791, -273.8380913146555145, -207.6486904937819702 ) ) ;
#17026 = EDGE_CURVE ( 'NONE', #55975, #12630, #24456, .T. ) ;
#17027 = VECTOR ( 'NONE', #15954, 1000.000000000000000 ) ;
#17028 = EDGE_CURVE ( 'NONE', #11793, #10254, #78948, .T. ) ;
#17029 = CARTESIAN_POINT ( 'NONE',  ( 37.53736984938573329, -288.6689337078706217, -254.5998794257499185 ) ) ;
#17030 = CARTESIAN_POINT ( 'NONE',  ( -21.13140423249311795, -288.6716417095884708, -341.5385463672683386 ) ) ;
#17031 = AXIS2_PLACEMENT_3D ( 'NONE', #6965, #37671, #45697 ) ;
#17032 = CARTESIAN_POINT ( 'NONE',  ( -16.74632019806061933, -281.8432034523698348, -199.6042237854304062 ) ) ;
#17033 = CARTESIAN_POINT ( 'NONE',  ( 9.714448960572047653, -300.4092151778905304, -196.3334390736784485 ) ) ;
#17034 = CARTESIAN_POINT ( 'NONE',  ( -34.28149324702157941, -278.8863664845567314, -197.0152557882587985 ) ) ;
#17035 = ORIENTED_EDGE ( 'NONE', *, *, #85914, .T. ) ;
#17036 = CARTESIAN_POINT ( 'NONE',  ( -40.43515626221180526, -297.6811161879879819, -193.3923310999386445 ) ) ;
#17037 = CARTESIAN_POINT ( 'NONE',  ( -70.89118457865664880, -293.5261031612056399, -203.9100360180572409 ) ) ;
#17038 = PLANE ( 'NONE',  #56694 ) ;
#17039 = CARTESIAN_POINT ( 'NONE',  ( -102.9332448087500751, -290.7668413008985908, -302.6355960454165483 ) ) ;
#17040 = CARTESIAN_POINT ( 'NONE',  ( 197.4232884941380632, 67.42303550333971884, 10.33355363093519408 ) ) ;
#17041 = CARTESIAN_POINT ( 'NONE',  ( -34.97487675231187154, -290.2211375274265492, -194.6203530960704882 ) ) ;
#17042 = CARTESIAN_POINT ( 'NONE',  ( -94.46520784620715006, -296.8610407036135257, -224.8749403803518874 ) ) ;
#17043 = DIRECTION ( 'NONE',  ( 0.000000000000000000, 0.000000000000000000, 1.000000000000000000 ) ) ;
#17044 = CARTESIAN_POINT ( 'NONE',  ( -94.20765612706266268, -292.7686938366508684, -219.4791879710477929 ) ) ;
#17045 = CARTESIAN_POINT ( 'NONE',  ( -99.86837403722181250, -298.4090924074129703, -320.2651865833026363 ) ) ;
#17046 = CARTESIAN_POINT ( 'NONE',  ( 32.68129103810331060, -289.2069678638544588, -243.8178324011119855 ) ) ;
#17047 = CARTESIAN_POINT ( 'NONE',  ( 6.449504501896194952, -274.4559377987663993, -331.1075355486583476 ) ) ;
#17048 = CARTESIAN_POINT ( 'NONE',  ( 36.79023414869326558, -277.5598317763680143, -277.1265090728467158 ) ) ;
#17049 = CARTESIAN_POINT ( 'NONE',  ( -19.70779079199753525, -290.3603383001662337, -197.9865895230953470 ) ) ;
#17050 = CARTESIAN_POINT ( 'NONE',  ( -1.737187634855947405, -282.3792463229756322, -203.4834373066694297 ) ) ;
#17051 = CIRCLE ( 'NONE', #82062, 0.5000000000000016653 ) ;
#17052 = ORIENTED_EDGE ( 'NONE', *, *, #50609, .F. ) ;
#17053 = CARTESIAN_POINT ( 'NONE',  ( -1.208828318248188038, -281.9076789745990368, -333.9088027796296956 ) ) ;
#17054 = CARTESIAN_POINT ( 'NONE',  ( -104.5294228811511914, -280.1126735611623531, -233.3840653657056805 ) ) ;
#17055 = CARTESIAN_POINT ( 'NONE',  ( 30.71729914961442631, -280.8026177128979839, -305.5176441876676563 ) ) ;
#17056 = CARTESIAN_POINT ( 'NONE',  ( -20.16704954168087482, -277.7780738584860956, -345.2344634095481410 ) ) ;
#17057 = PRODUCT_CONTEXT ( 'NONE', #52342, 'mechanical' ) ;
#17058 = CARTESIAN_POINT ( 'NONE',  ( 22.20503976414471481, -276.4270353467877044, -222.6235991421189908 ) ) ;
#17059 = CARTESIAN_POINT ( 'NONE',  ( -21.33282851196159058, -279.3376638359844719, -340.3538533559490702 ) ) ;
#17060 = ORIENTED_EDGE ( 'NONE', *, *, #41512, .T. ) ;
#17061 = CARTESIAN_POINT ( 'NONE',  ( -112.3757206867542209, -298.5734697461911651, -268.7137049685347847 ) ) ;
#17062 = CARTESIAN_POINT ( 'NONE',  ( -100.5635952833257676, -291.1231957957028271, -307.5719586288238929 ) ) ;
#17063 = CARTESIAN_POINT ( 'NONE',  ( -62.40794291757152479, -291.1338337932824629, -342.1499922993866676 ) ) ;
#17064 = CARTESIAN_POINT ( 'NONE',  ( -37.54191246908424517, -291.3982018185155880, -197.2469975106114077 ) ) ;
#17065 = CARTESIAN_POINT ( 'NONE',  ( -9.591380266982669767, -288.2067576737762806, -342.1207629847342560 ) ) ;
#17066 = DIRECTION ( 'NONE',  ( 1.000000000000000000, -0.000000000000000000, -0.000000000000000000 ) ) ;
#17067 = CARTESIAN_POINT ( 'NONE',  ( -109.9768138420115662, -283.1233705359891815, -257.2294789445528522 ) ) ;
#17068 = CARTESIAN_POINT ( 'NONE',  ( -98.35075614819106704, -291.8328144825426875, -312.6771825152179076 ) ) ;
#17069 = CARTESIAN_POINT ( 'NONE',  ( -110.2958998249210509, -283.1680735061545988, -259.9499461383621224 ) ) ;
#17070 = CARTESIAN_POINT ( 'NONE',  ( -27.50886567974005459, -281.4947197331291022, -197.4771800675971463 ) ) ;
#17071 = CARTESIAN_POINT ( 'NONE',  ( 39.36982669833987103, -288.5440512768979033, -274.3985717569670442 ) ) ;
#17072 = CARTESIAN_POINT ( 'NONE',  ( -85.52946810435238945, -279.8563801938807956, -215.4436575628681965 ) ) ;
#17073 = CARTESIAN_POINT ( 'NONE',  ( -79.36370624807180718, -290.2937126527990017, -206.2496138276864315 ) ) ;
#17074 = CARTESIAN_POINT ( 'NONE',  ( 39.44349999278087893, -288.4056541474216147, -274.4042232703071136 ) ) ;
#17075 = CARTESIAN_POINT ( 'NONE',  ( 14.20099994950011357, -287.2454115821495293, -213.1680483020372776 ) ) ;
#17076 = CARTESIAN_POINT ( 'NONE',  ( -93.42070761499181231, -284.0556817035841277, -317.0959542807008802 ) ) ;
#17077 = ORIENTED_EDGE ( 'NONE', *, *, #25991, .F. ) ;
#17078 = DIRECTION ( 'NONE',  ( 0.000000000000000000, 0.000000000000000000, 1.000000000000000000 ) ) ;
#17079 = CARTESIAN_POINT ( 'NONE',  ( -35.02234885980617207, -293.9413678095104956, -194.6188838303984028 ) ) ;
#17080 = AXIS2_PLACEMENT_3D ( 'NONE', #35976, #49707, #71037 ) ;
#17081 = CARTESIAN_POINT ( 'NONE',  ( 24.47785268041048568, -292.8393481070178836, -315.4569098001047678 ) ) ;
#17082 = CARTESIAN_POINT ( 'NONE',  ( -21.61413719671539369, -275.9044262284627393, -341.9398599046951404 ) ) ;
#17083 = CARTESIAN_POINT ( 'NONE',  ( -113.0373125896367412, -296.0703745083641252, -256.8153791377112611 ) ) ;
#17084 = CARTESIAN_POINT ( 'NONE',  ( 22.37783350028307794, -291.4334531066760974, -227.1622849017408043 ) ) ;
#17085 = CARTESIAN_POINT ( 'NONE',  ( -65.94389949280636642, -295.9125459065321593, -202.0977441553750111 ) ) ;
#17086 = TOROIDAL_SURFACE ( 'NONE', #11056, 203.9779373800640485, 1.000000000000000000 ) ;
#17087 = CARTESIAN_POINT ( 'NONE',  ( -14.73861911021209536, -293.5567719355829013, -200.5311012799999446 ) ) ;
#17088 = CARTESIAN_POINT ( 'NONE',  ( 16.95792029340102047, -293.9283570217650663, -221.0345013277714372 ) ) ;
#17089 = CARTESIAN_POINT ( 'NONE',  ( 208.9648513981561564, 35.82080690278420576, 15.11414978972049106 ) ) ;
#17090 = CIRCLE ( 'NONE', #41249, 24.00000000000000355 ) ;
#17091 = CARTESIAN_POINT ( 'NONE',  ( -73.74143771664761005, -293.5336571068012859, -336.1848155651765637 ) ) ;
#17092 = CARTESIAN_POINT ( 'NONE',  ( -108.1383874600115860, -298.8746320690293601, -245.4521829112844387 ) ) ;
#17093 = CARTESIAN_POINT ( 'NONE',  ( 5.993473317834490999, -289.3895814077063164, -329.4622047780503067 ) ) ;
#17094 = CIRCLE ( 'NONE', #35213, 0.5000000000000004441 ) ;
#17095 = VECTOR ( 'NONE', #45170, 1000.000000000000114 ) ;
#17096 = CARTESIAN_POINT ( 'NONE',  ( -69.57408567824386125, -279.4541102137527560, -338.4889746555440979 ) ) ;
#17097 = CARTESIAN_POINT ( 'NONE',  ( -64.96627987024398010, -276.1999092687393045, -341.8656412701643603 ) ) ;
#17098 = CARTESIAN_POINT ( 'NONE',  ( -101.1193559776045845, -272.4685757678341247, -227.3044516608795220 ) ) ;
#17099 = CARTESIAN_POINT ( 'NONE',  ( 33.35169860706576372, -279.3265370003301769, -246.8798789812441328 ) ) ;
#17100 = CARTESIAN_POINT ( 'NONE',  ( -20.32479232698709737, -275.2371024213733222, -344.6908681440314695 ) ) ;
#17101 = AXIS2_PLACEMENT_3D ( 'NONE', #80411, #73786, #58660 ) ;
#17102 = CARTESIAN_POINT ( 'NONE',  ( -109.3713837463181164, -295.0449333588217087, -285.0172878133939776 ) ) ;
#17103 = CARTESIAN_POINT ( 'NONE',  ( 139.1539576904058606, 276.0000000000000568, 10.50000000000000000 ) ) ;
#17104 = CARTESIAN_POINT ( 'NONE',  ( -91.20324744867943423, -273.9120753011823695, -220.9176282906345818 ) ) ;
#17105 = FACE_OUTER_BOUND ( 'NONE', #78446, .T. ) ;
#17107 = CARTESIAN_POINT ( 'NONE',  ( 34.62601386784767499, -275.2231172221764268, -258.0537830887010387 ) ) ;
#17106 = CARTESIAN_POINT ( 'NONE',  ( -107.9241650482618553, -288.9150467175742847, -243.8208380544978411 ) ) ;
#17108 = AXIS2_PLACEMENT_3D ( 'NONE', #24442, #52854, #44357 ) ;
#17109 = CARTESIAN_POINT ( 'NONE',  ( 16.68595630013767206, -288.3094014086133825, -325.2988411975274516 ) ) ;
#17110 = CARTESIAN_POINT ( 'NONE',  ( -37.62728611644039489, -300.0284796732971699, -195.0064548997399356 ) ) ;
#17111 = CARTESIAN_POINT ( 'NONE',  ( -81.25057586038475677, -293.6504158035310184, -330.9584698689731681 ) ) ;
#17112 = CARTESIAN_POINT ( 'NONE',  ( -44.41455641505240948, -282.3365025426542161, -346.9266734630156179 ) ) ;
#17113 = DIRECTION ( 'NONE',  ( -0.000000000000000000, 1.000000000000000000, -0.000000000000000000 ) ) ;
#17114 = CARTESIAN_POINT ( 'NONE',  ( 31.98991793651351401, -279.1772270529588127, -241.6243364124823358 ) ) ;
#17115 = CIRCLE ( 'NONE', #51908, 24.00000000000000000 ) ;
#17116 = PLANE ( 'NONE',  #12022 ) ;
#17117 = CARTESIAN_POINT ( 'NONE',  ( -100.0428952900193735, -289.8697157148333190, -232.2076039955548481 ) ) ;
#17118 = CARTESIAN_POINT ( 'NONE',  ( -56.66282946885505112, -281.4434672721770880, -342.0378885477648510 ) ) ;
#17119 = DIRECTION ( 'NONE',  ( -0.000000000000000000, -1.000000000000000000, -0.000000000000000000 ) ) ;
#17120 = CARTESIAN_POINT ( 'NONE',  ( -110.9052975537900636, -288.3635819187505831, -285.0350590254873282 ) ) ;
#17121 = CARTESIAN_POINT ( 'NONE',  ( 22.02837887884630064, -276.4663330344525320, -226.7044864991603674 ) ) ;
#17122 = CARTESIAN_POINT ( 'NONE',  ( -1.804651291749928221, -283.7969840363227263, -338.2222031463684857 ) ) ;
#17124 = CARTESIAN_POINT ( 'NONE',  ( -82.79472189085720402, -283.6934346386124730, -327.5488571289008632 ) ) ;
#17123 = CARTESIAN_POINT ( 'NONE',  ( -69.49632849633245257, -271.7122004015988637, -201.9701224755656881 ) ) ;
#17125 = CARTESIAN_POINT ( 'NONE',  ( 33.42163236142050664, -276.7103670143191607, -249.9820284977034532 ) ) ;
#17126 = CARTESIAN_POINT ( 'NONE',  ( 32.67389097122043040, -276.6359001961558874, -291.6276374757095482 ) ) ;
#17127 = CARTESIAN_POINT ( 'NONE',  ( 23.50016623585100106, -284.1495149351130181, -314.2380068539533795 ) ) ;
#17128 = ORIENTED_EDGE ( 'NONE', *, *, #13516, .F. ) ;
#17129 = CARTESIAN_POINT ( 'NONE',  ( 160.5350683151633575, 275.5000000000000568, -11.99999999999998934 ) ) ;
#17130 = CARTESIAN_POINT ( 'NONE',  ( 6.612260534475175255, -294.3063269520496306, -333.6483068051148848 ) ) ;
#17131 = CARTESIAN_POINT ( 'NONE',  ( 35.30539193004074150, -289.3100312676060071, -253.1523306551676171 ) ) ;
#17132 = LINE ( 'NONE', #16205, #92672 ) ;
#17133 = CARTESIAN_POINT ( 'NONE',  ( -37.30987171927208834, -289.5523547857346784, -190.3611179825600175 ) ) ;
#17134 = CARTESIAN_POINT ( 'NONE',  ( -112.4934941197131479, -277.2797112481852082, -285.7133348417480079 ) ) ;
#17135 = EDGE_CURVE ( 'NONE', #77618, #3669, #65394, .T. ) ;
#17136 = CARTESIAN_POINT ( 'NONE',  ( -22.33122652777116812, -290.6410133030788074, -195.6004191284564797 ) ) ;
#17137 = CARTESIAN_POINT ( 'NONE',  ( -110.7851798487517812, -285.9930491389008580, -276.4243710502900626 ) ) ;
#17138 = CARTESIAN_POINT ( 'NONE',  ( -107.2135138095480897, -279.9901929397520348, -294.9275518852743971 ) ) ;
#17139 = CARTESIAN_POINT ( 'NONE',  ( -108.4865581322787449, -286.3351113479791366, -242.3421374403021957 ) ) ;
#17140 = CARTESIAN_POINT ( 'NONE',  ( -33.36539822217105922, -285.0022726118937726, -345.2685585424827082 ) ) ;
#17141 = CARTESIAN_POINT ( 'NONE',  ( 30.54406808840042942, -276.1897650093678749, -306.8126993175403072 ) ) ;
#17142 = CARTESIAN_POINT ( 'NONE',  ( -78.39603293036846310, -295.5172546557896567, -207.9581134579399304 ) ) ;
#17143 = CARTESIAN_POINT ( 'NONE',  ( -82.23713664484530739, -279.2914289285507721, -207.8039458561275126 ) ) ;
#17144 = CARTESIAN_POINT ( 'NONE',  ( -78.32478079314712716, -299.4166727202165248, -208.1565753724476338 ) ) ;
#17145 = CARTESIAN_POINT ( 'NONE',  ( 185.8445586754484964, 214.9970011440365454, 23.11617803653495784 ) ) ;
#17146 = PLANE ( 'NONE',  #66255 ) ;
#17147 = CARTESIAN_POINT ( 'NONE',  ( -113.3275340877688251, -270.8281558274566692, -267.5090283341868940 ) ) ;
#17149=STYLED_ITEM('',(#93738),#26626);
#17148 = DIRECTION ( 'NONE',  ( -0.000000000000000000, -0.000000000000000000, -1.000000000000000000 ) ) ;
#17150 = CARTESIAN_POINT ( 'NONE',  ( -27.01901063854439045, -276.4250050130776799, -342.6897466384641575 ) ) ;
#17151 = AXIS2_PLACEMENT_3D ( 'NONE', #8568, #60647, #53533 ) ;
#17152 = CARTESIAN_POINT ( 'NONE',  ( 15.74077815564904270, -275.9889201771181320, -215.1319661049836611 ) ) ;
#17153 = CARTESIAN_POINT ( 'NONE',  ( 26.09296876122256492, -280.0379483352124907, -227.0380001738530495 ) ) ;
#17154 = CARTESIAN_POINT ( 'NONE',  ( -0.4673932990832067036, -290.3154106884458088, -334.5937867421626493 ) ) ;
#17155 = CARTESIAN_POINT ( 'NONE',  ( -81.45496320822191194, -297.1599595502635793, -332.6890176643797759 ) ) ;
#17156 = CARTESIAN_POINT ( 'NONE',  ( -113.9685938274647015, -297.7306620818980605, -272.4742320110182163 ) ) ;
#17157 = CARTESIAN_POINT ( 'NONE',  ( 12.12404266986732360, -294.7417573551070404, -214.1389104939089520 ) ) ;
#17158 = CARTESIAN_POINT ( 'NONE',  ( 33.72551608239047027, -279.2465434817816572, -246.7566508464977915 ) ) ;
#17159 = AXIS2_PLACEMENT_3D ( 'NONE', #33889, #48068, #18270 ) ;
#17160 = CARTESIAN_POINT ( 'NONE',  ( 8.000459377986219422, -282.5970605639263340, -211.2586148898205067 ) ) ;
#17161 = CARTESIAN_POINT ( 'NONE',  ( -92.90373748404503829, -295.3267512501931265, -220.8214954148626816 ) ) ;
#17162 = CARTESIAN_POINT ( 'NONE',  ( -110.7155831740642782, -285.8919349505402465, -290.9211204937889761 ) ) ;
#17163 = CARTESIAN_POINT ( 'NONE',  ( 31.26874127271732462, -286.1276320056451823, -244.3946287249266049 ) ) ;
#17164 = CARTESIAN_POINT ( 'NONE',  ( 191.3253626393375839, 269.8902699472227482, -139.2695367922076741 ) ) ;
#17165 = VERTEX_POINT ( 'NONE', #83591 ) ;
#17166 = CARTESIAN_POINT ( 'NONE',  ( 32.32019631698473461, -286.5310452160484260, -301.7589917162479765 ) ) ;
#17167 = CARTESIAN_POINT ( 'NONE',  ( -8.242622313618772623, -286.1107520854085351, -203.3885030031145789 ) ) ;
#17168 = VERTEX_POINT ( 'NONE', #75571 ) ;
#17169 = CARTESIAN_POINT ( 'NONE',  ( -96.92351360873561816, -284.9813569728678431, -318.6673595311115150 ) ) ;
#17170 = CIRCLE ( 'NONE', #86710, 8.000000000000000000 ) ;
#17171 = CARTESIAN_POINT ( 'NONE',  ( 26.78735444693427326, -276.3632556239281257, -305.3889150724034494 ) ) ;
#17172 = CARTESIAN_POINT ( 'NONE',  ( -61.57780627145452712, -290.6649599033058848, -197.5445987055869637 ) ) ;
#17173 = CARTESIAN_POINT ( 'NONE',  ( 38.32675761814055448, -282.3760011066274842, -284.1309160592298895 ) ) ;
#17174 = DIRECTION ( 'NONE',  ( -1.000000000000000000, 0.000000000000000000, 0.000000000000000000 ) ) ;
#17175 = CARTESIAN_POINT ( 'NONE',  ( -98.88029927190306978, -280.6771413161891360, -225.2202311764013416 ) ) ;
#17176 = CARTESIAN_POINT ( 'NONE',  ( 37.30971162058846602, -281.6503181819015822, -251.5751919858336692 ) ) ;
#17177 = CARTESIAN_POINT ( 'NONE',  ( 21.27581636871891391, -273.6952119285918457, -317.1477375740089997 ) ) ;
#17178 = CARTESIAN_POINT ( 'NONE',  ( 190.4687118359351246, 271.0561473682616906, -139.6585402428168834 ) ) ;
#17179 = ORIENTED_EDGE ( 'NONE', *, *, #38393, .T. ) ;
#17180 = CARTESIAN_POINT ( 'NONE',  ( 20.61730575103503682, -278.2062920943478730, -317.7182191956979977 ) ) ;
#17181 = CARTESIAN_POINT ( 'NONE',  ( -48.94245970541811630, -154.4817453298226724, -364.6946769374113160 ) ) ;
#17182 = CIRCLE ( 'NONE', #42930, 9.103929867429224387 ) ;
#17183 = CARTESIAN_POINT ( 'NONE',  ( 8.164578208348435950, -278.6976418584205248, -211.1262394462077907 ) ) ;
#17184 = CARTESIAN_POINT ( 'NONE',  ( -44.57092174185743261, -297.3069882586909216, -197.5670679431429448 ) ) ;
#17185 = CARTESIAN_POINT ( 'NONE',  ( 19.47999444693757454, -293.7663245176897249, -322.3118442344506320 ) ) ;
#17186 = DIRECTION ( 'NONE',  ( -1.000000000000000000, 0.000000000000000000, 0.000000000000000000 ) ) ;
#17187 = EDGE_CURVE ( 'NONE', #39736, #93199, #5012, .T. ) ;
#17189 = CARTESIAN_POINT ( 'NONE',  ( -109.7273595455288699, -288.7635493391237560, -284.8048825290147192 ) ) ;
#17188 = CARTESIAN_POINT ( 'NONE',  ( -96.87575768589123015, -295.7738000571590078, -222.4622423559597735 ) ) ;
#17190 = CARTESIAN_POINT ( 'NONE',  ( -87.30410741372166683, -297.6180757882747798, -325.2667036394243496 ) ) ;
#17191 = CARTESIAN_POINT ( 'NONE',  ( -14.42804321940216816, -287.6705714765064954, -200.4778971785131603 ) ) ;
#17192 = ORIENTED_EDGE ( 'NONE', *, *, #38171, .T. ) ;
#17193 = CARTESIAN_POINT ( 'NONE',  ( 26.32332190230625457, -295.0602113281535708, -313.2515036511420021 ) ) ;
#17194 = CARTESIAN_POINT ( 'NONE',  ( -110.1565851648223600, -284.9654399085665659, -276.3595309915473877 ) ) ;
#17195 = CARTESIAN_POINT ( 'NONE',  ( -34.05265601491269933, -296.8874001566717880, -193.7588436825993483 ) ) ;
#17196 = CARTESIAN_POINT ( 'NONE',  ( -56.15915852686629961, -292.6186911709002061, -195.8075443401529583 ) ) ;
#17197 = CARTESIAN_POINT ( 'NONE',  ( -37.80095905698929926, -292.5388885756004242, -193.4240268963659730 ) ) ;
#17198 = CARTESIAN_POINT ( 'NONE',  ( -106.0318524081430525, -290.3897157999033425, -295.0727141316814368 ) ) ;
#17199 = ORIENTED_EDGE ( 'NONE', *, *, #78108, .F. ) ;
#17200 = CYLINDRICAL_SURFACE ( 'NONE', #59412, 4.000000000000003553 ) ;
#17201 = CARTESIAN_POINT ( 'NONE',  ( -96.39867958376001411, -299.0589563173783176, -222.8997793745646163 ) ) ;
#17202 = CARTESIAN_POINT ( 'NONE',  ( -34.10453689298036295, -272.8869472936946750, -193.8266192675493471 ) ) ;
#17203 = CARTESIAN_POINT ( 'NONE',  ( -21.34846707110369124, -281.9008480602296913, -341.8809463694336728 ) ) ;
#17204 = ORIENTED_EDGE ( 'NONE', *, *, #5180, .F. ) ;
#17205 = CARTESIAN_POINT ( 'NONE',  ( 1.010911956846083593, -276.0626131661437057, -337.1194019614455897 ) ) ;
#17206 = CARTESIAN_POINT ( 'NONE',  ( 52.75270939764214262, -297.6798444388553548, -196.6916333512348842 ) ) ;
#17207 = CARTESIAN_POINT ( 'NONE',  ( -103.2634827769061303, -280.8703711655966799, -236.1143822342512522 ) ) ;
#17208 = CARTESIAN_POINT ( 'NONE',  ( -3.322169788990462891, -274.7375080479140479, -336.3424565439934781 ) ) ;
#17209 = CARTESIAN_POINT ( 'NONE',  ( -108.8674280392905018, -297.9732979522711958, -253.8929440394740880 ) ) ;
#17210 = CARTESIAN_POINT ( 'NONE',  ( -31.33231338057652948, -275.0711317793014814, -197.3601017455594899 ) ) ;
#17211 = CARTESIAN_POINT ( 'NONE',  ( -97.61385962893201906, -298.7814247593959180, -223.7170187164452955 ) ) ;
#17212 = CARTESIAN_POINT ( 'NONE',  ( 25.57152109108438864, -273.0149701683577064, -228.8842159966131646 ) ) ;
#17213 = CARTESIAN_POINT ( 'NONE',  ( 18.54916894175702780, -293.5350613617497970, -223.2431445211967116 ) ) ;
#17214 = CARTESIAN_POINT ( 'NONE',  ( -9.487757388262888725, -290.9980194240793594, -202.1927760936629284 ) ) ;
#17215 = DIRECTION ( 'NONE',  ( 0.000000000000000000, -1.000000000000000000, 0.000000000000000000 ) ) ;
#17216 = CARTESIAN_POINT ( 'NONE',  ( 5.841927170023497595, -276.9759802325876308, -334.0376539787597494 ) ) ;
#17217 = CARTESIAN_POINT ( 'NONE',  ( -109.8860041760852653, -272.8262653978995900, -262.2171659512544011 ) ) ;
#17218 = CARTESIAN_POINT ( 'NONE',  ( -10.88836768577169956, -281.3993021718861200, -342.2054139834787634 ) ) ;
#17219 = CARTESIAN_POINT ( 'NONE',  ( -16.97846349042401570, -296.7901157069783835, -342.7708777124528297 ) ) ;
#17220 = DIRECTION ( 'NONE',  ( -0.000000000000000000, 1.000000000000000000, 0.000000000000000000 ) ) ;
#17221 = CARTESIAN_POINT ( 'NONE',  ( -92.68797249353914935, -283.0689085516376053, -318.2277759773480739 ) ) ;
#17222 = CARTESIAN_POINT ( 'NONE',  ( -108.4975852124747746, -282.2393248533763881, -294.5864857530026484 ) ) ;
#17223 = CARTESIAN_POINT ( 'NONE',  ( 25.79059335920872087, -273.6097927646864036, -232.4511574014176745 ) ) ;
#17224 = CARTESIAN_POINT ( 'NONE',  ( -26.53897922994619307, -282.1896313915731866, -196.0916231665542000 ) ) ;
#17225 = DIRECTION ( 'NONE',  ( -0.000000000000000000, -0.000000000000000000, -1.000000000000000000 ) ) ;
#17226 = DIRECTION ( 'NONE',  ( 0.000000000000000000, 0.000000000000000000, -1.000000000000000000 ) ) ;
#17227 = CARTESIAN_POINT ( 'NONE',  ( -91.58513040497733471, -271.6949018009564156, -216.8439180699880637 ) ) ;
#17228 = AXIS2_PLACEMENT_3D ( 'NONE', #67978, #76009, #31987 ) ;
#17229 = CARTESIAN_POINT ( 'NONE',  ( -107.8944406815436849, -280.8897397468701342, -244.2812028689015165 ) ) ;
#17230 = APPLICATION_CONTEXT ( 'automotive_design' ) ;
#17231 = CARTESIAN_POINT ( 'NONE',  ( 156.5250797092530206, 214.9970011440365454, 17.23862273017120117 ) ) ;
#17232 = CARTESIAN_POINT ( 'NONE',  ( -86.82570441288859797, -287.2906765238827234, -213.1897511470764925 ) ) ;
#17233 = FACE_OUTER_BOUND ( 'NONE', #64373, .T. ) ;
#17234 = CARTESIAN_POINT ( 'NONE',  ( -61.69377627843048373, -289.7356952099895580, -199.3705103345685927 ) ) ;
#17235 = CARTESIAN_POINT ( 'NONE',  ( 209.2568086740256206, 34.98978593258856051, 12.00000000000000000 ) ) ;
#17236 = CARTESIAN_POINT ( 'NONE',  ( -108.3576466698271616, -295.1029814045311923, -288.9544704216328341 ) ) ;
#17237 = CARTESIAN_POINT ( 'NONE',  ( -99.15205147371868577, -288.1302655786844298, -311.4980874790892926 ) ) ;
#17238 = CARTESIAN_POINT ( 'NONE',  ( 188.7508426036948208, 279.9709457756753181, -124.8390596414617590 ) ) ;
#17239 = CARTESIAN_POINT ( 'NONE',  ( -109.9110596246630251, -294.3080251905764726, -289.3510415761517152 ) ) ;
#17240 = CARTESIAN_POINT ( 'NONE',  ( 29.53334351106362732, -285.5505582073838582, -233.5031484245756133 ) ) ;
#17241 = CARTESIAN_POINT ( 'NONE',  ( 25.81042619173718577, -282.6311508200469120, -232.0750983725606602 ) ) ;
#17242 = CARTESIAN_POINT ( 'NONE',  ( -106.0983797336095904, -282.3721391996784860, -302.7106623519830464 ) ) ;
#17243 = CARTESIAN_POINT ( 'NONE',  ( -109.6229496821357969, -290.4161680802360479, -280.6694549657781863 ) ) ;
#17244 = CIRCLE ( 'NONE', #91290, 7.500000000000012434 ) ;
#17245 = TOROIDAL_SURFACE ( 'NONE', #61130, 4.499999999999990230, 0.5000000000000000000 ) ;
#17246 = CARTESIAN_POINT ( 'NONE',  ( 29.50034846094592211, -282.5640185884734592, -239.4573254970343044 ) ) ;
#17247 = CARTESIAN_POINT ( 'NONE',  ( -1.163283040704384375, -283.3616900024941287, -333.9513991910898199 ) ) ;
#17248 = EDGE_CURVE ( 'NONE', #71446, #25460, #33894, .T. ) ;
#17249 = CARTESIAN_POINT ( 'NONE',  ( 37.71154575191060587, -289.6181687691748721, -277.1003378065689162 ) ) ;
#17250 = CARTESIAN_POINT ( 'NONE',  ( -113.5240099626964394, -273.0281573994048472, -258.9520543865493778 ) ) ;
#17251 = ORIENTED_EDGE ( 'NONE', *, *, #57750, .T. ) ;
#17252 = AXIS2_PLACEMENT_3D ( 'NONE', #4859, #56477, #48398 ) ;
#17253 = CARTESIAN_POINT ( 'NONE',  ( 37.59186835044970110, -275.7744047437907398, -288.1368362308884912 ) ) ;
#17254 = CARTESIAN_POINT ( 'NONE',  ( -6.615725236069108561, -294.4374966344255995, -202.3334671863436824 ) ) ;
#17255 = DIRECTION ( 'NONE',  ( -0.000000000000000000, -1.000000000000000000, -0.000000000000000000 ) ) ;
#17256 = CARTESIAN_POINT ( 'NONE',  ( 21.27581636871892101, -289.4090924074130839, -223.5744983911110353 ) ) ;
#17257 = CARTESIAN_POINT ( 'NONE',  ( 34.30721672438074421, -273.8446070346852821, -293.0868993893792549 ) ) ;
#17258 = CARTESIAN_POINT ( 'NONE',  ( 155.0231696494769835, 19.71747416578156020, -13.29925684040344969 ) ) ;
#17259 = CARTESIAN_POINT ( 'NONE',  ( -48.82905715762767329, -296.3081915587064259, -194.9788592001873440 ) ) ;
#17260 = CARTESIAN_POINT ( 'NONE',  ( -44.39675081950817059, -293.5617031899628273, -196.8477340852852535 ) ) ;
#17261 = CARTESIAN_POINT ( 'NONE',  ( -19.23836903881461069, -273.6397564751534901, -199.4837471376149836 ) ) ;
#17262 = CARTESIAN_POINT ( 'NONE',  ( -82.16596912329586644, -292.9485735068852819, -211.8030051529857474 ) ) ;
#17263 = CIRCLE ( 'NONE', #80781, 11.40608546931776779 ) ;
#17264 = CARTESIAN_POINT ( 'NONE',  ( -94.48199854818197707, -292.1389076526286317, -224.5329478163124293 ) ) ;
#17265 = CARTESIAN_POINT ( 'NONE',  ( -111.1038514978274065, -286.2330297360794020, -276.4536574495593300 ) ) ;
#17266 = CARTESIAN_POINT ( 'NONE',  ( -113.7798749128485696, -292.0022879758289491, -268.3881773732959459 ) ) ;
#17267 = CARTESIAN_POINT ( 'NONE',  ( -36.40136205443786821, -293.3788782935071140, -193.8470972502124994 ) ) ;
#17268 = CARTESIAN_POINT ( 'NONE',  ( 22.93179133425186578, -293.9595900672553057, -311.6333210305399462 ) ) ;
#17269 = CARTESIAN_POINT ( 'NONE',  ( 36.25146153568864094, -289.7388097368263402, -284.8860849424076491 ) ) ;
#17270 = CARTESIAN_POINT ( 'NONE',  ( 36.47928983743612008, -281.9956219583908137, -292.4411704231692966 ) ) ;
#17271 = CARTESIAN_POINT ( 'NONE',  ( 51.50024267128915056, -297.2358502085104988, -194.8298982140941575 ) ) ;
#17272 = CARTESIAN_POINT ( 'NONE',  ( -111.1085870955612336, -284.1078938614560911, -292.4850959667163579 ) ) ;
#17273 = CARTESIAN_POINT ( 'NONE',  ( 35.78079552368199501, -277.7255356919781661, -285.3593657375697603 ) ) ;
#17274 = EDGE_CURVE ( 'NONE', #75279, #79924, #47612, .T. ) ;
#17275 = CARTESIAN_POINT ( 'NONE',  ( -96.24955757627314767, -282.7362816921143462, -314.1446175757996571 ) ) ;
#17276 = CARTESIAN_POINT ( 'NONE',  ( 28.39128983025559805, -285.0705969506945507, -234.1399340539306024 ) ) ;
#17277 = CARTESIAN_POINT ( 'NONE',  ( -14.97728027383291405, -274.9052119461082953, -342.8048412693465252 ) ) ;
#17278 = CARTESIAN_POINT ( 'NONE',  ( 197.7051530045995094, 41.80213891112347824, 12.00000000000000000 ) ) ;
#17279 = CARTESIAN_POINT ( 'NONE',  ( -45.65269004266314568, -282.6678403796090606, -342.9994538287614319 ) ) ;
#17280 = CARTESIAN_POINT ( 'NONE',  ( -73.59135694896299640, -280.7871346000828794, -202.8631258503381503 ) ) ;
#17281 = CARTESIAN_POINT ( 'NONE',  ( 38.32696717412664356, -286.4477840016668324, -257.3580460447529958 ) ) ;
#17282 = CARTESIAN_POINT ( 'NONE',  ( -20.59743046470784478, -296.5945001501515321, -342.5083564738381483 ) ) ;
#17283 = CARTESIAN_POINT ( 'NONE',  ( 18.33276714831145782, -277.8692702564945876, -322.3879774774844122 ) ) ;
#17284 = CARTESIAN_POINT ( 'NONE',  ( 38.43342003731101642, -276.7344543188282842, -259.8051037481508843 ) ) ;
#17285 = CARTESIAN_POINT ( 'NONE',  ( -100.5838947601770030, -277.8843166162832858, -306.9239246804433492 ) ) ;
#17286 = CARTESIAN_POINT ( 'NONE',  ( -111.9874385977608000, -274.5676579626259013, -267.6010372180072636 ) ) ;
#17287 = CARTESIAN_POINT ( 'NONE',  ( 21.80495789753821612, -284.9221397419026971, -224.5168023592966904 ) ) ;
#17288 = CARTESIAN_POINT ( 'NONE',  ( -65.13603027350988839, -291.0093331354566430, -341.3669608528520030 ) ) ;
#17289 = CARTESIAN_POINT ( 'NONE',  ( 10.48282447417927976, -293.2935075352553440, -325.9222637526256676 ) ) ;
#17290 = ORIENTED_EDGE ( 'NONE', *, *, #70497, .F. ) ;
#17291 = EDGE_CURVE ( 'NONE', #49791, #74853, #10653, .T. ) ;
#17292 = CARTESIAN_POINT ( 'NONE',  ( 33.97137422211154245, -293.0110402770283144, -254.6019189343419100 ) ) ;
#17293 = EDGE_LOOP ( 'NONE', ( #52940, #63550, #80191, #73505 ) ) ;
#17294 = CARTESIAN_POINT ( 'NONE',  ( 3.029155595932095046, -289.6036105966744572, -335.6283790457749774 ) ) ;
#17295 = CARTESIAN_POINT ( 'NONE',  ( -110.2609086990360083, -279.2716149022717786, -265.1956858301158491 ) ) ;
#17296 = CARTESIAN_POINT ( 'NONE',  ( -106.2296086547079739, -295.9070403498156452, -236.6572818849101623 ) ) ;
#17297 = CARTESIAN_POINT ( 'NONE',  ( 14.17243384388611638, -287.4044519914698412, -213.1967195512843318 ) ) ;
#17298 = CARTESIAN_POINT ( 'NONE',  ( 39.68137774207683321, -287.9002644426528832, -271.5467260053712266 ) ) ;
#17299 = CARTESIAN_POINT ( 'NONE',  ( -105.5862007463691583, -285.2321602334261570, -244.3846743830534933 ) ) ;
#17300 = CARTESIAN_POINT ( 'NONE',  ( 64.61140586824606658, 48.03908741837865648, -318.8617120424071345 ) ) ;
#17301 = CARTESIAN_POINT ( 'NONE',  ( 152.0371421904949898, 206.9602274457216140, -216.0695842911233342 ) ) ;
#17302 = CARTESIAN_POINT ( 'NONE',  ( 188.1653916184831985, 268.5676892509308118, -137.5199885634606005 ) ) ;
#17303 = CARTESIAN_POINT ( 'NONE',  ( -74.10323679174986466, -276.7513667766365870, -333.6160873461321330 ) ) ;
#17304 = CARTESIAN_POINT ( 'NONE',  ( -107.4161531682840973, -277.1864005470471852, -292.0671586347614266 ) ) ;
#17305 = CARTESIAN_POINT ( 'NONE',  ( 53.50357903997114306, -298.6686332334738267, -193.4299620268588740 ) ) ;
#17306 = CARTESIAN_POINT ( 'NONE',  ( -37.71430735586704941, -140.7961144971097838, -361.8212181249343757 ) ) ;
#17307 = CARTESIAN_POINT ( 'NONE',  ( -6.787134126971194448, -275.3442443828581077, -340.5159738421589850 ) ) ;
#17308 = AXIS2_PLACEMENT_3D ( 'NONE', #75229, #52046, #80930 ) ;
#17309 =( BOUNDED_CURVE ( )  B_SPLINE_CURVE ( 3, ( #31440, #88247, #59870, #87313 ),
 .UNSPECIFIED., .F., .F. ) 
 B_SPLINE_CURVE_WITH_KNOTS ( ( 4, 4 ),
 ( 2.029441677703989200, 3.141592653589793116 ),
 .UNSPECIFIED. ) 
 CURVE ( )  GEOMETRIC_REPRESENTATION_ITEM ( )  RATIONAL_B_SPLINE_CURVE ( ( 1.000000000000000000, 0.8995554851227761661, 0.8995554851227761661, 1.000000000000000000 ) ) 
 REPRESENTATION_ITEM ( '' )  );
#17310 = CARTESIAN_POINT ( 'NONE',  ( -110.3985106707871040, -291.0335470360811883, -271.1923067597078330 ) ) ;
#17311 = CARTESIAN_POINT ( 'NONE',  ( -36.90828264224272459, -298.8602770830073609, -193.5225356378665538 ) ) ;
#17312 = CARTESIAN_POINT ( 'NONE',  ( 33.87054648191396211, -285.9981849473351190, -252.1427390963366690 ) ) ;
#17313 = CARTESIAN_POINT ( 'NONE',  ( -106.7547775772333125, -273.6283590829956438, -237.2682567386859205 ) ) ;
#17314 = CARTESIAN_POINT ( 'NONE',  ( 10.29312531376072037, -294.5396583741396626, -325.6776924391340344 ) ) ;
#17315 = ORIENTED_EDGE ( 'NONE', *, *, #18614, .F. ) ;
#17316 =( BOUNDED_CURVE ( )  B_SPLINE_CURVE ( 3, ( #27493, #69177, #25605, #33653 ),
 .UNSPECIFIED., .F., .F. ) 
 B_SPLINE_CURVE_WITH_KNOTS ( ( 4, 4 ),
 ( 0.000000000000000000, 1.112150975885804360 ),
 .UNSPECIFIED. ) 
 CURVE ( )  GEOMETRIC_REPRESENTATION_ITEM ( )  RATIONAL_B_SPLINE_CURVE ( ( 1.000000000000000000, 0.8995554851227760551, 0.8995554851227760551, 1.000000000000000000 ) ) 
 REPRESENTATION_ITEM ( '' )  );
#17317 = VECTOR ( 'NONE', #86922, 1000.000000000000227 ) ;
#17318 = CARTESIAN_POINT ( 'NONE',  ( -88.22403272715123990, -279.6782952476348214, -326.2207852301311846 ) ) ;
#17319 = CARTESIAN_POINT ( 'NONE',  ( 29.70519285336511217, -281.5510723694352464, -308.2088008696974839 ) ) ;
#17320 = CIRCLE ( 'NONE', #30697, 4.999999999999993783 ) ;
#17321 = CARTESIAN_POINT ( 'NONE',  ( -110.2096938671491273, -279.5204610175326820, -278.8391610750215364 ) ) ;
#17322 = CARTESIAN_POINT ( 'NONE',  ( 28.23292922482151823, -277.8186542418793010, -308.7530702280602100 ) ) ;
#17323 = CARTESIAN_POINT ( 'NONE',  ( -110.8792132449868006, -271.1041387173808062, -264.8424321276107207 ) ) ;
#17324 = DIRECTION ( 'NONE',  ( 1.000000000000000000, 0.000000000000000000, 0.000000000000000000 ) ) ;
#17325 = CARTESIAN_POINT ( 'NONE',  ( -100.8128535064753351, -279.2127159221628290, -234.2998826556250265 ) ) ;
#17326 = CARTESIAN_POINT ( 'NONE',  ( -35.53784720795390228, -274.8770435820706552, -193.5306673363320158 ) ) ;
#17327 = AXIS2_PLACEMENT_3D ( 'NONE', #88982, #67702, #37406 ) ;
#17328 = CARTESIAN_POINT ( 'NONE',  ( -2.043237557616166100, -287.2794484643570740, -338.2383366514214345 ) ) ;
#17329 = CARTESIAN_POINT ( 'NONE',  ( -65.50058040811698845, -275.6841838574832764, -200.8341629001307638 ) ) ;
#17330 = CARTESIAN_POINT ( 'NONE',  ( 35.49543667650704748, -274.4194024630090212, -293.4556583519470792 ) ) ;
#17331 = CARTESIAN_POINT ( 'NONE',  ( 185.4166944662832179, 249.5000000000000568, 23.37680765314684095 ) ) ;
#17332 = CARTESIAN_POINT ( 'NONE',  ( -110.4986279574996075, -289.7385756856916146, -271.1769837689780616 ) ) ;
#17333 = CARTESIAN_POINT ( 'NONE',  ( -68.45190604978013482, -285.0026387793832328, -200.0227409260162972 ) ) ;
#17334 = CARTESIAN_POINT ( 'NONE',  ( 18.35280545869903435, -280.4780349904306149, -319.1063337730138869 ) ) ;
#17336 = CARTESIAN_POINT ( 'NONE',  ( -22.14238133598405511, -284.3280492697555246, -197.4364398687798712 ) ) ;
#17335 = CARTESIAN_POINT ( 'NONE',  ( 21.46995819204322231, -280.7432844575790796, -314.6149968204221636 ) ) ;
#17337 = CARTESIAN_POINT ( 'NONE',  ( -57.18235084095585563, -291.3081638130456668, -342.7422772900183645 ) ) ;
#17338 = CARTESIAN_POINT ( 'NONE',  ( 28.12868111699887308, -282.3078411552432385, -237.0707713852813754 ) ) ;
#17339 = CARTESIAN_POINT ( 'NONE',  ( -111.0966513668062987, -270.7302858448049392, -256.4752353820961162 ) ) ;
#17340 = CARTESIAN_POINT ( 'NONE',  ( -21.90813622569987018, -281.2574288904340278, -344.9817955370863842 ) ) ;
#17341 = CARTESIAN_POINT ( 'NONE',  ( 37.44480028843214825, -295.4797054385879846, -264.7060316005111531 ) ) ;
#17342 = CARTESIAN_POINT ( 'NONE',  ( -50.73866334289159141, -278.1231293446849691, -195.5647585248190126 ) ) ;
#17343 = CARTESIAN_POINT ( 'NONE',  ( -80.48787350135009433, -285.6351848300802203, -331.9746990533922144 ) ) ;
#17344 = CARTESIAN_POINT ( 'NONE',  ( 151.9231709899832197, 19.99481412879373821, 6.233581502755908943 ) ) ;
#17345 = CARTESIAN_POINT ( 'NONE',  ( 0.9488755633414936996, -294.4786119038654988, -205.1618984093132383 ) ) ;
#17346 = CARTESIAN_POINT ( 'NONE',  ( 33.97122977329271265, -273.2500782435105862, -246.9674522928405054 ) ) ;
#17347 = CARTESIAN_POINT ( 'NONE',  ( 39.54074170339981720, -286.7643335073328217, -271.5589967052943052 ) ) ;
#17348 = CARTESIAN_POINT ( 'NONE',  ( -86.44629943036402153, -289.7569767129008369, -215.1998949706504618 ) ) ;
#17349 = CARTESIAN_POINT ( 'NONE',  ( -43.26778476368559012, -275.6832172112468129, -431.4324561993768157 ) ) ;
#17350 = CARTESIAN_POINT ( 'NONE',  ( 30.72850444077189636, -274.6072431817221400, -298.2036865914383839 ) ) ;
#17351 = CARTESIAN_POINT ( 'NONE',  ( -12.61884051280087071, -292.8669864717097653, -340.4127388891209307 ) ) ;
#17352 = CARTESIAN_POINT ( 'NONE',  ( -90.94102016010253919, -291.1478831444605362, -320.7181809395301570 ) ) ;
#17353 = CARTESIAN_POINT ( 'NONE',  ( 175.2296996224750103, 158.6892791692949629, -24.00000000000001066 ) ) ;
#17354 = CARTESIAN_POINT ( 'NONE',  ( 104.1717476309105166, -299.5541904835127980, -195.3611179825600175 ) ) ;
#17355 = CARTESIAN_POINT ( 'NONE',  ( 33.82329035037079024, -291.6783760850907470, -242.6786271492420894 ) ) ;
#17356 = CARTESIAN_POINT ( 'NONE',  ( -25.02818243234750284, -287.8117877235282549, -197.5437615274489076 ) ) ;
#17357 = CARTESIAN_POINT ( 'NONE',  ( -45.93375120771811027, -287.3993972179886782, -345.9128883804920065 ) ) ;
#17358 = CARTESIAN_POINT ( 'NONE',  ( 19.96268232578134416, -288.3296445726543880, -224.1720922405726242 ) ) ;
#17359 = CARTESIAN_POINT ( 'NONE',  ( 85.55100297371609486, -296.0521521680024080, -517.1711561948568487 ) ) ;
#17360 = CARTESIAN_POINT ( 'NONE',  ( 30.63900943890631012, -288.7176255493006352, -297.5389725819040336 ) ) ;
#17361 = EDGE_CURVE ( 'NONE', #49216, #4620, #18600, .T. ) ;
#17362 = CARTESIAN_POINT ( 'NONE',  ( -50.16233512675388084, -297.1947526626561285, -344.6704779160114072 ) ) ;
#17363 = DIRECTION ( 'NONE',  ( 0.000000000000000000, 1.000000000000000000, 0.000000000000000000 ) ) ;
#17364 = CARTESIAN_POINT ( 'NONE',  ( -33.76131852421374901, -287.3013387875780609, -193.8419074089113110 ) ) ;
#17365 = CARTESIAN_POINT ( 'NONE',  ( -38.54697923533018411, -275.1470060928124326, -345.9115084783269367 ) ) ;
#17366 = CARTESIAN_POINT ( 'NONE',  ( -104.9549896037654690, -278.4090899085048818, -307.1604029989917990 ) ) ;
#17367 = CARTESIAN_POINT ( 'NONE',  ( 21.95713398562930863, -280.5588514336336061, -221.2755542760304763 ) ) ;
#17368 = CARTESIAN_POINT ( 'NONE',  ( -111.7817001273665340, -274.4719972231438874, -270.3855101330484558 ) ) ;
#17369 = CARTESIAN_POINT ( 'NONE',  ( -55.20876260339449004, -283.8223120539859110, -197.4666836907997265 ) ) ;
#17370 = DIRECTION ( 'NONE',  ( 0.000000000000000000, 1.000000000000000000, 0.000000000000000000 ) ) ;
#17371 = CARTESIAN_POINT ( 'NONE',  ( 18.91583923652932597, -279.0132568130363211, -221.9065400194043605 ) ) ;
#17372 = CARTESIAN_POINT ( 'NONE',  ( 32.71013882639473280, -279.9002235033647139, -297.1517974412815875 ) ) ;
#17373 = DIRECTION ( 'NONE',  ( 0.000000000000000000, 0.000000000000000000, 1.000000000000000000 ) ) ;
#17374 = CARTESIAN_POINT ( 'NONE',  ( 10.07989956661196729, -274.8922012460616315, -330.2106776633971776 ) ) ;
#17375 = CARTESIAN_POINT ( 'NONE',  ( -110.9055404474918305, -298.1293450798474396, -265.9942943827450108 ) ) ;
#17376 = CARTESIAN_POINT ( 'NONE',  ( 15.53044193640267423, -281.2454830924386897, -325.9131575730608006 ) ) ;
#17377 = CARTESIAN_POINT ( 'NONE',  ( -92.02855128315889033, -298.1876951188758085, -221.6501668604090867 ) ) ;
#17378 = CARTESIAN_POINT ( 'NONE',  ( -75.54825422226015519, -298.8691424917408881, -204.0163945042463638 ) ) ;
#17379 = CARTESIAN_POINT ( 'NONE',  ( 9.501894560030693881, -274.3835815511989153, -214.2791420062029601 ) ) ;
#17380 = CARTESIAN_POINT ( 'NONE',  ( 12.23425376785284691, -294.7417573533030577, -214.0137313260702285 ) ) ;
#17381 = CARTESIAN_POINT ( 'NONE',  ( 34.85349275685213399, -287.3803270298765256, -243.5869862729987290 ) ) ;
#17382 = CARTESIAN_POINT ( 'NONE',  ( -97.41631948712981171, -277.2548627894911988, -224.5104268710522888 ) ) ;
#17383 = CIRCLE ( 'NONE', #27947, 7.999911143031724237 ) ;
#17384 = CARTESIAN_POINT ( 'NONE',  ( -113.3603913257561118, -290.2322206120939541, -282.6150395224028671 ) ) ;
#17385 = EDGE_CURVE ( 'NONE', #19715, #23354, #68404, .T. ) ;
#17386 = EDGE_CURVE ( 'NONE', #83022, #62368, #77460, .T. ) ;
#17387 = CARTESIAN_POINT ( 'NONE',  ( 18.84998463886424602, -285.9462176970576479, -223.3745348976965488 ) ) ;
#17388 = CARTESIAN_POINT ( 'NONE',  ( -28.07039215829282597, -290.1695408240248071, -195.8840855177694209 ) ) ;
#17389 = ORIENTED_EDGE ( 'NONE', *, *, #79781, .F. ) ;
#17390 = CARTESIAN_POINT ( 'NONE',  ( -113.2098679957031493, -271.2709011634024137, -296.4525692007673570 ) ) ;
#17391 = CARTESIAN_POINT ( 'NONE',  ( 33.75952855361387606, -287.2813925079688033, -287.1719395516581130 ) ) ;
#17392 = DIRECTION ( 'NONE',  ( 0.000000000000000000, 0.000000000000000000, 1.000000000000000000 ) ) ;
#17393 = CARTESIAN_POINT ( 'NONE',  ( -112.9032018303532823, -285.3199108162264679, -284.1908079601929558 ) ) ;
#17394 = CARTESIAN_POINT ( 'NONE',  ( 17.33047449263798612, -291.8679161439345080, -216.3995816595989083 ) ) ;
#17395 = CARTESIAN_POINT ( 'NONE',  ( 27.42489549581026864, -282.3294860345162647, -229.5361227191907574 ) ) ;
#17396 = CARTESIAN_POINT ( 'NONE',  ( -70.21682618138015641, -283.3311927541809609, -335.5535141087693205 ) ) ;
#17397 = CARTESIAN_POINT ( 'NONE',  ( -99.09243925907853168, -297.1641952792186885, -224.3407836498434165 ) ) ;
#17398 = CARTESIAN_POINT ( 'NONE',  ( -31.31585938465800112, -275.4449934751644378, -197.1026819448701701 ) ) ;
#17399 = CARTESIAN_POINT ( 'NONE',  ( -41.66341245129767401, -290.0176888039568439, -195.7905555449135022 ) ) ;
#17400 = AXIS2_PLACEMENT_3D ( 'NONE', #66682, #44426, #1809 ) ;
#17401 = CARTESIAN_POINT ( 'NONE',  ( -24.51202229943083921, -273.0143260533575926, -198.0421738022632496 ) ) ;
#17402 = VERTEX_POINT ( 'NONE', #66391 ) ;
#17403 = CARTESIAN_POINT ( 'NONE',  ( 11.63197158325052172, -285.8906705383787994, 52.50000000000000711 ) ) ;
#17404 = CARTESIAN_POINT ( 'NONE',  ( -35.93020660818435630, -287.9901466074219911, -195.9344971594413209 ) ) ;
#17405 = CARTESIAN_POINT ( 'NONE',  ( -16.57730310165831256, -295.8697747746049345, -344.2424982707772187 ) ) ;
#17406 = CARTESIAN_POINT ( 'NONE',  ( -109.7143091425620582, -285.3392583229757520, -260.0607232007880043 ) ) ;
#17407 = CARTESIAN_POINT ( 'NONE',  ( 39.47182112341977955, -274.6211883752372955, -271.1811299742585675 ) ) ;
#17408 = CARTESIAN_POINT ( 'NONE',  ( 19.33491743841234722, -293.4955389560321919, -218.3892620616566944 ) ) ;
#17409 = CARTESIAN_POINT ( 'NONE',  ( 27.65135217505240561, -285.1745211976586347, -231.3213609079857918 ) ) ;
#17410 = CARTESIAN_POINT ( 'NONE',  ( 8.896842877848062159, -294.7703685697233595, -331.9057475787039380 ) ) ;
#17411 = CARTESIAN_POINT ( 'NONE',  ( -108.3699965399736698, -290.6619709388741057, -287.3042167456861762 ) ) ;
#17412 = DIRECTION ( 'NONE',  ( 0.000000000000000000, 1.000000000000000000, 0.000000000000000000 ) ) ;
#17413 = DIRECTION ( 'NONE',  ( -0.000000000000000000, -0.000000000000000000, 1.000000000000000000 ) ) ;
#17414 = CARTESIAN_POINT ( 'NONE',  ( -60.31974984533258777, -287.2797680917233833, -197.5412312525447476 ) ) ;
#17415 = CARTESIAN_POINT ( 'NONE',  ( -37.30987171927208834, -271.5523547857346784, -190.3611179825600175 ) ) ;
#17416 = ORIENTED_EDGE ( 'NONE', *, *, #33617, .T. ) ;
#17417 = CARTESIAN_POINT ( 'NONE',  ( -66.69592087417289861, -282.3662966608265492, -337.5503074108665373 ) ) ;
#17418 = CARTESIAN_POINT ( 'NONE',  ( -97.04068790367236375, -277.5663565828650121, -318.9798592174279861 ) ) ;
#17419 = CARTESIAN_POINT ( 'NONE',  ( 21.95335797599150496, -282.9252805374165973, -224.6880888030420067 ) ) ;
#17420 = CARTESIAN_POINT ( 'NONE',  ( -29.05393780148455107, -125.5975973158746939, -363.1324652132601045 ) ) ;
#17421 = CARTESIAN_POINT ( 'NONE',  ( -52.81616487699096751, -281.8213018474361320, -345.2426454896730661 ) ) ;
#17422 = CARTESIAN_POINT ( 'NONE',  ( 16.22705510898434511, -284.8372971622442265, -218.3780893619775156 ) ) ;
#17423 = CARTESIAN_POINT ( 'NONE',  ( 18.43902994631035952, -300.5015369122558013, -194.3579889076426355 ) ) ;
#17424 = CARTESIAN_POINT ( 'NONE',  ( -80.18579986607710453, -296.1425222528308723, -329.5419557522594687 ) ) ;
#17425 = ORIENTED_EDGE ( 'NONE', *, *, #25604, .F. ) ;
#17426 = CARTESIAN_POINT ( 'NONE',  ( -44.33053900005747039, -290.6468708636233487, -197.1498615812441813 ) ) ;
#17427 = CARTESIAN_POINT ( 'NONE',  ( -113.9767765952946945, -279.1162914832361253, -277.3301055722702699 ) ) ;
#17428 = CARTESIAN_POINT ( 'NONE',  ( 32.06181328548421305, -275.2499161837557153, -247.5677234965944535 ) ) ;
#17429 = CARTESIAN_POINT ( 'NONE',  ( 16.72750232955500493, -275.2251956535507702, -324.8228837448914419 ) ) ;
#17430 = CARTESIAN_POINT ( 'NONE',  ( 179.7289557593406357, 250.5000000000000568, -24.91818181818184641 ) ) ;
#17431 = CARTESIAN_POINT ( 'NONE',  ( -27.99891104009856235, -272.1704639728073971, -195.8940181553785465 ) ) ;
#17432 = CARTESIAN_POINT ( 'NONE',  ( -39.07613178564673007, -296.4987845210786759, -346.7522041218230129 ) ) ;
#17433 = CARTESIAN_POINT ( 'NONE',  ( 139.1539576904058606, 275.5000000000000568, 10.50000000000000000 ) ) ;
#17434 = CARTESIAN_POINT ( 'NONE',  ( -43.23637629196743148, -278.5210525055342146, -507.4181868956659969 ) ) ;
#17435 = CARTESIAN_POINT ( 'NONE',  ( -95.35264803199918049, -285.0031781335119945, -315.2029835891626135 ) ) ;
#17436 = CARTESIAN_POINT ( 'NONE',  ( -97.23172872720684268, -285.6790394460022640, -317.1281842972056211 ) ) ;
#17437 = CARTESIAN_POINT ( 'NONE',  ( -80.69324594591869015, -283.0061209662997044, -329.2844126287917561 ) ) ;
#17438 = CARTESIAN_POINT ( 'NONE',  ( -7.199346675504460613, -275.0498768496129287, -337.7248986464228437 ) ) ;
#17439 = CARTESIAN_POINT ( 'NONE',  ( -3.029751930673151517, -284.4542661378049502, -336.2051097402604114 ) ) ;
#17440 = CARTESIAN_POINT ( 'NONE',  ( -108.4947006497384763, -276.7810372259582437, -289.5433563956704575 ) ) ;
#17441 = CARTESIAN_POINT ( 'NONE',  ( 19.42966961143937255, -277.2859519677858771, -316.7623405887259764 ) ) ;
#17442 = CARTESIAN_POINT ( 'NONE',  ( 207.6662022560304024, 36.29800326561213808, 14.90057469441954119 ) ) ;
#17443 = CARTESIAN_POINT ( 'NONE',  ( -106.0358127635873871, -279.8000975799142793, -235.8147225526070088 ) ) ;
#17444 = CARTESIAN_POINT ( 'NONE',  ( -41.01173716849114470, -280.4995061011442203, -193.4970532098554088 ) ) ;
#17445 = VERTEX_POINT ( 'NONE', #8604 ) ;
#17446 = CARTESIAN_POINT ( 'NONE',  ( 196.7071296363291140, 19.50333209967902448, -12.79999999999991722 ) ) ;
#17447 = CARTESIAN_POINT ( 'NONE',  ( 35.95555826579214909, -289.6565411443053222, -289.5396840117884949 ) ) ;
#17448 = EDGE_CURVE ( 'NONE', #68064, #74899, #8150, .T. ) ;
#17449 = CARTESIAN_POINT ( 'NONE',  ( -108.6320850499026562, -295.9657148304178804, -253.9208398440649432 ) ) ;
#17450 = CARTESIAN_POINT ( 'NONE',  ( -103.1243386839901177, -290.4223665898716717, -230.4343924258889160 ) ) ;
#17451 = CARTESIAN_POINT ( 'NONE',  ( 36.56597276341372549, -285.7293118389002871, -265.5427631288117141 ) ) ;
#17453 = CARTESIAN_POINT ( 'NONE',  ( -104.9828017033906633, -288.3916052706242681, -300.5319968872909726 ) ) ;
#17452 = CARTESIAN_POINT ( 'NONE',  ( 5.079731740519486394, -285.2126242096164788, -210.1672529268174117 ) ) ;
#17454 = CARTESIAN_POINT ( 'NONE',  ( -10.61962907896915631, -287.6137106452035823, -201.9877259235813369 ) ) ;
#17455 = CARTESIAN_POINT ( 'NONE',  ( -105.7622911574838724, -276.1477636316831195, -301.2060395054491551 ) ) ;
#17456 = CARTESIAN_POINT ( 'NONE',  ( 2.741799994701370924, -286.9242427873922452, -335.2285111532752921 ) ) ;
#17457 = CARTESIAN_POINT ( 'NONE',  ( 28.36672737334033201, -289.0702739995776369, -234.0953939819645768 ) ) ;
#17458 = CARTESIAN_POINT ( 'NONE',  ( 13.34812564381097566, -286.3453118897524519, -325.9345112661461030 ) ) ;
#17459 = CARTESIAN_POINT ( 'NONE',  ( -4.711594718966118478, -283.5526203182462837, -335.9254731602548532 ) ) ;
#17460 = CARTESIAN_POINT ( 'NONE',  ( -109.4800393152221432, -292.8236813707837314, -249.2403119589064033 ) ) ;
#17461 = DIRECTION ( 'NONE',  ( -0.000000000000000000, -0.000000000000000000, -1.000000000000000000 ) ) ;
#17462 = CARTESIAN_POINT ( 'NONE',  ( 185.8264795993290477, 214.9910457053126720, 23.09031830825835385 ) ) ;
#17463 = CARTESIAN_POINT ( 'NONE',  ( -112.3483424243524524, -298.5886378315103116, -261.2332590518147981 ) ) ;
#17464 = CARTESIAN_POINT ( 'NONE',  ( -22.15091938936496518, -279.4487684361694733, -198.7420997981078870 ) ) ;
#17465 = CARTESIAN_POINT ( 'NONE',  ( 22.59322928371074113, -280.1684892195593193, -315.4689691595826275 ) ) ;
#17466 = CARTESIAN_POINT ( 'NONE',  ( 17.43923545849672863, -293.4913175282214866, -324.3182100686868239 ) ) ;
#17467 = CARTESIAN_POINT ( 'NONE',  ( -84.57134656037391096, -295.7892314662637432, -213.5863795484178809 ) ) ;
#17468 = CARTESIAN_POINT ( 'NONE',  ( 35.52398691814099152, -280.1064382329424234, -260.3990408057631498 ) ) ;
#17469 = CARTESIAN_POINT ( 'NONE',  ( 33.43850124423435233, -273.3300717607625074, -247.1413374894281105 ) ) ;
#17470 = CARTESIAN_POINT ( 'NONE',  ( -55.91185261690477404, -296.6113598862893923, -341.5221698142247533 ) ) ;
#17471 = DIRECTION ( 'NONE',  ( -0.5379402104274362273, 0.8429829950866658539, 0.000000000000000000 ) ) ;
#17472 = CARTESIAN_POINT ( 'NONE',  ( -36.53015085399769646, -296.5420233074727889, -194.0546518089647634 ) ) ;
#17473 = CARTESIAN_POINT ( 'NONE',  ( 12.71127048530909853, -292.6055182704702133, -327.6031832661492444 ) ) ;
#17474 = CARTESIAN_POINT ( 'NONE',  ( 7.017093579273952386, -294.0950555991188935, -211.6442350926261327 ) ) ;
#17475 = FACE_OUTER_BOUND ( 'NONE', #12518, .T. ) ;
#17476 = CARTESIAN_POINT ( 'NONE',  ( 32.90808573650183178, -294.6252299198634432, -290.8406812693814913 ) ) ;
#17477 = CARTESIAN_POINT ( 'NONE',  ( 195.7212220663432163, 20.45996914382524423, 12.49744573203606279 ) ) ;
#17479 = CARTESIAN_POINT ( 'NONE',  ( 29.49005693663191252, -293.9472564303571289, -299.7297449106809495 ) ) ;
#17478 = CARTESIAN_POINT ( 'NONE',  ( -65.97512147630251889, -281.4450370303358113, -340.0781880884891848 ) ) ;
#17480 = CARTESIAN_POINT ( 'NONE',  ( 26.72188612836074029, -282.1144386810832998, -313.0794620043430427 ) ) ;
#17481 = CARTESIAN_POINT ( 'NONE',  ( 0.6287828212901023228, -282.4739372254828709, -204.9750190359183080 ) ) ;
#17482 = CARTESIAN_POINT ( 'NONE',  ( -9.997500605309646460, -286.0661833940826568, -198.3457388481283203 ) ) ;
#17483 = CARTESIAN_POINT ( 'NONE',  ( -69.79007302455002559, -289.6238236234000283, -202.9145480600821543 ) ) ;
#17484 = CARTESIAN_POINT ( 'NONE',  ( 38.92620833365420197, -280.0627212286973418, -272.7929670375329465 ) ) ;
#17485 = CARTESIAN_POINT ( 'NONE',  ( 23.03556061290170476, -287.1073233994362113, -317.6694546320412087 ) ) ;
#17486 = FACE_OUTER_BOUND ( 'NONE', #25314, .T. ) ;
#17487 = CARTESIAN_POINT ( 'NONE',  ( -78.37784092801625491, -297.2142509949216560, -331.7618536361208612 ) ) ;
#17488 = CARTESIAN_POINT ( 'NONE',  ( 31.33373573036174520, -277.4122267762397200, -303.9823026842777267 ) ) ;
#17490 = CARTESIAN_POINT ( 'NONE',  ( -7.987051889962353712, -280.1143254664593201, -203.4864502092059411 ) ) ;
#17489 = CARTESIAN_POINT ( 'NONE',  ( 38.01220734520700262, -291.5360035164656551, -267.5242249225218529 ) ) ;
#17491 = CARTESIAN_POINT ( 'NONE',  ( -4.606071721740135239, -292.6383004410208173, -200.6662212011133875 ) ) ;
#17492 = CARTESIAN_POINT ( 'NONE',  ( -104.1472886334710211, -283.0978109061526879, -234.9457931597620188 ) ) ;
#17493 = CARTESIAN_POINT ( 'NONE',  ( -9.918746155033637990, -278.6941960401608753, -340.1678672598071103 ) ) ;
#17494 = CARTESIAN_POINT ( 'NONE',  ( 10.43599032618497979, -293.4319046665373207, -325.8651785753781951 ) ) ;
#17495 = CARTESIAN_POINT ( 'NONE',  ( -34.12766851902003395, -296.0922285863567254, -195.3622050365462997 ) ) ;
#17496 = ORIENTED_EDGE ( 'NONE', *, *, #32434, .T. ) ;
#17497 = DIRECTION ( 'NONE',  ( -0.000000000000000000, -0.000000000000000000, -1.000000000000000000 ) ) ;
#17498 = CARTESIAN_POINT ( 'NONE',  ( -109.8941877590768712, -280.7584839853464018, -252.8116637138289491 ) ) ;
#17499 = CARTESIAN_POINT ( 'NONE',  ( 34.54484983433269463, -292.8868745628288934, -257.2411398688824420 ) ) ;
#17500 = CYLINDRICAL_SURFACE ( 'NONE', #24682, 7.999999999999992895 ) ;
#17501 = CARTESIAN_POINT ( 'NONE',  ( -37.30987171927208834, -295.5523547857347353, -200.3611179825600459 ) ) ;
#17502 = CARTESIAN_POINT ( 'NONE',  ( -51.74467765753521320, -296.9310961366714992, -194.9055242722224079 ) ) ;
#17503 = CARTESIAN_POINT ( 'NONE',  ( 16.35186851445192247, -289.6243635113345931, -324.9352531123055883 ) ) ;
#17504 = CARTESIAN_POINT ( 'NONE',  ( 3.612852318004160956, -288.3177486632435489, -330.8515715501690693 ) ) ;
#17505 = CARTESIAN_POINT ( 'NONE',  ( -51.98387877882040442, -281.3816212681724664, -198.0848371837162745 ) ) ;
#17506 = CARTESIAN_POINT ( 'NONE',  ( -92.61639579301298397, -299.0064520846261189, -221.1403699812744605 ) ) ;
#17507 = EDGE_CURVE ( 'NONE', #13368, #48925, #16962, .T. ) ;
#17508 = CARTESIAN_POINT ( 'NONE',  ( -92.49673606005032411, -278.0347397038505051, -221.9162614387430210 ) ) ;
#17509 = ORIENTED_EDGE ( 'NONE', *, *, #43641, .F. ) ;
#17510 = CARTESIAN_POINT ( 'NONE',  ( 99.14367289792072313, -299.3839090181289748, -193.3896128337344464 ) ) ;
#17511 = CARTESIAN_POINT ( 'NONE',  ( -4.213781257199535446, -294.4124272079877755, -203.6846733922491524 ) ) ;
#17512 = CARTESIAN_POINT ( 'NONE',  ( 37.29121272633503992, -295.3465699402026985, -285.7354061505645291 ) ) ;
#17513 = CARTESIAN_POINT ( 'NONE',  ( -43.18343439339132317, -283.1093320178187582, -430.6442049081568939 ) ) ;
#17514 = EDGE_CURVE ( 'NONE', #14181, #28861, #78734, .T. ) ;
#17515 = CARTESIAN_POINT ( 'NONE',  ( -108.4476387076542210, -290.9800514709121444, -287.3269120187252952 ) ) ;
#17516 = CARTESIAN_POINT ( 'NONE',  ( 157.4970531492008661, 276.0000000000000568, 16.90571646082702983 ) ) ;
#17517 = EDGE_LOOP ( 'NONE', ( #26631, #61006, #2763, #67395, #61105, #14033, #29296 ) ) ;
#17518 = CARTESIAN_POINT ( 'NONE',  ( -1.369095648345087568, -290.6636434989744657, -203.6807069975050410 ) ) ;
#17519 = CARTESIAN_POINT ( 'NONE',  ( -110.4032385894416564, -272.0598842017238894, -270.3548639019163602 ) ) ;
#17520 = CARTESIAN_POINT ( 'NONE',  ( 204.6539576904058606, 287.9062406767683910, 3.999999999999991562 ) ) ;
#17521 = DIRECTION ( 'NONE',  ( 0.000000000000000000, 0.000000000000000000, 1.000000000000000000 ) ) ;
#17522 = CARTESIAN_POINT ( 'NONE',  ( -95.84689571780667450, -291.4067589979324566, -319.3696406983293627 ) ) ;
#17523 = CARTESIAN_POINT ( 'NONE',  ( -88.47809603358389552, -298.1948066931273615, -334.5364918783848793 ) ) ;
#17524 = CARTESIAN_POINT ( 'NONE',  ( 37.51354006194395652, -289.5249655844303902, -268.2355949849344370 ) ) ;
#17525 = CARTESIAN_POINT ( 'NONE',  ( 20.43004431873800897, -272.8944578711617055, -222.7958578237532947 ) ) ;
#17526 = CARTESIAN_POINT ( 'NONE',  ( 36.44470349350193317, -277.3449787899690477, -260.5183115621274510 ) ) ;
#17527 = CARTESIAN_POINT ( 'NONE',  ( -78.02204385755844385, -289.5805180903799396, -208.0199291073758161 ) ) ;
#17528 = CARTESIAN_POINT ( 'NONE',  ( -107.3799877926219466, -280.7857915663868766, -241.4657249381293127 ) ) ;
#17529 = EDGE_LOOP ( 'NONE', ( #53252, #29553 ) ) ;
#17530 = CARTESIAN_POINT ( 'NONE',  ( -33.49915127433074957, -282.3511272221823560, -343.3745813227926078 ) ) ;
#17531 = CARTESIAN_POINT ( 'NONE',  ( -113.4576900262697166, -279.5088570713479044, -280.1537234041435340 ) ) ;
#17532 = CARTESIAN_POINT ( 'NONE',  ( 3.622666666422747372, -279.3847135291584891, -205.5687900262641392 ) ) ;
#17533 = CARTESIAN_POINT ( 'NONE',  ( 159.4405072948125053, 218.8499916850896625, -202.6910633192169371 ) ) ;
#17534 = CARTESIAN_POINT ( 'NONE',  ( 37.71279890453170935, -276.2904820463264173, -254.1855979908594350 ) ) ;
#17535 = APPLICATION_PROTOCOL_DEFINITION ( 'draft international standard', 'automotive_design', 1998, #31747 ) ;
#17536 = CARTESIAN_POINT ( 'NONE',  ( 13.48807720687364053, -276.2682843017167897, -213.3779467923982907 ) ) ;
#17537 = CARTESIAN_POINT ( 'NONE',  ( 99.44099354567467230, -302.2645883696979467, -195.3030568020281521 ) ) ;
#17538 = ORIENTED_EDGE ( 'NONE', *, *, #64655, .F. ) ;
#17539 = ORIENTED_EDGE ( 'NONE', *, *, #20409, .T. ) ;
#17540 = CARTESIAN_POINT ( 'NONE',  ( -110.0946008801723224, -291.5134281744877853, -279.3745249762035314 ) ) ;
#17541 = CARTESIAN_POINT ( 'NONE',  ( -98.20386861814067458, -291.6986682820609076, -315.8773571623503926 ) ) ;
#17542 = CARTESIAN_POINT ( 'NONE',  ( -98.38008394364008780, -290.4589650651858506, -230.0422246006149010 ) ) ;
#17543 = CARTESIAN_POINT ( 'NONE',  ( -69.76119187579043057, -285.1443256224156357, -200.5721025084264966 ) ) ;
#17544 = CARTESIAN_POINT ( 'NONE',  ( 165.7865175155837676, 3.000000000000000000, -9.000000000000001776 ) ) ;
#17545 = CARTESIAN_POINT ( 'NONE',  ( 10.41099691718589071, -280.7803217381434138, -326.6965947874548419 ) ) ;
#17546 = CARTESIAN_POINT ( 'NONE',  ( -34.50750544262766795, -290.8767156475494176, -344.5926187316542837 ) ) ;
#17547 = CARTESIAN_POINT ( 'NONE',  ( -29.38888906310765137, -281.4296026389145595, -343.6750557052867521 ) ) ;
#17548 = CARTESIAN_POINT ( 'NONE',  ( 19.20488162198130055, -282.2057988919751210, -223.3977153338049106 ) ) ;
#17549 = CARTESIAN_POINT ( 'NONE',  ( -8.310972920920896456, -289.6224746684585512, -341.4389546749428064 ) ) ;
#17550 = CARTESIAN_POINT ( 'NONE',  ( -105.5740067817427956, -279.3947497613974065, -244.0977306108511300 ) ) ;
#17551 = CARTESIAN_POINT ( 'NONE',  ( -91.32963113160940338, -288.5940226579364776, -324.7801353660519226 ) ) ;
#17552 = CARTESIAN_POINT ( 'NONE',  ( -60.47107579267689204, -286.5625942198196867, -197.0308933975291268 ) ) ;
#17553 = CARTESIAN_POINT ( 'NONE',  ( -64.53131373240800883, -286.1989270235665686, -198.3729949387868601 ) ) ;
#17554 = CARTESIAN_POINT ( 'NONE',  ( -110.3904050505611991, -284.7115739677781221, -270.9114176497573112 ) ) ;
#17555 = EDGE_LOOP ( 'NONE', ( #44898, #18549, #33954, #20594 ) ) ;
#17556 = DIRECTION ( 'NONE',  ( -1.000000000000000000, 0.000000000000000000, 0.000000000000000000 ) ) ;
#17557 = CARTESIAN_POINT ( 'NONE',  ( -16.98168619059447693, -294.1727440538232941, -197.3832082391498943 ) ) ;
#17558 = CARTESIAN_POINT ( 'NONE',  ( 13.05829143550436733, -293.0504138646471688, -327.9912201096366289 ) ) ;
#17559 = CARTESIAN_POINT ( 'NONE',  ( -45.94760717793854354, -276.2225555154175254, -343.1398029587629708 ) ) ;
#17560 = CARTESIAN_POINT ( 'NONE',  ( -114.2644733835511914, -295.8744718991156901, -272.4587236071556617 ) ) ;
#17561 = CARTESIAN_POINT ( 'NONE',  ( -44.34702231820411811, -290.4419559596660179, -196.9502023754466506 ) ) ;
#17562 = CARTESIAN_POINT ( 'NONE',  ( -67.73149879945538032, -293.6963548811190776, -337.8615645571416053 ) ) ;
#17563 = B_SPLINE_CURVE_WITH_KNOTS ( 'NONE', 3,
 ( #91433, #76776, #92364, #27526, #39822, #11903, #62589, #20429 ),
 .UNSPECIFIED., .F., .F.,
 ( 4, 2, 2, 4 ),
 ( 4.336808689942017736E-19, 0.004152702846877201481, 0.006229054270315790079, 0.008305405693754378676 ),
 .UNSPECIFIED. ) ;
#17564 = CARTESIAN_POINT ( 'NONE',  ( -97.09350757342762961, -292.3505356560202131, -227.6505802757958747 ) ) ;
#17565 = CARTESIAN_POINT ( 'NONE',  ( -2.303740420511388720, -293.6070158556617002, -205.9530174245219314 ) ) ;
#17566 = CARTESIAN_POINT ( 'NONE',  ( 121.3395553409046528, -299.5541904835127980, -195.3611179825600175 ) ) ;
#17567 = CARTESIAN_POINT ( 'NONE',  ( -14.36720165022969375, -292.7547783989718937, -341.9306704774790546 ) ) ;
#17568 = CARTESIAN_POINT ( 'NONE',  ( -109.3111139716955194, -298.2784766785204056, -291.6440130419127286 ) ) ;
#17569 = CARTESIAN_POINT ( 'NONE',  ( -18.40112929506057426, -289.7434632275808326, -341.1575199974448651 ) ) ;
#17570 = EDGE_CURVE ( 'NONE', #50020, #14856, #86341, .T. ) ;
#17571 = EDGE_CURVE ( 'NONE', #77857, #31, #27591, .T. ) ;
#17572 = CARTESIAN_POINT ( 'NONE',  ( -61.84676131758235584, -279.3488433007075287, -341.6756634153824734 ) ) ;
#17573 = CARTESIAN_POINT ( 'NONE',  ( -86.85032266208642682, -276.5178237371862338, -328.8848325797329721 ) ) ;
#17574 = CARTESIAN_POINT ( 'NONE',  ( -52.51737664630387314, -273.2113978267725543, -194.9209980936768147 ) ) ;
#17575 = CARTESIAN_POINT ( 'NONE',  ( 35.89791776494042352, -279.8051600642812673, -283.7467905870917093 ) ) ;
#17576 = CARTESIAN_POINT ( 'NONE',  ( -72.48998852668894699, -275.9093293212183085, -337.9851243546137880 ) ) ;
#17577 = CARTESIAN_POINT ( 'NONE',  ( -96.81730069627408852, -294.6366040678423133, -313.5554710507019536 ) ) ;
#17578 = CARTESIAN_POINT ( 'NONE',  ( -60.82200480488018002, -275.7477713320995463, -199.0777475753787087 ) ) ;
#17579 = CARTESIAN_POINT ( 'NONE',  ( -35.15191628180505745, -298.8830887981370097, -197.1993321852654049 ) ) ;
#17580 = CARTESIAN_POINT ( 'NONE',  ( 194.4805735913283229, 26.12542652888812356, 14.33214477299284795 ) ) ;
#17582 = CARTESIAN_POINT ( 'NONE',  ( -38.08023040182426655, -273.8759625125530306, -197.3648538482133858 ) ) ;
#17581 = CARTESIAN_POINT ( 'NONE',  ( -79.63869437661979589, -287.6403044513306213, -332.7889907146593487 ) ) ;
#17583 = CARTESIAN_POINT ( 'NONE',  ( 0.7192939522333362534, -288.5595452132297396, -337.3568675169548783 ) ) ;
#17584 = CARTESIAN_POINT ( 'NONE',  ( -98.10055036839052889, -275.1549477452975907, -226.0210668610420157 ) ) ;
#17585 = CARTESIAN_POINT ( 'NONE',  ( -110.8416446690041397, -294.7338470644844506, -256.2293286010323641 ) ) ;
#17586 = CARTESIAN_POINT ( 'NONE',  ( -92.32534344588422925, -283.0115202022175822, -324.0356723619553350 ) ) ;
#17587 = CARTESIAN_POINT ( 'NONE',  ( 41.08708295871279859, -270.5084069056321141, -430.6442049081568939 ) ) ;
#17588 = CARTESIAN_POINT ( 'NONE',  ( 24.72548240771276440, -278.9818722485092053, -228.2353968721334354 ) ) ;
#17589 = CARTESIAN_POINT ( 'NONE',  ( 197.9510393857643180, 24.58358384448226630, 11.14414497126373860 ) ) ;
#17590 = CARTESIAN_POINT ( 'NONE',  ( -79.74767768327657791, -290.2597899866490252, -210.3917056528001694 ) ) ;
#17591 = CARTESIAN_POINT ( 'NONE',  ( -23.86409863191952496, -281.0177179328717898, -343.3626230054558732 ) ) ;
#17592 = DIRECTION ( 'NONE',  ( -0.000000000000000000, -1.000000000000000000, -0.000000000000000000 ) ) ;
#17593 = DIRECTION ( 'NONE',  ( -0.000000000000000000, 1.000000000000000000, -0.000000000000000000 ) ) ;
#17594 = CARTESIAN_POINT ( 'NONE',  ( -108.4599159734351588, -288.8598716074000663, -246.5451564612150719 ) ) ;
#17595 = CARTESIAN_POINT ( 'NONE',  ( 17.79151208367478532, -276.3793972487744668, -221.3873016889835128 ) ) ;
#17596 = CARTESIAN_POINT ( 'NONE',  ( -47.19003495194347408, -284.3797052228750317, -346.3283413034232012 ) ) ;
#17598 = CARTESIAN_POINT ( 'NONE',  ( -69.00916445148507705, -283.4805967386897692, -336.1485608028720549 ) ) ;
#17597 = CARTESIAN_POINT ( 'NONE',  ( -93.06643966019032632, -271.3395360653064472, -219.3119560265996597 ) ) ;
#17599 = CARTESIAN_POINT ( 'NONE',  ( 34.74539836981070096, -277.1710055054147119, -285.1538577177547609 ) ) ;
#17600 = CARTESIAN_POINT ( 'NONE',  ( 29.22873980964546803, -275.9452564596628577, -239.8909788744041975 ) ) ;
#17601 = CARTESIAN_POINT ( 'NONE',  ( 5.796042162565585798, -284.4680844852121027, -331.7771934716265605 ) ) ;
#17602 = EDGE_LOOP ( 'NONE', ( #44775, #13136, #57697 ) ) ;
#17603 = CARTESIAN_POINT ( 'NONE',  ( 204.2968234959853930, 292.4580586366143962, -53.99999999999221956 ) ) ;
#17604 = CARTESIAN_POINT ( 'NONE',  ( -33.43696022384644095, -294.8376238862369405, -347.2751672175621138 ) ) ;
#17605 = CARTESIAN_POINT ( 'NONE',  ( -40.05847396863813259, -287.9977322027883133, -195.7657699698966098 ) ) ;
#17606 = CARTESIAN_POINT ( 'NONE',  ( 197.2116943569230330, 275.0000000000000568, -12.42446933126074882 ) ) ;
#17607 = CARTESIAN_POINT ( 'NONE',  ( -99.86837403722181250, -288.6952119285918457, -220.4570493818173702 ) ) ;
#17608 = CARTESIAN_POINT ( 'NONE',  ( -89.11087932520128163, -276.9557470734431490, -327.1423728589171560 ) ) ;
#17609 = CARTESIAN_POINT ( 'NONE',  ( -53.20269626787620609, -290.2520618232817355, -195.7761941319945720 ) ) ;
#17610 = CARTESIAN_POINT ( 'NONE',  ( -92.04880742444235864, -286.7733887058387836, -220.9116240308455019 ) ) ;
#17611 = CARTESIAN_POINT ( 'NONE',  ( -96.06350241333637996, -279.6870949627451637, -315.4135757671613192 ) ) ;
#17612 = CARTESIAN_POINT ( 'NONE',  ( -40.80805155351878710, -287.4347538856222286, -193.9772171418615017 ) ) ;
#17613 = CARTESIAN_POINT ( 'NONE',  ( 34.89237758625882435, -283.8119169392057870, -290.5412732702028507 ) ) ;
#17614 = CARTESIAN_POINT ( 'NONE',  ( 16.95673149184141693, -276.4713462457476112, -325.0311802529481042 ) ) ;
#17615 = CARTESIAN_POINT ( 'NONE',  ( -82.54799658096474957, -277.4843043900669386, -332.6940207346409579 ) ) ;
#17616 = CARTESIAN_POINT ( 'NONE',  ( -93.85324223422927048, -299.1488582801878238, -221.8878161867566803 ) ) ;
#17617 = CARTESIAN_POINT ( 'NONE',  ( 159.2635086430408080, 16.19322481500758215, 10.13850573484278783 ) ) ;
#17618 = CARTESIAN_POINT ( 'NONE',  ( 21.31550574532285580, -278.6948066931273615, -317.0979686699210447 ) ) ;
#17619 = CARTESIAN_POINT ( 'NONE',  ( -97.24259044483734726, -295.3214412754409750, -223.9484999571485275 ) ) ;
#17620 = DIRECTION ( 'NONE',  ( -0.000000000000000000, -0.000000000000000000, 1.000000000000000000 ) ) ;
#17621 = CARTESIAN_POINT ( 'NONE',  ( -105.3273519283102360, -277.7022816625387804, -297.1181654807863879 ) ) ;
#17622 = CARTESIAN_POINT ( 'NONE',  ( -7.857672798845277917, -275.6349315123820816, -199.6033272883307177 ) ) ;
#17623 = CARTESIAN_POINT ( 'NONE',  ( 38.02596540867186548, -280.4280202092706418, -255.7825307694277512 ) ) ;
#17624 = CARTESIAN_POINT ( 'NONE',  ( 9.656927660583086492, -288.4694223126115844, -213.1850478405015110 ) ) ;
#17625 = CARTESIAN_POINT ( 'NONE',  ( -94.12259327859879932, -297.3741066089525020, -321.3574167657899920 ) ) ;
#17626 = CARTESIAN_POINT ( 'NONE',  ( -70.62141972905970988, -296.6862643438914233, -339.3717040882862079 ) ) ;
#17627 = CARTESIAN_POINT ( 'NONE',  ( -50.02387512309542217, -293.8902599616650377, -196.5576308607510896 ) ) ;
#17628 = CARTESIAN_POINT ( 'NONE',  ( 21.98458729161788483, -278.9256080531673661, -224.7286594058828371 ) ) ;
#17629 = CARTESIAN_POINT ( 'NONE',  ( 10.17734072955849811, -282.6330770578432521, -212.9942484425526743 ) ) ;
#17630 = CARTESIAN_POINT ( 'NONE',  ( -95.56257679745787925, -295.2744248083453726, -223.9753041816722146 ) ) ;
#17631 = CARTESIAN_POINT ( 'NONE',  ( -111.0954516566918215, -285.9094528261143751, -289.5654579535222410 ) ) ;
#17632 = EDGE_CURVE ( 'NONE', #23012, #9431, #50213, .T. ) ;
#17633 = CARTESIAN_POINT ( 'NONE',  ( 29.09586790816225843, -286.0558130400837626, -239.3728036355984727 ) ) ;
#17634 = CARTESIAN_POINT ( 'NONE',  ( 6.133466362344496936, -279.9740074315837433, -206.9322390316848157 ) ) ;
#17635 = CARTESIAN_POINT ( 'NONE',  ( -29.32149395268238479, -125.4031318350040891, -363.7124165658669881 ) ) ;
#17636 = EDGE_LOOP ( 'NONE', ( #81351, #74447, #32798, #66890 ) ) ;
#17637 = CARTESIAN_POINT ( 'NONE',  ( 32.69145310020566342, -286.9448490079262797, -249.6422584931054018 ) ) ;
#17638 = ORIENTED_EDGE ( 'NONE', *, *, #39759, .T. ) ;
#17639 = CARTESIAN_POINT ( 'NONE',  ( -96.02487318110094350, -284.9640772687168919, -319.7552888296561946 ) ) ;
#17640 = CARTESIAN_POINT ( 'NONE',  ( 7.340503886933810840, -275.0141102195086091, -212.6065672437735543 ) ) ;
#17641 = CARTESIAN_POINT ( 'NONE',  ( -49.26769202525431979, -284.6984497089737829, -194.6387801587113415 ) ) ;
#17642 = CARTESIAN_POINT ( 'NONE',  ( -73.27665556041465322, -290.5073833521827851, -202.5954748960363645 ) ) ;
#17643 = CARTESIAN_POINT ( 'NONE',  ( 12.82931170852911507, -281.6738949897509769, -212.2604313806997425 ) ) ;
#17644 = DIRECTION ( 'NONE',  ( 0.000000000000000000, 0.000000000000000000, 1.000000000000000000 ) ) ;
#17645 = CARTESIAN_POINT ( 'NONE',  ( -40.99474559807290319, -281.5271148272101414, -194.1288639248617471 ) ) ;
#17646 = CARTESIAN_POINT ( 'NONE',  ( 39.68926002210008619, -281.8799913415469405, -269.9261499705065148 ) ) ;
#17647 = CARTESIAN_POINT ( 'NONE',  ( -102.0455923789670294, -287.6237833571632905, -301.4846348637937581 ) ) ;
#17648 = CARTESIAN_POINT ( 'NONE',  ( -103.8349779299932152, -256.5568498903555792, -326.8183980474310601 ) ) ;
#17649 = VERTEX_POINT ( 'NONE', #29482 ) ;
#17650 = CARTESIAN_POINT ( 'NONE',  ( 33.84996063021831958, -277.8507559610383169, -293.4213839146042346 ) ) ;
#17651 = CARTESIAN_POINT ( 'NONE',  ( -110.7306624032010802, -265.9561541865978143, -306.7379753279722081 ) ) ;
#17652 = CARTESIAN_POINT ( 'NONE',  ( 35.95402134271872541, -279.3891321913799288, -256.1662435223460079 ) ) ;
#17653 = CARTESIAN_POINT ( 'NONE',  ( -72.88920365406468704, -296.9164125769060547, -206.4841451252907234 ) ) ;
#17654 = CARTESIAN_POINT ( 'NONE',  ( -70.86523179119832605, -291.1293228829475197, -201.1101271706874627 ) ) ;
#17655 = CARTESIAN_POINT ( 'NONE',  ( 180.7149167944524493, -12.49482340714361506, -3.999999999999998224 ) ) ;
#17657 = CARTESIAN_POINT ( 'NONE',  ( 20.98531840833684470, -285.3221071166516367, -225.1460836898898492 ) ) ;
#17656 = CARTESIAN_POINT ( 'NONE',  ( -65.30930134969403866, -296.2685389482138589, -199.1960651998306275 ) ) ;
#17658 = CARTESIAN_POINT ( 'NONE',  ( 22.33329217630785024, -296.0213409799287660, -314.5172135519637209 ) ) ;
#17659 = CARTESIAN_POINT ( 'NONE',  ( -71.42167675060044019, -286.9072998483213155, -205.2473815473493630 ) ) ;
#17660 = ORIENTED_EDGE ( 'NONE', *, *, #291, .T. ) ;
#17661 = CARTESIAN_POINT ( 'NONE',  ( 27.91225365938942815, -295.0249063270122178, -310.8929476730986039 ) ) ;
#17662 = CARTESIAN_POINT ( 'NONE',  ( -108.1513204925075655, -284.8071272311215125, -288.3607320252058912 ) ) ;
#17663 = CARTESIAN_POINT ( 'NONE',  ( -46.06932200116946063, -296.7387178400814491, -194.2569963170201106 ) ) ;
#17664 = CARTESIAN_POINT ( 'NONE',  ( 20.25086708675662805, -293.6645410333546806, -219.4761759203548195 ) ) ;
#17665 = CARTESIAN_POINT ( 'NONE',  ( -103.1664468090598774, -291.5659427370477488, -230.4258660393881826 ) ) ;
#17666 = CARTESIAN_POINT ( 'NONE',  ( -61.25300888706676972, -289.5381760259506336, -339.3339337720379945 ) ) ;
#17667 = ORIENTED_EDGE ( 'NONE', *, *, #54326, .F. ) ;
#17668 = CARTESIAN_POINT ( 'NONE',  ( 139.6539576904058606, 132.0000000000000568, -10.49999999999999822 ) ) ;
#17669 = CARTESIAN_POINT ( 'NONE',  ( -51.59190099714205502, -299.7323131751791152, -195.8950322800952506 ) ) ;
#17670 = CARTESIAN_POINT ( 'NONE',  ( -91.87556230996639783, -272.0898907607852948, -216.5645884134065113 ) ) ;
#17671 = CARTESIAN_POINT ( 'NONE',  ( -1.146107736160122847, -281.6178869853226843, -334.0265524014146763 ) ) ;
#17672 = ORIENTED_EDGE ( 'NONE', *, *, #6263, .F. ) ;
#17673 = CARTESIAN_POINT ( 'NONE',  ( -87.06020940125013396, -277.2304375771291802, -329.1470700126715201 ) ) ;
#17674 = CARTESIAN_POINT ( 'NONE',  ( -110.3714176747848370, -271.0953383341310996, -259.3776521411577392 ) ) ;
#17675 = CARTESIAN_POINT ( 'NONE',  ( -66.57761392687062596, -281.5255483142537969, -202.1114281615460300 ) ) ;
#17676 = CARTESIAN_POINT ( 'NONE',  ( 8.321853300821368649, -274.5596669924367461, -328.9561286365883461 ) ) ;
#17677 = ADVANCED_FACE ( 'NONE', ( #93395 ), #60842, .T. ) ;
#17678 = CARTESIAN_POINT ( 'NONE',  ( -108.6813437575163448, -297.5301244360953774, -287.6705433096478828 ) ) ;
#17679 = CARTESIAN_POINT ( 'NONE',  ( -100.1687726011513035, -298.1505643338160780, -232.4869132194841370 ) ) ;
#17680 = CARTESIAN_POINT ( 'NONE',  ( -110.0559311812380798, -298.4435442172528496, -247.4027046910749732 ) ) ;
#17681 = CARTESIAN_POINT ( 'NONE',  ( 20.60261249216338442, -272.9102088506251107, -222.1857773883080256 ) ) ;
#17682 = CARTESIAN_POINT ( 'NONE',  ( 33.74494510461933316, -293.9783495547694656, -253.2612146701854101 ) ) ;
#17683 = CARTESIAN_POINT ( 'NONE',  ( 32.36498716322867608, -291.8141178373648472, -246.6152450996182210 ) ) ;
#17684 = DIRECTION ( 'NONE',  ( -0.000000000000000000, 1.000000000000000000, -0.000000000000000000 ) ) ;
#17685 = CARTESIAN_POINT ( 'NONE',  ( 18.04094024406537855, -275.3119379607195469, -216.8778110723447412 ) ) ;
#17686 = EDGE_CURVE ( 'NONE', #16590, #63583, #35149, .T. ) ;
#17687 = CARTESIAN_POINT ( 'NONE',  ( -107.1971508084990887, -273.0015397566239130, -248.9932279303020550 ) ) ;
#17688 = EDGE_CURVE ( 'NONE', #59928, #3752, #18439, .T. ) ;
#17689 = CARTESIAN_POINT ( 'NONE',  ( -58.36740504657306872, -282.0030912873896796, -343.9772460047602749 ) ) ;
#17690 = CARTESIAN_POINT ( 'NONE',  ( 206.6110850237746490, 1.019348808636641568, -7.290232558141295449 ) ) ;
#17691 = CARTESIAN_POINT ( 'NONE',  ( -70.29679799779499660, -282.6951431472427885, -335.6940631539447963 ) ) ;
#17692 = CARTESIAN_POINT ( 'NONE',  ( -52.57165735092634407, -281.2465061577509573, -344.0219031879252611 ) ) ;
#17693 = CARTESIAN_POINT ( 'NONE',  ( 34.70189891626354495, -273.9297394749829664, -255.2963710662131120 ) ) ;
#17694 = CARTESIAN_POINT ( 'NONE',  ( 34.96609505648138594, -283.8089800578763970, -290.3229119254758643 ) ) ;
#17695 = CARTESIAN_POINT ( 'NONE',  ( 209.3504981911156335, 1.050453206927881578, 7.446924052135294403 ) ) ;
#17696 = CARTESIAN_POINT ( 'NONE',  ( 156.4217629211117355, 119.0463968525363327, 7.000000000000000000 ) ) ;
#17697 = CARTESIAN_POINT ( 'NONE',  ( -34.11644831687502943, -272.4919584861413568, -194.2294020716536238 ) ) ;
#17698 = CARTESIAN_POINT ( 'NONE',  ( -112.3999288486476189, -280.5006066881134643, -274.3972950378903306 ) ) ;
#17699 = PLANE ( 'NONE',  #30210 ) ;
#17700 = CARTESIAN_POINT ( 'NONE',  ( -85.17160331915195570, -285.6269433390694417, -328.8556865841721901 ) ) ;
#17701 = CARTESIAN_POINT ( 'NONE',  ( 200.4871970924806419, 61.71654497095076408, 9.999999999999998224 ) ) ;
#17702 = CARTESIAN_POINT ( 'NONE',  ( -110.3148300015880068, -288.3289346875240540, -287.7336675289198524 ) ) ;
#17703 = DIRECTION ( 'NONE',  ( 0.000000000000000000, 0.000000000000000000, 1.000000000000000000 ) ) ;
#17704 = CARTESIAN_POINT ( 'NONE',  ( -107.9891537345519765, -295.0854200283829982, -290.2625703017852743 ) ) ;
#17705 = CARTESIAN_POINT ( 'NONE',  ( -95.93996395916997244, -288.0601211273924491, -315.9569754350310973 ) ) ;
#17706 = CARTESIAN_POINT ( 'NONE',  ( -117.0946091816712453, -269.6096274233381109, -270.3236525939013859 ) ) ;
#17707 = CARTESIAN_POINT ( 'NONE',  ( -112.0398673256333097, -294.6454663220733892, -263.0808577613462376 ) ) ;
#17708 = CARTESIAN_POINT ( 'NONE',  ( 2.798800585097338534, -287.0042363100206444, -335.3187633961321694 ) ) ;
#17709 = CARTESIAN_POINT ( 'NONE',  ( 0.7961079936739583474, -282.1697093603694384, -207.1201059404870648 ) ) ;
#17710 = CARTESIAN_POINT ( 'NONE',  ( -16.44234836096939389, -281.0256802891428265, -343.4717528126160460 ) ) ;
#17711 = CARTESIAN_POINT ( 'NONE',  ( 10.11526302078678619, -288.3766170477246078, -325.8971964888217485 ) ) ;
#17712 = CARTESIAN_POINT ( 'NONE',  ( 29.85989559455946818, -283.3794908267593655, -300.4749768059178336 ) ) ;
#17713 = CARTESIAN_POINT ( 'NONE',  ( 19.48391776830431610, -283.0057355178621492, -316.4617847527654817 ) ) ;
#17714 = CARTESIAN_POINT ( 'NONE',  ( 31.20512715447165064, -289.1217149490772158, -238.9348096278522746 ) ) ;
#17715 = CARTESIAN_POINT ( 'NONE',  ( -80.62677572701804252, -297.6498053103783263, -206.6149693722878737 ) ) ;
#17716 = CARTESIAN_POINT ( 'NONE',  ( -21.35479054832686430, -274.2517471427060514, -195.0390181572846018 ) ) ;
#17717 = CARTESIAN_POINT ( 'NONE',  ( -22.43628846829315648, -294.2238390051361989, -197.2196420411085001 ) ) ;
#17718 = FACE_OUTER_BOUND ( 'NONE', #70423, .T. ) ;
#17719 = CARTESIAN_POINT ( 'NONE',  ( -95.95921662488163406, -280.4090924074130839, -317.1477375740089997 ) ) ;
#17720 = ORIENTED_EDGE ( 'NONE', *, *, #60067, .F. ) ;
#17721 = CARTESIAN_POINT ( 'NONE',  ( -12.49677587509686383, -274.7297834191364245, -341.3576404100920172 ) ) ;
#17722 = CARTESIAN_POINT ( 'NONE',  ( 197.3534831049100831, 70.40830473911788090, 11.81087581402289466 ) ) ;
#17723 = CARTESIAN_POINT ( 'NONE',  ( -113.3214010048881875, -295.0334561552160721, -263.9176088293445446 ) ) ;
#17724 = CARTESIAN_POINT ( 'NONE',  ( -29.97135204591434743, -273.4964847907365311, -197.6316835197017667 ) ) ;
#17725 = CARTESIAN_POINT ( 'NONE',  ( -94.63118473278014164, -291.4227757615917653, -316.7143563632914720 ) ) ;
#17726 = CARTESIAN_POINT ( 'NONE',  ( -92.74232247938222429, -292.1736885089243287, -222.4635241837306410 ) ) ;
#17727 = CARTESIAN_POINT ( 'NONE',  ( -1.924309616885777841, -284.3364837601328645, -335.3647026359278698 ) ) ;
#17728 = CARTESIAN_POINT ( 'NONE',  ( -113.0845722507409903, -292.1093589700644202, -259.8922154418312402 ) ) ;
#17729 = CARTESIAN_POINT ( 'NONE',  ( -1.052632141082161077, -293.8387203449771619, -203.0083020189727279 ) ) ;
#17730 = CARTESIAN_POINT ( 'NONE',  ( -50.47329019489183111, -295.0578508532300930, -342.1703189724210574 ) ) ;
#17731 = CARTESIAN_POINT ( 'NONE',  ( 33.72787448323956028, -289.2424871893406362, -246.4003956917890150 ) ) ;
#17732 = CARTESIAN_POINT ( 'NONE',  ( -2.890936421800040179, -282.7762008881508677, -339.2390045673786858 ) ) ;
#17733 = CARTESIAN_POINT ( 'NONE',  ( -111.7894443477939319, -294.4636028563085688, -283.5742726090718975 ) ) ;
#17734 = CARTESIAN_POINT ( 'NONE',  ( -44.42132949944037534, -282.9725524954667435, -347.0883227273838543 ) ) ;
#17735 = CARTESIAN_POINT ( 'NONE',  ( 34.09773391867471304, -277.8127698190616002, -292.0446562364148804 ) ) ;
#17736 = CARTESIAN_POINT ( 'NONE',  ( -3.112352779071856812, -284.5041144407283582, -203.6133033453804444 ) ) ;
#17737 = CARTESIAN_POINT ( 'NONE',  ( -12.29720411840080097, -274.8695054448504607, -341.9219351106789873 ) ) ;
#17738 = DIRECTION ( 'NONE',  ( -1.000000000000000000, 0.000000000000000000, 0.000000000000000000 ) ) ;
#17739 = CARTESIAN_POINT ( 'NONE',  ( 13.96343427941700632, -281.8163053036024621, -322.4493760913728124 ) ) ;
#17740 = CARTESIAN_POINT ( 'NONE',  ( -33.94829648898074481, -281.2990232641605530, -193.8333875115237959 ) ) ;
#17741 = CARTESIAN_POINT ( 'NONE',  ( 36.46832320789222592, -286.3435441246020332, -249.0795967653575929 ) ) ;
#17742 = CARTESIAN_POINT ( 'NONE',  ( 5.066164061071487978, -294.3939564883672233, -209.6390351055500787 ) ) ;
#17743 = CARTESIAN_POINT ( 'NONE',  ( 38.83060425639602187, -277.1263172982480114, -268.3067426007121981 ) ) ;
#17744 = CARTESIAN_POINT ( 'NONE',  ( 36.76526535727481360, -277.1067776853337250, -289.3731126372894096 ) ) ;
#17745 = CARTESIAN_POINT ( 'NONE',  ( -110.2802261272020274, -278.3459589253014315, -273.3563524575844212 ) ) ;
#17746 = CARTESIAN_POINT ( 'NONE',  ( -53.04402875454506727, -299.8507008681648358, -197.1405474645553966 ) ) ;
#17747 = CARTESIAN_POINT ( 'NONE',  ( 23.49656973147837391, -284.9568857992414337, -226.6992580576661283 ) ) ;
#17748 = CARTESIAN_POINT ( 'NONE',  ( 19.51119775226462849, -293.9253648607297009, -322.3376204120130524 ) ) ;
#17749 = CARTESIAN_POINT ( 'NONE',  ( -113.5893940586632027, -292.1411720431717072, -271.2400806128175077 ) ) ;
#17750 = CARTESIAN_POINT ( 'NONE',  ( 31.12196087148551982, -292.1239159680870898, -244.1513260037536952 ) ) ;
#17751 = ORIENTED_EDGE ( 'NONE', *, *, #67910, .T. ) ;
#17752 = CARTESIAN_POINT ( 'NONE',  ( -20.06304599662741239, -291.9469558478332374, -199.3614184540020631 ) ) ;
#17753 = VERTEX_POINT ( 'NONE', #29007 ) ;
#17754 = CARTESIAN_POINT ( 'NONE',  ( 7.763859992516961128, -289.5322511306217166, -332.4506485357376278 ) ) ;
#17755 = CARTESIAN_POINT ( 'NONE',  ( -35.66877213859904572, -280.7250724815806961, -197.2659092102464342 ) ) ;
#17756 = CARTESIAN_POINT ( 'NONE',  ( -97.09681548444250154, -296.1193449961528472, -222.2901423307159519 ) ) ;
#17757 = CARTESIAN_POINT ( 'NONE',  ( 22.90684029761423801, -287.5630349142196565, -222.5549246932329197 ) ) ;
#17758 = CARTESIAN_POINT ( 'NONE',  ( 37.35528158426782852, -287.6526170707588790, -251.7572147712762671 ) ) ;
#17759 = CARTESIAN_POINT ( 'NONE',  ( -107.7804260445666102, -284.6306542899195051, -289.6560006776313116 ) ) ;
#17760 = CARTESIAN_POINT ( 'NONE',  ( -112.7013083777456330, -271.1594590305112433, -296.3539449067754390 ) ) ;
#17761 = CARTESIAN_POINT ( 'NONE',  ( -108.3564486399562412, -260.6790360280811569, -316.7380296206242747 ) ) ;
#17762 = CARTESIAN_POINT ( 'NONE',  ( 201.5605854984582663, 292.5235874916616581, -68.22477292250835035 ) ) ;
#17763 = CARTESIAN_POINT ( 'NONE',  ( 18.42487748536285608, -275.4212177974885094, -317.7181718254829548 ) ) ;
#17764 = CARTESIAN_POINT ( 'NONE',  ( 36.00789036824063061, -274.4887990777709774, -271.6038690425473305 ) ) ;
#17765 = CARTESIAN_POINT ( 'NONE',  ( -113.8411827663665576, -272.3261748891251841, -261.7836214039719493 ) ) ;
#17766 = CARTESIAN_POINT ( 'NONE',  ( 203.5339397030482189, 292.0436732951557701, -68.28815551792725103 ) ) ;
#17767 = CARTESIAN_POINT ( 'NONE',  ( -4.223575908080033692, -275.3095016481788093, -339.3428195689347717 ) ) ;
#17768 = CARTESIAN_POINT ( 'NONE',  ( -43.58970876774290559, -275.7324274079122688, -196.5605576942260484 ) ) ;
#17769 = VERTEX_POINT ( 'NONE', #72560 ) ;
#17770 = CARTESIAN_POINT ( 'NONE',  ( -69.99432313723040977, -289.9866398203401445, -335.7339556616880714 ) ) ;
#17771 = CARTESIAN_POINT ( 'NONE',  ( -109.7022403020554577, -297.6819397677380152, -244.5132738567006072 ) ) ;
#17772 = CARTESIAN_POINT ( 'NONE',  ( -85.18305597396116013, -297.9037045220665618, -210.1055657580390630 ) ) ;
#17773 = CARTESIAN_POINT ( 'NONE',  ( -55.80126008196373988, -295.4630507210210340, -341.0410072046119012 ) ) ;
#17774 = EDGE_LOOP ( 'NONE', ( #964, #51053, #54340, #34403 ) ) ;
#17775 = CARTESIAN_POINT ( 'NONE',  ( -94.11240937194851597, -279.7846083622071092, -320.2249402561186571 ) ) ;
#17776 = ADVANCED_FACE ( 'NONE', ( #51231 ), #36636, .T. ) ;
#17777 = CARTESIAN_POINT ( 'NONE',  ( 39.57938809120850721, -281.0185663768605764, -267.0662712064930702 ) ) ;
#17778 = CARTESIAN_POINT ( 'NONE',  ( -100.8437493448315934, -279.1304673795540907, -307.0924776408278376 ) ) ;
#17779 = CARTESIAN_POINT ( 'NONE',  ( -14.86772463289301527, -278.5251861102902922, -343.0033648326723323 ) ) ;
#17780 = CARTESIAN_POINT ( 'NONE',  ( -101.7213526399206103, -295.6101781062986902, -234.7151468470400744 ) ) ;
#17781 = CARTESIAN_POINT ( 'NONE',  ( 219.7099725226080977, -142.7221692137691775, -1.978481845683818907 ) ) ;
#17782 = ADVANCED_FACE ( 'NONE', ( #32255 ), #38099, .T. ) ;
#17783 = CARTESIAN_POINT ( 'NONE',  ( -110.3919245767296502, -278.7151521488672756, -270.6401720130731405 ) ) ;
#17784 = CARTESIAN_POINT ( 'NONE',  ( -7.762213384313215059, -275.2327533195534670, -199.3877004573737395 ) ) ;
#17785 = CARTESIAN_POINT ( 'NONE',  ( -48.81170910836917898, -287.8800048916109517, -346.0568836833317619 ) ) ;
#17786 = CARTESIAN_POINT ( 'NONE',  ( -69.30323031890370089, -275.6318797607426632, -202.4982656123123945 ) ) ;
#17787 = CARTESIAN_POINT ( 'NONE',  ( 38.15070460945472774, -274.2799164297738912, -282.5038458828271359 ) ) ;
#17788 = LINE ( 'NONE', #3576, #29340 ) ;
#17789 = CARTESIAN_POINT ( 'NONE',  ( -95.90370837899199330, -289.1348904764423082, -314.2351120136659688 ) ) ;
#17790 = CARTESIAN_POINT ( 'NONE',  ( -76.04822907539227117, -284.8982021472038468, -203.8534527296125987 ) ) ;
#17791 = CARTESIAN_POINT ( 'NONE',  ( -13.22000077407985685, -280.9744824399166419, -340.3877236193171143 ) ) ;
#17793 = CARTESIAN_POINT ( 'NONE',  ( -77.81182374204136920, -283.5842397628268827, -207.8221080490869781 ) ) ;
#17792 = CARTESIAN_POINT ( 'NONE',  ( 26.05752155882104404, -280.6371631298986244, -307.8236974248523552 ) ) ;
#17794 = CARTESIAN_POINT ( 'NONE',  ( 12.60499006191922788, -290.3565190197821266, -326.3792900967713990 ) ) ;
#17795 = CARTESIAN_POINT ( 'NONE',  ( -107.4916046095127200, -279.4707790256399562, -292.1210325950855236 ) ) ;
#17796 = PLANE ( 'NONE',  #80542 ) ;
#17797 = CARTESIAN_POINT ( 'NONE',  ( 32.82126330089431576, -280.3358637658288330, -300.2211750137091144 ) ) ;
#17798 = CARTESIAN_POINT ( 'NONE',  ( 32.58854498080377482, -295.1980916641944646, -243.1112403593733120 ) ) ;
#17799 = CARTESIAN_POINT ( 'NONE',  ( -109.5792601793995118, -277.0944433828132105, -246.6207923682664216 ) ) ;
#17800 = CARTESIAN_POINT ( 'NONE',  ( -82.75481009332455073, -285.6710795534855265, -330.3237122468634084 ) ) ;
#17801 = CARTESIAN_POINT ( 'NONE',  ( 201.2104617360081704, 25.32700003806615996, 10.00000000000000000 ) ) ;
#17802 = CARTESIAN_POINT ( 'NONE',  ( -112.9289674395089378, -292.4970901128252194, -268.4166340671497437 ) ) ;
#17803 = CARTESIAN_POINT ( 'NONE',  ( 36.53880701214865212, -286.4819411836165273, -249.0574248363113270 ) ) ;
#17804 = CARTESIAN_POINT ( 'NONE',  ( -107.7589061983304788, -289.2420863045257420, -248.2310885533853480 ) ) ;
#17805 = CARTESIAN_POINT ( 'NONE',  ( -48.18343439339133027, -279.1637174034569284, -435.8377362500897902 ) ) ;
#17806 = CARTESIAN_POINT ( 'NONE',  ( 36.13629455319700412, -274.2174135372637238, -268.8685449644514733 ) ) ;
#17807 = CARTESIAN_POINT ( 'NONE',  ( -23.30816682774668891, -293.0105356823012244, -343.3102691443972390 ) ) ;
#17808 = CARTESIAN_POINT ( 'NONE',  ( 165.2494399300530290, 8.542400036368780647, 13.00000000000000178 ) ) ;
#17809 = CARTESIAN_POINT ( 'NONE',  ( 197.4288403404171959, 41.88980437486001307, 11.72798125285450332 ) ) ;
#17810 = CARTESIAN_POINT ( 'NONE',  ( 34.80349393727056651, -291.7140716903027169, -245.3458976984586286 ) ) ;
#17811 = CARTESIAN_POINT ( 'NONE',  ( -38.65940762213166693, -287.6355219465610844, -196.5602618129810537 ) ) ;
#17812 = CARTESIAN_POINT ( 'NONE',  ( -73.95893579426329723, -287.7714655530916161, -336.9578954560478792 ) ) ;
#17813 = CARTESIAN_POINT ( 'NONE',  ( -27.77780136780434006, -287.6012640409599612, -197.3960115495131902 ) ) ;
#17814 = DIRECTION ( 'NONE',  ( 0.000000000000000000, 0.000000000000000000, -1.000000000000000000 ) ) ;
#17815 = CARTESIAN_POINT ( 'NONE',  ( 31.99036457150398505, -288.0453523541719392, -247.0016117508360480 ) ) ;
#17816 = CARTESIAN_POINT ( 'NONE',  ( 30.68993463090458462, -295.1061912378903571, -237.8346389110484722 ) ) ;
#17817 = CARTESIAN_POINT ( 'NONE',  ( 194.7510731661265595, -143.7221692137691775, 21.50000000000000000 ) ) ;
#17818 = CARTESIAN_POINT ( 'NONE',  ( 21.77391092965908825, -288.0992556379646317, -221.6440444926696500 ) ) ;
#17819 = CARTESIAN_POINT ( 'NONE',  ( -61.96036808352577197, -275.4494254994771154, -341.8533129174110741 ) ) ;
#17820 = CARTESIAN_POINT ( 'NONE',  ( -80.21088674958232900, -277.9483797814314130, -334.3625740726946560 ) ) ;
#17821 = ORIENTED_EDGE ( 'NONE', *, *, #291, .F. ) ;
#17822 = CARTESIAN_POINT ( 'NONE',  ( -16.99051278330689740, -290.3927826601469064, -197.5933822124611083 ) ) ;
#17823 = CARTESIAN_POINT ( 'NONE',  ( -94.96178988952230782, -279.2441756305032641, -219.2834784924319251 ) ) ;
#17824 = CARTESIAN_POINT ( 'NONE',  ( -94.00916981728916255, -299.2085867525287313, -221.7549831944050993 ) ) ;
#17825 = CARTESIAN_POINT ( 'NONE',  ( -48.18343439339133027, -269.7890444396509793, -499.6173591253298127 ) ) ;
#17826 = CARTESIAN_POINT ( 'NONE',  ( -108.4197741028974349, -282.8633569967754511, -246.2631681985445198 ) ) ;
#17827 = EDGE_CURVE ( 'NONE', #26935, #52628, #88604, .T. ) ;
#17828 = CARTESIAN_POINT ( 'NONE',  ( -48.18343439339133027, -262.5501068226030839, -494.5729214566502492 ) ) ;
#17829 = CARTESIAN_POINT ( 'NONE',  ( -111.3890742955827022, -276.7601902350255045, -265.0836321121481660 ) ) ;
#17830 = CARTESIAN_POINT ( 'NONE',  ( 31.35160356192858444, -279.1578583464187773, -240.2574525251123987 ) ) ;
#17831 = CARTESIAN_POINT ( 'NONE',  ( -54.94434090351493438, -285.8906705383787994, 54.50000000000000711 ) ) ;
#17832 = CARTESIAN_POINT ( 'NONE',  ( 12.23930627921130920, -274.8563713899467871, -328.3648381615888638 ) ) ;
#17833 = CARTESIAN_POINT ( 'NONE',  ( -88.97394391291211946, -297.3136534890559801, -323.0143604032419944 ) ) ;
#17834 = CARTESIAN_POINT ( 'NONE',  ( -66.47162356621498702, -282.3451124456813091, -341.3184654210264739 ) ) ;
#17835 = CARTESIAN_POINT ( 'NONE',  ( -82.09735401828436352, -298.3662192843175944, -212.3283994760195412 ) ) ;
#17836 = CARTESIAN_POINT ( 'NONE',  ( -113.2872878658722300, -297.9837553270439798, -261.1109301218626229 ) ) ;
#17837 = CARTESIAN_POINT ( 'NONE',  ( -19.26228503191035202, -273.9578373196731604, -199.5610796301048140 ) ) ;
#17838 = CARTESIAN_POINT ( 'NONE',  ( 37.52953047237122775, -295.4854416473697825, -265.1527522131964361 ) ) ;
#17839 = CARTESIAN_POINT ( 'NONE',  ( 19.62567604681163402, -288.4230589538124150, -322.1853722743121580 ) ) ;
#17840 = CARTESIAN_POINT ( 'NONE',  ( -112.2855505907938181, -276.7597884635018772, -260.3342467771904580 ) ) ;
#17841 = CARTESIAN_POINT ( 'NONE',  ( -98.34696146254658800, -291.0126312216229962, -223.3572542702410715 ) ) ;
#17842 = CARTESIAN_POINT ( 'NONE',  ( 29.63540557068274595, -287.0097712819272147, -300.1091083374892037 ) ) ;
#17843 = AXIS2_PLACEMENT_3D ( 'NONE', #39353, #68271, #3393 ) ;
#17844 = CARTESIAN_POINT ( 'NONE',  ( -67.50053590734492559, -289.6564177026513676, -201.6780268868807298 ) ) ;
#17845 = ORIENTED_EDGE ( 'NONE', *, *, #17507, .T. ) ;
#17846 = CARTESIAN_POINT ( 'NONE',  ( 201.7194887906492795, 294.2213704821156739, -83.28174295417332473 ) ) ;
#17847 = CARTESIAN_POINT ( 'NONE',  ( -75.90653936328065754, -289.0901101615197035, -332.4154620398738871 ) ) ;
#17848 = CARTESIAN_POINT ( 'NONE',  ( 208.8901450372919442, 29.13786557026924839, 13.14640446942321539 ) ) ;
#17849 = CARTESIAN_POINT ( 'NONE',  ( -67.77700842209684140, -284.3831914922274677, -340.8346039365395086 ) ) ;
#17850 = CARTESIAN_POINT ( 'NONE',  ( 39.47617173764678000, -292.6104118191377097, -270.3220790589136300 ) ) ;
#17851 = CARTESIAN_POINT ( 'NONE',  ( 18.55927979783339765, -282.4394403096026167, -218.5777146674589062 ) ) ;
#17852 = CARTESIAN_POINT ( 'NONE',  ( 22.47916806744032669, -282.2244053468974130, -222.6458313036172001 ) ) ;
#17853 = CARTESIAN_POINT ( 'NONE',  ( -37.54265456413710211, -282.8880918631435861, -343.3732708148669985 ) ) ;
#17854 = CARTESIAN_POINT ( 'NONE',  ( -113.2038780994886338, -296.3834467473143377, -283.8506665897165249 ) ) ;
#17855 = CARTESIAN_POINT ( 'NONE',  ( -13.92405418389636651, -275.6776531361581988, -200.6986651414621008 ) ) ;
#17856 = CARTESIAN_POINT ( 'NONE',  ( -68.46450504575271623, -289.6613386426316197, -202.5000590882436029 ) ) ;
#17857 = CARTESIAN_POINT ( 'NONE',  ( -110.5838718324912691, -271.4191342215616487, -264.8685366628302518 ) ) ;
#17858 = ORIENTED_EDGE ( 'NONE', *, *, #31125, .F. ) ;
#17859 = FACE_OUTER_BOUND ( 'NONE', #80476, .T. ) ;
#17860 = CARTESIAN_POINT ( 'NONE',  ( -96.10864961828872310, -287.1038208322881928, -224.6484012227728329 ) ) ;
#17861 = CARTESIAN_POINT ( 'NONE',  ( -2.097246812907239910, -295.6762117236767722, -338.4736793880846903 ) ) ;
#17862 = CARTESIAN_POINT ( 'NONE',  ( -98.19651279018879109, -285.7650456333064994, -229.8569892538839383 ) ) ;
#17863 = CARTESIAN_POINT ( 'NONE',  ( 14.71478924110950892, -275.3993183041594648, -326.8510239473284287 ) ) ;
#17864 = CARTESIAN_POINT ( 'NONE',  ( 37.68630615537986017, -294.4153881692369055, -287.2761744134524520 ) ) ;
#17865 = CARTESIAN_POINT ( 'NONE',  ( 22.03882654398868013, -285.0516125766982327, -223.2845220377510316 ) ) ;
#17866 = CARTESIAN_POINT ( 'NONE',  ( -72.16649807255318194, -291.9375431129384424, -201.6953917857080398 ) ) ;
#17867 = CARTESIAN_POINT ( 'NONE',  ( -56.06691911712367471, -289.6332004899992967, -340.9931032738587078 ) ) ;
#17868 = DIRECTION ( 'NONE',  ( 0.000000000000000000, 1.000000000000000000, -0.000000000000000000 ) ) ;
#17869 = CARTESIAN_POINT ( 'NONE',  ( 222.8344101925596306, -44.55766379199612004, 21.50000000000000000 ) ) ;
#17870 = CARTESIAN_POINT ( 'NONE',  ( 202.6187423002989760, 291.9839001675061354, -68.23006720443765971 ) ) ;
#17871 = CARTESIAN_POINT ( 'NONE',  ( -112.3206975191757664, -286.2545543845835141, -255.9133864947453674 ) ) ;
#17872 = CARTESIAN_POINT ( 'NONE',  ( -88.47809603358389552, -276.9094976428775681, -206.1857440867352693 ) ) ;
#17873 = VERTEX_POINT ( 'NONE', #23752 ) ;
#17874 = CARTESIAN_POINT ( 'NONE',  ( -29.42487889863111761, -281.8699822111988169, -343.2922167462845664 ) ) ;
#17875 = CARTESIAN_POINT ( 'NONE',  ( -113.2149299087082710, -278.3814987222999662, -257.3612220517189826 ) ) ;
#17876 = CARTESIAN_POINT ( 'NONE',  ( -77.83478494667707537, -281.5074748238621964, -207.3681125572547046 ) ) ;
#17877 = CARTESIAN_POINT ( 'NONE',  ( 140.6823888433080185, 178.4315446074800775, -239.9256222415464208 ) ) ;
#17878 = CARTESIAN_POINT ( 'NONE',  ( -67.66434415870708108, -282.0170496562066091, -340.4977243517851093 ) ) ;
#17879 = CARTESIAN_POINT ( 'NONE',  ( 29.13416963295219375, -285.1198088678092972, -236.2940885028409070 ) ) ;
#17880 = CARTESIAN_POINT ( 'NONE',  ( -109.8618611376048761, -274.6944470158696276, -248.2468764230110025 ) ) ;
#17881 = CARTESIAN_POINT ( 'NONE',  ( -92.23276838147855017, -296.3567580256465135, -318.5789473383214272 ) ) ;
#17882 = ORIENTED_EDGE ( 'NONE', *, *, #17917, .T. ) ;
#17883 = CARTESIAN_POINT ( 'NONE',  ( 6.986933163425442572, -291.3550503286494404, -211.7418741532002002 ) ) ;
#17884 = CARTESIAN_POINT ( 'NONE',  ( -34.28682982873007035, -277.6660963884695548, -347.1984822937913577 ) ) ;
#17885 = CARTESIAN_POINT ( 'NONE',  ( -40.77494098136474321, -274.0079063102132864, -197.3921958657863343 ) ) ;
#17886 = CARTESIAN_POINT ( 'NONE',  ( 39.31379013062058192, -274.5187136260051943, -274.0428914934993827 ) ) ;
#17887 = LINE ( 'NONE', #83198, #5306 ) ;
#17888 = CARTESIAN_POINT ( 'NONE',  ( -94.68934645725113342, -271.2205475670941723, -222.0067555394310261 ) ) ;
#17889 = CARTESIAN_POINT ( 'NONE',  ( -55.90940225614659909, -296.7119844954328869, -344.4816058991301020 ) ) ;
#17890 = ADVANCED_FACE ( 'NONE', ( #75344 ), #20364, .F. ) ;
#17891 = CARTESIAN_POINT ( 'NONE',  ( 180.2835393005426283, 214.8829713991971744, -24.64732457002850552 ) ) ;
#17892 = CARTESIAN_POINT ( 'NONE',  ( -43.47559602926583722, -255.2571177548196317, -494.0444526766419813 ) ) ;
#17893 = CARTESIAN_POINT ( 'NONE',  ( -105.8587019241274021, -285.9784302318867049, -244.2910865683883230 ) ) ;
#17894 = CARTESIAN_POINT ( 'NONE',  ( 28.88980644139570231, -283.8031981469814582, -307.7157132501973820 ) ) ;
#17895 = CARTESIAN_POINT ( 'NONE',  ( -104.2098807475242950, -283.5037726830101974, -299.8998906126874999 ) ) ;
#17896 = CARTESIAN_POINT ( 'NONE',  ( -26.92855561026095756, -275.3174022520358903, -343.4227825891136376 ) ) ;
#17897 = CARTESIAN_POINT ( 'NONE',  ( -38.88743911569032718, -284.9321276517055139, -344.5929297332987744 ) ) ;
#17898 = CARTESIAN_POINT ( 'NONE',  ( -108.8495197728233705, -276.7985453130717701, -288.2272198505789902 ) ) ;
#17899 = CARTESIAN_POINT ( 'NONE',  ( -31.32800131403647725, -275.2095288573261200, -197.2863761609956725 ) ) ;
#17900 = CARTESIAN_POINT ( 'NONE',  ( 138.6539576904058606, 132.0000000000000568, 12.50000000000000000 ) ) ;
#17901 = CARTESIAN_POINT ( 'NONE',  ( -48.10629391742389771, -280.7214930502006496, -194.2266236132717268 ) ) ;
#17902 = ORIENTED_EDGE ( 'NONE', *, *, #41688, .T. ) ;
#17903 = CARTESIAN_POINT ( 'NONE',  ( 199.3270723581583468, 16.88338937786772931, 10.34008960743410377 ) ) ;
#17904 = CARTESIAN_POINT ( 'NONE',  ( -43.58843769956197889, -287.8345778333856515, -194.8018668970822205 ) ) ;
#17905 = CARTESIAN_POINT ( 'NONE',  ( -3.077160550970305053, -293.7843424804066217, -335.0027690669103890 ) ) ;
#17906 = EDGE_CURVE ( 'NONE', #60755, #75996, #91005, .T. ) ;
#17907 = CARTESIAN_POINT ( 'NONE',  ( -112.5385412501642719, -290.1029234668242225, -254.2133834058313369 ) ) ;
#17908 = CARTESIAN_POINT ( 'NONE',  ( -7.830588247316364381, -284.6841226726079412, -202.4857300217522891 ) ) ;
#17910 = CARTESIAN_POINT ( 'NONE',  ( -77.79046375480390907, -289.7405051465075871, -208.3782854139334972 ) ) ;
#17909 = CARTESIAN_POINT ( 'NONE',  ( 26.89048318388064729, -285.6383751426846516, -234.3457915549133759 ) ) ;
#17911 = VECTOR ( 'NONE', #55668, 1000.000000000000000 ) ;
#17912 = CARTESIAN_POINT ( 'NONE',  ( -110.7150508492322700, -285.7138046583366418, -273.6712645020565446 ) ) ;
#17913 = CARTESIAN_POINT ( 'NONE',  ( -74.37149863358020241, -275.5444467015143459, -335.5822393489199840 ) ) ;
#17914 = CARTESIAN_POINT ( 'NONE',  ( 36.72197811232332754, -286.1791198311559583, -288.3329846976881186 ) ) ;
#17915 = CARTESIAN_POINT ( 'NONE',  ( -35.23073474381349257, -288.0787840962679525, -195.3780250453162637 ) ) ;
#17916 = CARTESIAN_POINT ( 'NONE',  ( 37.86769054303137239, -285.5671982581714019, -271.5483714285646784 ) ) ;
#17917 = EDGE_CURVE ( 'NONE', #70030, #36590, #12928, .T. ) ;
#17918 = CARTESIAN_POINT ( 'NONE',  ( -64.13031593051653090, -284.3516778530453166, -338.5210659848444834 ) ) ;
#17919 = CARTESIAN_POINT ( 'NONE',  ( -51.31882272647337828, -291.2306304217091792, -344.2168453672753685 ) ) ;
#17920 = CARTESIAN_POINT ( 'NONE',  ( -54.94434090351493438, -232.1443419142230766, 25.50000000000000000 ) ) ;
#17921 = CARTESIAN_POINT ( 'NONE',  ( -112.2221283039967261, -298.3385691411418748, -280.8545720266008061 ) ) ;
#17922 = CARTESIAN_POINT ( 'NONE',  ( 19.49643042900759937, -278.8735348455500684, -221.4085070258459496 ) ) ;
#17923 = CARTESIAN_POINT ( 'NONE',  ( 27.92062554659392148, -292.2165256299355747, -229.7021124312570635 ) ) ;
#17924 = CARTESIAN_POINT ( 'NONE',  ( -88.66764493470971331, -295.7175498362159374, -217.2606677287537025 ) ) ;
#17925 = CARTESIAN_POINT ( 'NONE',  ( 36.19605775320617624, -280.2497566681219610, -271.3369076827034974 ) ) ;
#17926 = CARTESIAN_POINT ( 'NONE',  ( -54.52057962059964069, -271.9095451280041402, -197.9304594582519599 ) ) ;
#17927 = CARTESIAN_POINT ( 'NONE',  ( -15.42993453999099351, -296.0778288366647075, -340.5653331691756307 ) ) ;
#17928 = CARTESIAN_POINT ( 'NONE',  ( 82.61707336526248469, -302.0539871969763226, -195.3101965168185075 ) ) ;
#17929 = CARTESIAN_POINT ( 'NONE',  ( -30.54182987992833631, -296.6157088357578573, -194.0561673880331455 ) ) ;
#17930 = CARTESIAN_POINT ( 'NONE',  ( 16.82328374188123377, -292.5341632022899603, -323.7287901156560110 ) ) ;
#17931 = CARTESIAN_POINT ( 'NONE',  ( -64.30426354947856282, -293.1185809685653680, -201.8756179379270463 ) ) ;
#17932 = CARTESIAN_POINT ( 'NONE',  ( 125.0516381006427338, 8.053287430127817004, -22.50000000000000000 ) ) ;
#17933 = CARTESIAN_POINT ( 'NONE',  ( 2.319469534305223846, -293.4009671579829046, -208.8227126230175656 ) ) ;
#17934 = CARTESIAN_POINT ( 'NONE',  ( 192.9182251362765328, 250.0000000000000568, 16.22085278731030300 ) ) ;
#17936 = CARTESIAN_POINT ( 'NONE',  ( -23.51883577991246099, -294.8706522354275421, -342.0920666986595506 ) ) ;
#17935 = CARTESIAN_POINT ( 'NONE',  ( -49.84594460838042806, -281.2308681745444119, -344.7243461393659913 ) ) ;
#17937 = CARTESIAN_POINT ( 'NONE',  ( -35.89919520043400070, -283.0345628644328713, -347.3607219302351155 ) ) ;
#17938 = CARTESIAN_POINT ( 'NONE',  ( 16.18541838600518901, -282.7241604108434103, -216.9570936029969914 ) ) ;
#17939 = CARTESIAN_POINT ( 'NONE',  ( -112.9766573518263471, -284.4014519225808044, -255.7626271358629992 ) ) ;
#17940 = CARTESIAN_POINT ( 'NONE',  ( -111.2333342016190585, -288.3986596520966827, -282.2763623087900555 ) ) ;
#17941 = CARTESIAN_POINT ( 'NONE',  ( -187.9122233887894140, -89.54582641780471874, 22.50000000000000000 ) ) ;
#17942 = CARTESIAN_POINT ( 'NONE',  ( 38.83566919842929366, -280.0985560234222476, -275.6324650527377003 ) ) ;
#17943 = CARTESIAN_POINT ( 'NONE',  ( 37.80264758640984724, -286.6649037824816446, -285.6849398751988929 ) ) ;
#17944 = DIRECTION ( 'NONE',  ( 0.9951408606192332362, 1.205805641958552022E-17, 0.09846150276129254919 ) ) ;
#17945 = CARTESIAN_POINT ( 'NONE',  ( 2.013500102684104398, -296.1163451210549056, -332.8524822916819517 ) ) ;
#17946 = CARTESIAN_POINT ( 'NONE',  ( 5.555600154180043049, -277.9087550779553908, -333.5942415821975260 ) ) ;
#17947 = CARTESIAN_POINT ( 'NONE',  ( -19.52528915047310676, -279.9542605156218542, -199.4945267803107640 ) ) ;
#17948 = CARTESIAN_POINT ( 'NONE',  ( 37.08203665545636341, -293.4709804389500505, -250.5591165819264745 ) ) ;
#17949 = CARTESIAN_POINT ( 'NONE',  ( -102.7808759551754036, -283.1336685982954577, -232.4810949917221023 ) ) ;
#17950 = CARTESIAN_POINT ( 'NONE',  ( -96.33944084527684026, -279.9167293191851513, -316.6673512941497393 ) ) ;
#17951 = CARTESIAN_POINT ( 'NONE',  ( 4.648329915294786119, -291.6929981418353464, -210.2968972892569184 ) ) ;
#17952 = CARTESIAN_POINT ( 'NONE',  ( -102.6243353615422222, -271.0489455335326738, -232.9980859303907437 ) ) ;
#17953 = ORIENTED_EDGE ( 'NONE', *, *, #5504, .F. ) ;
#17954 = CYLINDRICAL_SURFACE ( 'NONE', #37823, 2.999999999999993783 ) ;
#17955 = CARTESIAN_POINT ( 'NONE',  ( 35.48527500345447550, -293.1369055841996669, -276.2109158189680329 ) ) ;
#17956 = CYLINDRICAL_SURFACE ( 'NONE', #36783, 4.999999999999978684 ) ;
#17957 = CARTESIAN_POINT ( 'NONE',  ( 30.91033621190086578, -284.8380690714489560, -254.8156830097664738 ) ) ;
#17958 = CARTESIAN_POINT ( 'NONE',  ( -114.0191301341673835, -271.8211713909706191, -264.6280860948100440 ) ) ;
#17959 = CARTESIAN_POINT ( 'NONE',  ( 7.242866786761873676, -287.9604952569976604, -208.1226151188525648 ) ) ;
#17960 = CARTESIAN_POINT ( 'NONE',  ( -58.69115764644078581, -289.1692586464731107, -340.2222362731490648 ) ) ;
#17961 = CARTESIAN_POINT ( 'NONE',  ( -74.34482963965119495, -279.0739464559936209, -334.0908297273024914 ) ) ;
#17962 = CARTESIAN_POINT ( 'NONE',  ( -99.97003332532584352, -274.6852543939538691, -231.3209810034608438 ) ) ;
#17963 = CARTESIAN_POINT ( 'NONE',  ( 2.934630619526648498, -279.4006366701439674, -208.9409556386853524 ) ) ;
#17964 = ORIENTED_EDGE ( 'NONE', *, *, #18823, .F. ) ;
#17965 = CARTESIAN_POINT ( 'NONE',  ( -97.32720108050966701, -296.8656143773355325, -222.1171135140552053 ) ) ;
#17966 = CARTESIAN_POINT ( 'NONE',  ( -111.2156214725146839, -292.3537753134795594, -279.5239746591864218 ) ) ;
#17967 = CARTESIAN_POINT ( 'NONE',  ( 25.81826575643291477, -294.5835893717372187, -227.6390108249181594 ) ) ;
#17968 = DIRECTION ( 'NONE',  ( 0.000000000000000000, -0.9681751575201845705, -0.2502735790305594121 ) ) ;
#17969 = EDGE_CURVE ( 'NONE', #73033, #20083, #3366, .T. ) ;
#17970 = CARTESIAN_POINT ( 'NONE',  ( -96.63644385673210024, -290.6064540176594164, -313.1165390954720351 ) ) ;
#17971 = CARTESIAN_POINT ( 'NONE',  ( 156.8041522122653646, 275.5797763526087465, 16.89672165344857646 ) ) ;
#17972 = CARTESIAN_POINT ( 'NONE',  ( 34.29264416751010458, -291.3738325663738920, -245.5277576387058218 ) ) ;
#17973 = CIRCLE ( 'NONE', #70910, 2.842139515347646750 ) ;
#17974 = CARTESIAN_POINT ( 'NONE',  ( -65.53821522606727967, -298.0268086569568595, -198.6752323913819396 ) ) ;
#17975 = CARTESIAN_POINT ( 'NONE',  ( -109.6427289972625658, -272.2029407733185735, -259.5013167817942303 ) ) ;
#17976 = CARTESIAN_POINT ( 'NONE',  ( -18.20453976106250948, -63.49190233628851132, 21.50000000000000000 ) ) ;
#17977 = LINE ( 'NONE', #24607, #76400 ) ;
#17978 = CARTESIAN_POINT ( 'NONE',  ( -94.92228125629038971, -291.3892706161867636, -320.4329107491910804 ) ) ;
#17979 = CARTESIAN_POINT ( 'NONE',  ( -115.3288506153726871, -298.8376638359844719, -288.1938231032136741 ) ) ;
#17980 = CARTESIAN_POINT ( 'NONE',  ( -95.56410301845868105, -287.2010402643243197, -223.3282454972648168 ) ) ;
#17981 = CARTESIAN_POINT ( 'NONE',  ( -31.16358464767422731, -272.1301938694913360, -195.7702764445280934 ) ) ;
#17982 = CARTESIAN_POINT ( 'NONE',  ( 10.39005413820319923, -276.6366541941227410, -213.1710137120338970 ) ) ;
#17983 = CARTESIAN_POINT ( 'NONE',  ( -0.5235883853854483849, -290.6252841494993504, -205.6490530696761141 ) ) ;
#17984 = CARTESIAN_POINT ( 'NONE',  ( -56.58702471676015477, -279.1579247533197758, -343.6950406279113963 ) ) ;
#17985 = VERTEX_POINT ( 'NONE', #30393 ) ;
#17986 = CARTESIAN_POINT ( 'NONE',  ( 21.08638295824463782, -281.5170183977454030, -314.3141549924685592 ) ) ;
#17987 = CARTESIAN_POINT ( 'NONE',  ( -67.57404601996459803, -278.5192752884484548, -340.8415959338715879 ) ) ;
#17988 = CARTESIAN_POINT ( 'NONE',  ( 37.47438529173152233, -280.5546241949439263, -286.8704121074773639 ) ) ;
#17989 = CARTESIAN_POINT ( 'NONE',  ( -57.01831460352683223, -168.7166579112505076, -361.2910810254234093 ) ) ;
#17990 = CARTESIAN_POINT ( 'NONE',  ( 39.39533236147819650, -276.4675469492279944, -268.3000364723632174 ) ) ;
#17991 = APPLICATION_PROTOCOL_DEFINITION ( 'draft international standard', 'automotive_design', 1998, #84968 ) ;
#17992 = CARTESIAN_POINT ( 'NONE',  ( -89.70131972699893197, -274.8501301295296457, -214.7805831402981482 ) ) ;
#17993 = ADVANCED_FACE ( 'NONE', ( #31332 ), #26004, .F. ) ;
#17994 = CARTESIAN_POINT ( 'NONE',  ( 10.64812456238590066, -296.9090924074130271, -330.4860931364851808 ) ) ;
#17995 = VERTEX_POINT ( 'NONE', #16188 ) ;
#17996 = EDGE_LOOP ( 'NONE', ( #14365, #88855, #13927, #21694 ) ) ;
#17997 = CARTESIAN_POINT ( 'NONE',  ( 222.8344101925596306, 0.000000000000000000, 21.50000000000000000 ) ) ;
#17998 = CARTESIAN_POINT ( 'NONE',  ( -76.02020901471033199, -290.6618753314619994, -332.6363058482935458 ) ) ;
#17999 = CARTESIAN_POINT ( 'NONE',  ( 38.34021232037498095, -289.3984532023920337, -277.1598046428026692 ) ) ;
#18000 = CARTESIAN_POINT ( 'NONE',  ( -107.0518137728636816, -289.6073988583702885, -292.5375279606629420 ) ) ;
#18001 = CARTESIAN_POINT ( 'NONE',  ( -4.794276594578900763, -285.9770882108968522, -200.6460398081742937 ) ) ;
#18002 = DIRECTION ( 'NONE',  ( 0.000000000000000000, 1.000000000000000000, 0.000000000000000000 ) ) ;
#18003 = CARTESIAN_POINT ( 'NONE',  ( 36.50304705240625935, -279.9648481492842507, -271.3445336252290190 ) ) ;
#18004 = CARTESIAN_POINT ( 'NONE',  ( 22.97897273797579487, -290.0073499000262700, -313.6309909518141126 ) ) ;
#18005 = CARTESIAN_POINT ( 'NONE',  ( -61.78276150045344650, -281.8553734777087243, -339.9371088017694547 ) ) ;
#18006 = CARTESIAN_POINT ( 'NONE',  ( -69.97424247316737933, -280.9282175235711634, -204.4961280445561442 ) ) ;
#18007 = CARTESIAN_POINT ( 'NONE',  ( 38.85852485267836443, -288.6153405054805035, -280.0814623336628983 ) ) ;
#18008 = CARTESIAN_POINT ( 'NONE',  ( -104.3253024600627441, -278.6510317413237772, -299.6629466611464636 ) ) ;
#18009 = CARTESIAN_POINT ( 'NONE',  ( -110.8468058300933308, -289.6189627239074298, -248.7970702489311918 ) ) ;
#18010 = CARTESIAN_POINT ( 'NONE',  ( -105.6359288366484606, -284.8988409717413219, -305.6916251268866063 ) ) ;
#18011 = CARTESIAN_POINT ( 'NONE',  ( -60.49737871820320834, -286.2521588366652168, -196.9343270369304264 ) ) ;
#18012 = CARTESIAN_POINT ( 'NONE',  ( -88.89278703546426641, -283.9676730958867665, -322.1184815215181629 ) ) ;
#18013 = ORIENTED_EDGE ( 'NONE', *, *, #54005, .T. ) ;
#18014 = DIRECTION ( 'NONE',  ( -0.6421047760857900855, 0.000000000000000000, -0.7666168903225504261 ) ) ;
#18015 = CARTESIAN_POINT ( 'NONE',  ( -6.413199518535557253, -294.3144447141544333, -201.1825231115184920 ) ) ;
#18016 = CARTESIAN_POINT ( 'NONE',  ( 39.00876406373024707, -292.3082015038104373, -276.0194636441065086 ) ) ;
#18017 = CARTESIAN_POINT ( 'NONE',  ( 19.18809629456653809, -273.9531950305727150, -223.8015801276337129 ) ) ;
#18018 = EDGE_CURVE ( 'NONE', #79410, #34882, #30550, .T. ) ;
#18019 = CARTESIAN_POINT ( 'NONE',  ( -94.58125694300041175, -295.2029220962525642, -321.7319407562005154 ) ) ;
#18020 = CARTESIAN_POINT ( 'NONE',  ( -3.298921860933128336, -290.9901752331776947, -205.0021323581624983 ) ) ;
#18021 = CARTESIAN_POINT ( 'NONE',  ( -61.36295055479155280, -293.6081528662633104, -340.4222530457843163 ) ) ;
#18022 = CARTESIAN_POINT ( 'NONE',  ( -72.83233706808053398, -292.7763400831755121, -206.0580258984577142 ) ) ;
#18023 = CARTESIAN_POINT ( 'NONE',  ( 209.7064572754727010, 36.40703279031868789, 14.69807322781338854 ) ) ;
#18024 = CARTESIAN_POINT ( 'NONE',  ( -2.873279564846140222, -290.5064174230686831, -203.5488127789022599 ) ) ;
#18025 = CARTESIAN_POINT ( 'NONE',  ( 37.40978467044119071, -295.6383167608520353, -277.0590636709445675 ) ) ;
#18026 = CARTESIAN_POINT ( 'NONE',  ( 14.25763484092335887, -289.2461596953247636, -322.3314660537604937 ) ) ;
#18027 = CARTESIAN_POINT ( 'NONE',  ( -41.27287486526417837, -279.0812758069678239, -345.6266372181603401 ) ) ;
#18028 = CARTESIAN_POINT ( 'NONE',  ( -98.49574850924500424, -276.7293206268953440, -316.5149732037925787 ) ) ;
#18029 = CARTESIAN_POINT ( 'NONE',  ( 30.62114302869646210, -298.0799046342134488, -193.5315563099809992 ) ) ;
#18030 = CARTESIAN_POINT ( 'NONE',  ( -21.45709149045410413, -275.0856687575517299, -342.7025081007390099 ) ) ;
#18031 = CARTESIAN_POINT ( 'NONE',  ( -88.50290385550056271, -277.4083945310232480, -216.2173105567106575 ) ) ;
#18032 = CARTESIAN_POINT ( 'NONE',  ( -74.95918653625092531, -275.9444142133216360, -336.6284940595022022 ) ) ;
#18033 = ADVANCED_FACE ( 'NONE', ( #73941 ), #9056, .F. ) ;
#18034 = CARTESIAN_POINT ( 'NONE',  ( -92.57227568588936606, -294.5495288714236040, -318.8464456849785051 ) ) ;
#18035 = CARTESIAN_POINT ( 'NONE',  ( 152.4536156746142410, 249.5000000000000568, -12.50000000000000000 ) ) ;
#18036 = CARTESIAN_POINT ( 'NONE',  ( -49.99186470170865704, -298.6894284096910610, -198.3015935408572830 ) ) ;
#18037 = CONICAL_SURFACE ( 'NONE', #33170, 24.00000000000001066, 0.7853981633974361776 ) ;
#18038 = CARTESIAN_POINT ( 'NONE',  ( 208.8930925782355530, 0.04008605884692667543, 7.489252814170929362 ) ) ;
#18040 = CARTESIAN_POINT ( 'NONE',  ( 15.44825792080862570, -274.6574826638428135, -219.8675067066500333 ) ) ;
#18039 = CARTESIAN_POINT ( 'NONE',  ( -84.16285887031533264, -287.7119377562086129, -329.4716425059943958 ) ) ;
#18041 = CARTESIAN_POINT ( 'NONE',  ( 38.29018392685653538, -287.3714282203288235, -255.9105777054480484 ) ) ;
#18042 = CARTESIAN_POINT ( 'NONE',  ( -105.1993608477266520, -274.9768893016398579, -238.0289930122082467 ) ) ;
#18043 = CARTESIAN_POINT ( 'NONE',  ( -105.6195421794715941, -294.1480482802759298, -301.1173586129912110 ) ) ;
#18044 = CARTESIAN_POINT ( 'NONE',  ( -99.66352008639135818, -283.1511254564550200, -315.3961251892413884 ) ) ;
#18045 = CARTESIAN_POINT ( 'NONE',  ( 152.4536156746142410, 129.7208004331680797, -12.50000000000000000 ) ) ;
#18046 = CARTESIAN_POINT ( 'NONE',  ( -110.7826118108331741, -276.7481238899337654, -255.0860738245242487 ) ) ;
#18047 = CARTESIAN_POINT ( 'NONE',  ( 0.000000000000000000, 15.00000000000000000, 15.00000000000000000 ) ) ;
#18048 = CARTESIAN_POINT ( 'NONE',  ( -110.6412360897021188, -289.4082884483579505, -265.6951657635079300 ) ) ;
#18049 = DIRECTION ( 'NONE',  ( 0.000000000000000000, 1.000000000000000000, 0.000000000000000000 ) ) ;
#18050 =( LENGTH_UNIT ( ) NAMED_UNIT ( * ) SI_UNIT ( .MILLI., .METRE. ) );
#18051 = CARTESIAN_POINT ( 'NONE',  ( -109.6741961782062020, -288.8069350171326732, -250.5366213644957725 ) ) ;
#18052 = CARTESIAN_POINT ( 'NONE',  ( -29.93929056898641861, -275.6676698235258982, -197.0405063863528028 ) ) ;
#18053 = CARTESIAN_POINT ( 'NONE',  ( 38.59506268172602006, -282.8644978374809966, -261.4008997495978406 ) ) ;
#18055 = CARTESIAN_POINT ( 'NONE',  ( -76.12712328346938762, -283.5858777957122356, -332.2649855398151431 ) ) ;
#18054 = CARTESIAN_POINT ( 'NONE',  ( 73.39505216521877173, -297.4518555997764793, -195.0430490344880639 ) ) ;
#18056 = CARTESIAN_POINT ( 'NONE',  ( -76.89610879619954176, -274.9361968461952301, -208.3061127740946858 ) ) ;
#18057 = CARTESIAN_POINT ( 'NONE',  ( 33.66343321265914312, -276.1228331557512661, -252.7295336312109839 ) ) ;
#18058 = CARTESIAN_POINT ( 'NONE',  ( 10.24384159414530693, -284.3963923786469081, -328.3991689218567558 ) ) ;
#18059 = CARTESIAN_POINT ( 'NONE',  ( -85.50292996027178560, -272.2882151667443509, -215.0239310549584388 ) ) ;
#18060 = ORIENTED_EDGE ( 'NONE', *, *, #23274, .T. ) ;
#18061 = DIRECTION ( 'NONE',  ( 0.000000000000000000, 1.000000000000000000, 0.000000000000000000 ) ) ;
#18062 = CARTESIAN_POINT ( 'NONE',  ( 22.28528703165126856, -294.0396495093075941, -319.1016519084193988 ) ) ;
#18063 = CARTESIAN_POINT ( 'NONE',  ( -100.4074896745002121, -285.9912218275712235, -310.3896868822066040 ) ) ;
#18064 = DIRECTION ( 'NONE',  ( 0.000000000000000000, 0.000000000000000000, 1.000000000000000000 ) ) ;
#18065 = CARTESIAN_POINT ( 'NONE',  ( -111.2586520408596868, -276.4809262143062369, -234.7283546768995564 ) ) ;
#18066 = CARTESIAN_POINT ( 'NONE',  ( -114.0713048191169463, -277.6980648889752388, -274.4509326489190926 ) ) ;
#18067 = CARTESIAN_POINT ( 'NONE',  ( -71.56561616223670796, -287.8965877215275668, -338.4431566515374925 ) ) ;
#18068 = CARTESIAN_POINT ( 'NONE',  ( -64.29106800550495393, -284.9304544015237184, -338.9500334413642122 ) ) ;
#18069 = CARTESIAN_POINT ( 'NONE',  ( -83.62318655960478964, -279.4568709248052869, -328.1851628299783101 ) ) ;
#18070 = CARTESIAN_POINT ( 'NONE',  ( 9.435613885606153772, -288.1064320772111387, -209.9418397267265846 ) ) ;
#18071 = CARTESIAN_POINT ( 'NONE',  ( -13.70199456395707571, -282.3590026441876262, -199.1292238622698676 ) ) ;
#18072 = CARTESIAN_POINT ( 'NONE',  ( 26.14336544449704647, -275.1435071581625493, -226.7642883875858502 ) ) ;
#18073 = CARTESIAN_POINT ( 'NONE',  ( -114.0793033075686793, -278.2983300078909679, -277.3289659113175958 ) ) ;
#18074 = CARTESIAN_POINT ( 'NONE',  ( -111.6511860468581290, -298.5293127653650345, -265.9549293871266400 ) ) ;
#18075 = CARTESIAN_POINT ( 'NONE',  ( 156.2095471516454950, 16.65459343288105742, 7.440913067426849992 ) ) ;
#18076 = CARTESIAN_POINT ( 'NONE',  ( 10.59707575819634329, -277.1948066931274184, -210.1954327657594490 ) ) ;
#18077 = CARTESIAN_POINT ( 'NONE',  ( 18.28230932294182765, -296.8810154162835602, -194.6137105603779673 ) ) ;
#18078 = CARTESIAN_POINT ( 'NONE',  ( -21.64590741762824067, -276.3532587977351795, -341.7688153884450912 ) ) ;
#18079 = CARTESIAN_POINT ( 'NONE',  ( -15.90327380157685866, -275.5283849561884040, -196.7642256439629875 ) ) ;
#18080 = CARTESIAN_POINT ( 'NONE',  ( -30.45906869755862800, -287.9003832277448396, -196.6169872058072201 ) ) ;
#18081 = CARTESIAN_POINT ( 'NONE',  ( -113.4311038434072714, -298.1532039758272958, -263.9481717307529607 ) ) ;
#18082 = CARTESIAN_POINT ( 'NONE',  ( -65.44347433371051181, -296.6165405443485383, -341.6374502665573800 ) ) ;
#18083 = CARTESIAN_POINT ( 'NONE',  ( 18.07920354488868497, -294.8486975101263283, -220.0004401667031289 ) ) ;
#18084 = CARTESIAN_POINT ( 'NONE',  ( -66.76772219179306944, -277.6655957177939058, -201.5420688903798521 ) ) ;
#18085 = CARTESIAN_POINT ( 'NONE',  ( -1.289670350696733969, -282.4544997042830801, -205.2338168861113274 ) ) ;
#18086 = CARTESIAN_POINT ( 'NONE',  ( -91.06857115018763693, -295.3619118662326741, -218.7632322667241453 ) ) ;
#18087 = CARTESIAN_POINT ( 'NONE',  ( -63.46355892975361002, -285.2493971380450262, -341.4804119374946367 ) ) ;
#18088 = CARTESIAN_POINT ( 'NONE',  ( -5.652630567788729188, -285.3992527417561291, -204.2410801963400218 ) ) ;
#18089 = CARTESIAN_POINT ( 'NONE',  ( -105.6297312391304359, -263.1519871882180723, -317.3200005741121004 ) ) ;
#18090 = ORIENTED_EDGE ( 'NONE', *, *, #16334, .T. ) ;
#18091 = CARTESIAN_POINT ( 'NONE',  ( 18.68071328570327694, -286.5540901638994455, -223.5060017140951913 ) ) ;
#18092 = EDGE_LOOP ( 'NONE', ( #54036, #2952, #91460, #50386 ) ) ;
#18093 = CARTESIAN_POINT ( 'NONE',  ( -113.5950452014927379, -285.5291007883886891, -278.5415748413252572 ) ) ;
#18094 = CARTESIAN_POINT ( 'NONE',  ( 35.37545181723947252, -275.9732145410503676, -277.0171903743586199 ) ) ;
#18095 = CARTESIAN_POINT ( 'NONE',  ( 38.58375897387485765, -286.2192895141771487, -260.1958153054453646 ) ) ;
#18096 = CARTESIAN_POINT ( 'NONE',  ( -101.4180963075515507, -290.0297646582602056, -228.1266961355314891 ) ) ;
#18097 = CARTESIAN_POINT ( 'NONE',  ( 35.10164134661182089, -282.1703452812040496, -244.8098595320705613 ) ) ;
#18098 = CARTESIAN_POINT ( 'NONE',  ( 73.43068321062709458, -178.2391364535880882, 0.000000000000000000 ) ) ;
#18099 = CARTESIAN_POINT ( 'NONE',  ( -74.68567290369099965, -281.0845501752829705, -203.8168811883388685 ) ) ;
#18100 = CARTESIAN_POINT ( 'NONE',  ( 22.85612142997651119, -281.2426715117946969, -222.3613495282661745 ) ) ;
#18101 = AXIS2_PLACEMENT_3D ( 'NONE', #500, #67234, #44951 ) ;
#18102 = CARTESIAN_POINT ( 'NONE',  ( -67.74223827176246004, -286.9809262143061233, -333.4151289067050357 ) ) ;
#18103 = CARTESIAN_POINT ( 'NONE',  ( -83.59145992945265391, -219.8537403536915349, -352.6472634170126526 ) ) ;
#18104 = EDGE_LOOP ( 'NONE', ( #62633, #43175, #23249, #18216 ) ) ;
#18105 = CARTESIAN_POINT ( 'NONE',  ( 32.99342612457994761, -277.8861982004544871, -296.0656774936185229 ) ) ;
#18106 = CARTESIAN_POINT ( 'NONE',  ( 4.790628490442398579, -57.97448044145017576, -354.2496948606743103 ) ) ;
#18107 = AXIS2_PLACEMENT_3D ( 'NONE', #47010, #18621, #46551 ) ;
#18108 = CARTESIAN_POINT ( 'NONE',  ( 26.96347060040966781, -280.0826325642604502, -308.3669161624852109 ) ) ;
#18109 = CARTESIAN_POINT ( 'NONE',  ( -16.75952356001461752, -296.5501350731234993, -343.5617022503755038 ) ) ;
#18110 = CARTESIAN_POINT ( 'NONE',  ( -102.8631988861991289, -295.4605631668603110, -302.8919788410278215 ) ) ;
#18111 = CARTESIAN_POINT ( 'NONE',  ( -101.6290880532886405, -290.6169941463634245, -227.9966399342466161 ) ) ;
#18112 = DIRECTION ( 'NONE',  ( 0.000000000000000000, 0.000000000000000000, 1.000000000000000000 ) ) ;
#18114 = CARTESIAN_POINT ( 'NONE',  ( 33.84824440399329148, -286.2084714786589643, -290.0038920776575537 ) ) ;
#18113 = CARTESIAN_POINT ( 'NONE',  ( -112.8047378861226093, -295.2791273407638641, -258.2810093332199699 ) ) ;
#18115 = CARTESIAN_POINT ( 'NONE',  ( 35.92933724591973288, -295.2568409881761795, -258.3561569091314709 ) ) ;
#18116 = CARTESIAN_POINT ( 'NONE',  ( -4.388352754425544511, -287.8110998014808501, -204.6700198311277745 ) ) ;
#18117 = ORIENTED_EDGE ( 'NONE', *, *, #84467, .F. ) ;
#18118 = CARTESIAN_POINT ( 'NONE',  ( 24.70319955045539473, -295.0954095058709754, -315.5855944460318483 ) ) ;
#18119 = CARTESIAN_POINT ( 'NONE',  ( -110.0563141808517003, -285.1448226521748097, -262.7498669716907784 ) ) ;
#18120 = CARTESIAN_POINT ( 'NONE',  ( -111.9227573999169607, -295.1265798582989532, -287.9014542500962648 ) ) ;
#18121 = CARTESIAN_POINT ( 'NONE',  ( -102.1595363065640498, -290.8118206242222072, -311.7240932340248492 ) ) ;
#18122 = CARTESIAN_POINT ( 'NONE',  ( -112.5811137997226865, -291.2464985321876156, -254.2192117478826390 ) ) ;
#18123 = CARTESIAN_POINT ( 'NONE',  ( -107.7252383329497576, -290.4606925366467181, -289.9163623409639854 ) ) ;
#18124 = ORIENTED_EDGE ( 'NONE', *, *, #47455, .F. ) ;
#18125 = FACE_OUTER_BOUND ( 'NONE', #93299, .T. ) ;
#18126 = CARTESIAN_POINT ( 'NONE',  ( -86.67621203822126574, -299.2356916232678827, -212.7905346530961879 ) ) ;
#18127 = CARTESIAN_POINT ( 'NONE',  ( -83.32939574910948011, -272.2329275806613964, -209.0318582419886297 ) ) ;
#18128 = CARTESIAN_POINT ( 'NONE',  ( -16.07558768771819047, -281.8290384852472243, -340.4407934189530351 ) ) ;
#18129 = CARTESIAN_POINT ( 'NONE',  ( 25.28046480523453710, -274.4669971186978614, -225.6396809806910255 ) ) ;
#18130 = CARTESIAN_POINT ( 'NONE',  ( -108.2753891595561839, -294.7704246917772934, -290.3390937019854050 ) ) ;
#18131 = CARTESIAN_POINT ( 'NONE',  ( -69.76995504129746450, -279.3441004804227532, -337.1529813944812872 ) ) ;
#18132 = CARTESIAN_POINT ( 'NONE',  ( -32.58867434441228284, -272.2522469987749787, -196.2654923021844979 ) ) ;
#18133 = CARTESIAN_POINT ( 'NONE',  ( -40.55060778842110381, -299.2160173004481294, -197.0216068422801925 ) ) ;
#18134 = CARTESIAN_POINT ( 'NONE',  ( -69.40509320019954487, -298.6996137152854089, -204.4356684245572922 ) ) ;
#18135 = DIRECTION ( 'NONE',  ( 0.000000000000000000, 1.000000000000000000, 0.000000000000000000 ) ) ;
#18136 = CARTESIAN_POINT ( 'NONE',  ( -84.73494010419553035, -299.0113074292253259, -210.6926906699645770 ) ) ;
#18137 = CARTESIAN_POINT ( 'NONE',  ( -105.3477705462717040, -270.9974771543297152, -237.9022026277494604 ) ) ;
#18138 = CARTESIAN_POINT ( 'NONE',  ( 12.43034001889411222, -294.9884195360733656, -323.9714860499759084 ) ) ;
#18139 = CARTESIAN_POINT ( 'NONE',  ( 2.575236969764949091, -291.1732212437169665, -208.4783142036073684 ) ) ;
#18140 = DIRECTION ( 'NONE',  ( -0.000000000000000000, -0.000000000000000000, -1.000000000000000000 ) ) ;
#18141 = CARTESIAN_POINT ( 'NONE',  ( -7.720073655555841796, -274.9223180753100451, -199.2969198332054361 ) ) ;
#18142 = CARTESIAN_POINT ( 'NONE',  ( -37.82691618514939336, -298.3791909823559081, -197.3415859910845711 ) ) ;
#18143 = CARTESIAN_POINT ( 'NONE',  ( 16.66543480844003255, -284.2688982524047105, -322.9869758288136836 ) ) ;
#18144 = CARTESIAN_POINT ( 'NONE',  ( -30.27720841372053684, -281.6493745725233566, -346.5411102987293930 ) ) ;
#18145 = CARTESIAN_POINT ( 'NONE',  ( -56.90611539612606862, -276.6464998373929802, -344.7837432606136758 ) ) ;
#18146 = CARTESIAN_POINT ( 'NONE',  ( 204.6539576904058606, 293.9636489450775230, 7.999911143031724237 ) ) ;
#18147 = CARTESIAN_POINT ( 'NONE',  ( -80.73010197126023968, -282.8547259652038406, -329.3312706299911383 ) ) ;
#18148 = CARTESIAN_POINT ( 'NONE',  ( -41.49395986215245102, -281.1040366486934658, -345.4640943208969475 ) ) ;
#18149 = ADVANCED_FACE ( 'NONE', ( #74889 ), #24686, .F. ) ;
#18150 = CARTESIAN_POINT ( 'NONE',  ( 14.13060180820468936, -274.8870813091570540, -323.0246247685816456 ) ) ;
#18151 = CARTESIAN_POINT ( 'NONE',  ( -64.59782538862290835, -281.6966279207716184, -200.4342570663369827 ) ) ;
#18152 = CARTESIAN_POINT ( 'NONE',  ( 210.2502813974796538, 1.019348808636640458, 7.290232558141290120 ) ) ;
#18153 = DIRECTION ( 'NONE',  ( 0.9452808130703180822, -1.131934301928085161E-15, -0.3262578496237575343 ) ) ;
#18154 = CARTESIAN_POINT ( 'NONE',  ( -80.77747054860677167, -271.8738210070736159, -207.6890882135760421 ) ) ;
#18155 = CARTESIAN_POINT ( 'NONE',  ( -111.2580287891604485, -280.3764921234789540, -284.0847209193519234 ) ) ;
#18156 = CARTESIAN_POINT ( 'NONE',  ( 209.7513585654923816, 282.2246705312486483, 13.99999999999999112 ) ) ;
#18157 = CARTESIAN_POINT ( 'NONE',  ( -90.89986402906950502, -287.2193120737205732, -217.0616125765146478 ) ) ;
#18158 = VERTEX_POINT ( 'NONE', #39325 ) ;
#18159 = CARTESIAN_POINT ( 'NONE',  ( 156.4851178187871312, 15.00000000000000178, -7.000000000000000888 ) ) ;
#18160 = CARTESIAN_POINT ( 'NONE',  ( 36.84248808864709446, -285.4059526134255407, -258.9873166894478231 ) ) ;
#18161 = DIRECTION ( 'NONE',  ( -1.110223024625156146E-15, 0.000000000000000000, 1.000000000000000000 ) ) ;
#18162 = CARTESIAN_POINT ( 'NONE',  ( -110.1279612694756338, -295.4760791475494557, -260.5284142102742067 ) ) ;
#18163 = CARTESIAN_POINT ( 'NONE',  ( -105.1860589060041207, -288.2913466964842542, -300.6213360324474024 ) ) ;
#18164 = CARTESIAN_POINT ( 'NONE',  ( 64.33209501061345748, 48.33985520751024723, -319.1928417150128325 ) ) ;
#18165 = CARTESIAN_POINT ( 'NONE',  ( -97.69499511117089696, -295.1596666381653336, -225.8143914365068383 ) ) ;
#18166 = CARTESIAN_POINT ( 'NONE',  ( -30.92270915973745815, -284.6117327519158948, -194.3117388756587616 ) ) ;
#18167 = CARTESIAN_POINT ( 'NONE',  ( 22.47216124325061415, -283.7506862935746881, -313.6117163196296360 ) ) ;
#18168 = CARTESIAN_POINT ( 'NONE',  ( -64.90578011014414983, -281.6471356910333839, -341.1861210966881686 ) ) ;
#18169 = CARTESIAN_POINT ( 'NONE',  ( -61.25501244800953060, -289.3715228502236414, -339.3332391177663112 ) ) ;
#18170 = CARTESIAN_POINT ( 'NONE',  ( -43.82091183182579641, -281.3940838636777357, -197.0070357235220513 ) ) ;
#18171 = CARTESIAN_POINT ( 'NONE',  ( -37.01785133431243935, -280.8591444631121021, -197.2003576699578673 ) ) ;
#18172 = CARTESIAN_POINT ( 'NONE',  ( 34.81779940107080762, -289.8110128755184292, -292.1180423218158353 ) ) ;
#18173 = CIRCLE ( 'NONE', #62043, 1.999999999999988454 ) ;
#18174 = CARTESIAN_POINT ( 'NONE',  ( -113.7750372036288411, -296.8354465289459654, -261.0366883487457130 ) ) ;
#18175 = ORIENTED_EDGE ( 'NONE', *, *, #82436, .T. ) ;
#18176 = CARTESIAN_POINT ( 'NONE',  ( -24.15960795104886927, -274.2158917917183771, -194.4437033385387963 ) ) ;
#18178 = CARTESIAN_POINT ( 'NONE',  ( -107.5717539381432175, -292.2026357477438978, -295.6511623316070541 ) ) ;
#18177 = AXIS2_PLACEMENT_3D ( 'NONE', #78572, #78113, #64865 ) ;
#18179 = CARTESIAN_POINT ( 'NONE',  ( 208.4306832106270804, -124.2391364535881024, 0.000000000000000000 ) ) ;
#18180 = CARTESIAN_POINT ( 'NONE',  ( -4.829096099716510437, -276.9805209788416391, -202.7746430608542312 ) ) ;
#18181 = EDGE_LOOP ( 'NONE', ( #55024, #55045, #4241, #85295 ) ) ;
#18182 = CARTESIAN_POINT ( 'NONE',  ( 17.54664569466083179, -274.2695623513662895, -321.7157469823216616 ) ) ;
#18183 = CARTESIAN_POINT ( 'NONE',  ( 195.5881128153457098, -27.00396092263537540, 22.50000000000000000 ) ) ;
#18184 = CARTESIAN_POINT ( 'NONE',  ( -3.601533979201898106, -293.0142652762226589, -338.6986365584622263 ) ) ;
#18185 = CARTESIAN_POINT ( 'NONE',  ( -27.26793590769204556, -273.5320073009398811, -197.9056457494495191 ) ) ;
#18186 = CARTESIAN_POINT ( 'NONE',  ( -109.0203320172620494, -291.8486196019856038, -287.4748985430444463 ) ) ;
#18187 = CARTESIAN_POINT ( 'NONE',  ( 20.99330678552420437, -283.9455359496082565, -315.9132966880353592 ) ) ;
#18188 = CARTESIAN_POINT ( 'NONE',  ( -56.06213042052504392, -293.2410307243430907, -196.2245256439732373 ) ) ;
#18189 = CARTESIAN_POINT ( 'NONE',  ( -4.829022191148051313, -293.7866085262849083, -201.1063416257239282 ) ) ;
#18190 = CARTESIAN_POINT ( 'NONE',  ( -15.59485231117861481, -294.5962133917923893, -340.0998296046340101 ) ) ;
#18191 = CARTESIAN_POINT ( 'NONE',  ( 23.60131616392930809, -290.1470718771006432, -314.0755253990889173 ) ) ;
#18192 = CARTESIAN_POINT ( 'NONE',  ( -1.632255045848221009, -282.7587562147315907, -338.5801441881794176 ) ) ;
#18193 = CARTESIAN_POINT ( 'NONE',  ( -100.3354151751951377, -295.1916321699050059, -228.6110057608879629 ) ) ;
#18194 = CARTESIAN_POINT ( 'NONE',  ( -90.43967588808307312, -283.6121212476750770, -326.1980611174371916 ) ) ;
#18195 = CARTESIAN_POINT ( 'NONE',  ( 34.43478431926597239, -277.2648973475054959, -249.6831612301122902 ) ) ;
#18196 = CARTESIAN_POINT ( 'NONE',  ( -21.39648532958013050, -294.7662352645559736, -200.3538533559491555 ) ) ;
#18197 = CARTESIAN_POINT ( 'NONE',  ( -107.5213509424310985, -276.3232438051216491, -298.9114610597084152 ) ) ;
#18198 = CARTESIAN_POINT ( 'NONE',  ( 188.7149167944524493, 8.542400036368780647, -9.000000000000001776 ) ) ;
#18199 = CARTESIAN_POINT ( 'NONE',  ( -21.38087224186254076, -282.3496806299198738, -341.7100209162651936 ) ) ;
#18200 = CARTESIAN_POINT ( 'NONE',  ( -79.70404211110033543, -280.6987563318910475, -206.4739675803249099 ) ) ;
#18201 = CARTESIAN_POINT ( 'NONE',  ( 37.79568156391006539, -286.4128727583988621, -254.5750176337077164 ) ) ;
#18202 = CARTESIAN_POINT ( 'NONE',  ( 7.269428477275335254, -294.4298706296019645, -211.3033393625548797 ) ) ;
#18203 = CARTESIAN_POINT ( 'NONE',  ( 4.407634550606300827, -276.2048717232679564, -206.5534572840067824 ) ) ;
#18204 = EDGE_CURVE ( 'NONE', #60166, #54193, #90447, .T. ) ;
#18205 = CARTESIAN_POINT ( 'NONE',  ( 36.10765709695770909, -276.5949543200039216, -248.7637435899196419 ) ) ;
#18207 = EDGE_CURVE ( 'NONE', #5766, #41385, #13304, .T. ) ;
#18206 = CARTESIAN_POINT ( 'NONE',  ( -41.85870550146714208, -276.9439378589466969, -343.2338315069463874 ) ) ;
#18208 = CARTESIAN_POINT ( 'NONE',  ( -99.22052059591496231, -275.1005702501601036, -228.5213059457727525 ) ) ;
#18209 = CARTESIAN_POINT ( 'NONE',  ( -60.52295502680039618, -283.7506191254590817, -199.2087614083980043 ) ) ;
#18210 = CARTESIAN_POINT ( 'NONE',  ( -50.55855099160432786, -291.5544947063978611, -194.5253800703103764 ) ) ;
#18211 = CARTESIAN_POINT ( 'NONE',  ( -88.93470132794379879, -291.3630481201342377, -326.4378746738435666 ) ) ;
#18212 = CARTESIAN_POINT ( 'NONE',  ( -19.98570428150715372, -291.2006857172567607, -199.0836611186962841 ) ) ;
#18213 = ORIENTED_EDGE ( 'NONE', *, *, #28676, .T. ) ;
#18214 = CARTESIAN_POINT ( 'NONE',  ( -25.09783649236970504, -290.7800888239664800, -194.9376859815413070 ) ) ;
#18215 = CARTESIAN_POINT ( 'NONE',  ( 28.75946473516069801, -292.7984424068595217, -239.2139817779631414 ) ) ;
#18216 = ORIENTED_EDGE ( 'NONE', *, *, #5917, .T. ) ;
#18217 = CARTESIAN_POINT ( 'NONE',  ( -23.35476190864703838, -289.9571510257961222, -345.8196457278615981 ) ) ;
#18218 = CARTESIAN_POINT ( 'NONE',  ( -91.37775038224786783, -279.9085582765397362, -221.1270043901050428 ) ) ;
#18219 = CARTESIAN_POINT ( 'NONE',  ( -114.0573774903131579, -295.4462826281028356, -272.4476079983765544 ) ) ;
#18220 = CARTESIAN_POINT ( 'NONE',  ( -85.45559725608460155, -286.0580012751763661, -210.3747387834109190 ) ) ;
#18221 = CARTESIAN_POINT ( 'NONE',  ( -10.00544028538734231, -286.7326382377291338, -198.3427249654797890 ) ) ;
#18222 = CARTESIAN_POINT ( 'NONE',  ( -86.94008692393909143, -284.0984581363721304, -324.0221513108425029 ) ) ;
#18223 = CARTESIAN_POINT ( 'NONE',  ( 197.2159948018767750, 285.3705696945321506, -111.7930995898936430 ) ) ;
#18224 = CARTESIAN_POINT ( 'NONE',  ( -96.30717022866939203, -238.7289040402379499, -340.4382983491259438 ) ) ;
#18225 = CARTESIAN_POINT ( 'NONE',  ( -111.6101193260526685, -270.5214411657722167, -283.6473540868328769 ) ) ;
#18226 = CARTESIAN_POINT ( 'NONE',  ( -6.217195794883286553, -275.8295935994290744, -336.5856925556955161 ) ) ;
#18227 = CARTESIAN_POINT ( 'NONE',  ( 20.25682744417047587, -275.1097319319255234, -315.7314752650584637 ) ) ;
#18228 = CARTESIAN_POINT ( 'NONE',  ( -109.7908048430232242, -296.3869687276562672, -244.4641272472954654 ) ) ;
#18229 = CARTESIAN_POINT ( 'NONE',  ( 200.0284319754563001, 285.7751889741193736, -96.47188040663559150 ) ) ;
#18230 = CARTESIAN_POINT ( 'NONE',  ( 17.74622032706428598, -273.5047082110119732, -217.1943800814364351 ) ) ;
#18231 = CARTESIAN_POINT ( 'NONE',  ( -40.84503458390711472, -275.7677631804482985, -196.3803512175339847 ) ) ;
#18232 = EDGE_LOOP ( 'NONE', ( #7254, #18926, #87600, #85867, #69916, #62240 ) ) ;
#18233 = CARTESIAN_POINT ( 'NONE',  ( 75.94312787335357484, -300.3792304208613473, -193.5787399965042823 ) ) ;
#18234 = CARTESIAN_POINT ( 'NONE',  ( -94.99525922198839112, -290.4125029528289019, -315.2595586687715468 ) ) ;
#18235 = CARTESIAN_POINT ( 'NONE',  ( -111.4335959565501213, -297.0993993742635553, -290.7216138842616715 ) ) ;
#18236 = CARTESIAN_POINT ( 'NONE',  ( -54.58747309104741419, -298.3286030556758419, -195.3803856710929097 ) ) ;
#18237 = CARTESIAN_POINT ( 'NONE',  ( 25.79372730310853612, -294.2215857037617184, -307.0069609605939718 ) ) ;
#18238 = EDGE_LOOP ( 'NONE', ( #8585, #89004, #88207, #7750, #55105, #35384 ) ) ;
#18239 = CARTESIAN_POINT ( 'NONE',  ( 0.3503353407831176769, -278.4747251098199285, -335.9080661585416578 ) ) ;
#18240 = CARTESIAN_POINT ( 'NONE',  ( 24.54597781270600265, -280.4518560126807643, -224.6507009806088604 ) ) ;
#18241 = CARTESIAN_POINT ( 'NONE',  ( -95.45242961043835805, -278.8683382162713542, -314.9318658767951433 ) ) ;
#18242 = CARTESIAN_POINT ( 'NONE',  ( -12.18029923166183082, -278.4894790951256027, -342.1162313434322186 ) ) ;
#18243 = CARTESIAN_POINT ( 'NONE',  ( -91.17211685321684911, -273.7530349604699609, -220.9434598797185174 ) ) ;
#18244 = CARTESIAN_POINT ( 'NONE',  ( -35.78185683332136335, -296.6467796405653985, -196.7722720066452382 ) ) ;
#18245 = CARTESIAN_POINT ( 'NONE',  ( 175.2296996224750103, 250.0000000000000568, 0.000000000000000000 ) ) ;
#18246 = CARTESIAN_POINT ( 'NONE',  ( -95.61303273711043005, -279.3367341394397272, -226.3693346183222275 ) ) ;
#18247 = CARTESIAN_POINT ( 'NONE',  ( 4.766106513950871815, -275.4077043515254672, -206.0244268040095506 ) ) ;
#18248 = CARTESIAN_POINT ( 'NONE',  ( 14.25866750302365737, -287.0301880852786667, -326.9191781763510676 ) ) ;
#18249 = CARTESIAN_POINT ( 'NONE',  ( 8.273239772838325123, -276.6764850652170367, -210.8272796759979713 ) ) ;
#18250 = CARTESIAN_POINT ( 'NONE',  ( -73.63393023854700914, -288.7441994783907262, -333.9009569047717605 ) ) ;
#18251 = CARTESIAN_POINT ( 'NONE',  ( -95.73371541225596104, -284.5774979902026871, -220.2444228675807381 ) ) ;
#18252 = CARTESIAN_POINT ( 'NONE',  ( -3.173229676874998351, -280.8342943871166426, -336.0296350206020293 ) ) ;
#18254 = CARTESIAN_POINT ( 'NONE',  ( -71.82396726941632892, -283.6724948674674920, -204.3892493326195563 ) ) ;
#18253 = CARTESIAN_POINT ( 'NONE',  ( 36.10908704477111542, -280.0678305426265524, -265.8492691944703097 ) ) ;
#18255 = CARTESIAN_POINT ( 'NONE',  ( -46.28686702164063860, -291.1656739007130454, -344.8769959924919135 ) ) ;
#18256 = CARTESIAN_POINT ( 'NONE',  ( -74.72115548864442758, -280.7481394762687614, -207.1369850336287470 ) ) ;
#18257 = CARTESIAN_POINT ( 'NONE',  ( 153.2628468892384319, 20.37991841447902530, -11.93555113919326693 ) ) ;
#18258 = CARTESIAN_POINT ( 'NONE',  ( 7.630768672711631062, -294.6656197601119516, -210.2756722165279655 ) ) ;
#18259 = CARTESIAN_POINT ( 'NONE',  ( -76.94499345125609580, -277.7696563499561648, -205.4499775751690436 ) ) ;
#18260 = CARTESIAN_POINT ( 'NONE',  ( -3.813334485546819419, -277.2489309625477745, -335.3206543557988084 ) ) ;
#18261 = CARTESIAN_POINT ( 'NONE',  ( -102.8074662133553829, -286.0600908035551129, -307.4023939802898440 ) ) ;
#18262 = DIRECTION ( 'NONE',  ( 1.000000000000000000, 0.000000000000000000, 0.000000000000000000 ) ) ;
#18263 = CARTESIAN_POINT ( 'NONE',  ( -73.71231011845847547, -291.4511664098068309, -336.6064918894743414 ) ) ;
#18264 = CARTESIAN_POINT ( 'NONE',  ( -7.396603977905934713, -285.6319899620386309, -199.5412390962606537 ) ) ;
#18265 = CARTESIAN_POINT ( 'NONE',  ( -94.90220160730498833, -289.5979389577954635, -224.1541500511134188 ) ) ;
#18266 = DIRECTION ( 'NONE',  ( -0.000000000000000000, -0.000000000000000000, 1.000000000000000000 ) ) ;
#18267 = CARTESIAN_POINT ( 'NONE',  ( -21.56336194408209295, -275.5305643681177798, -342.1928954265484322 ) ) ;
#18268 = CARTESIAN_POINT ( 'NONE',  ( -76.32655861281827470, -293.7185316948441596, -333.5957865230379298 ) ) ;
#18269 = CARTESIAN_POINT ( 'NONE',  ( 185.4166944662832179, 249.5000000000000568, 22.87680765314684095 ) ) ;
#18270 = DIRECTION ( 'NONE',  ( 1.000000000000000000, 0.000000000000000000, 0.000000000000000000 ) ) ;
#18271 = CARTESIAN_POINT ( 'NONE',  ( -113.6747595037471825, -289.0573677027789472, -268.3534615565037598 ) ) ;
#18272 = CARTESIAN_POINT ( 'NONE',  ( -60.24605010984494413, -287.3503279879221850, -200.2053543853141946 ) ) ;
#18273 = CARTESIAN_POINT ( 'NONE',  ( -41.72480855978398750, -287.3464898732314055, -346.2343162145714928 ) ) ;
#18274 = CARTESIAN_POINT ( 'NONE',  ( -30.49438800603590494, -287.5655683001523926, -197.0399350469283490 ) ) ;
#18275 = DIRECTION ( 'NONE',  ( 0.000000000000000000, 0.000000000000000000, 1.000000000000000000 ) ) ;
#18276 = CARTESIAN_POINT ( 'NONE',  ( -6.958753548722762972, -287.2641888718219434, -203.7930360852606668 ) ) ;
#18277 = CARTESIAN_POINT ( 'NONE',  ( -11.73637659663021005, -294.3636547049829915, -199.4347522718885841 ) ) ;
#18278 = CARTESIAN_POINT ( 'NONE',  ( -72.19855777007330744, -275.5893553945859935, -337.4151912561971471 ) ) ;
#18279 = CARTESIAN_POINT ( 'NONE',  ( -82.53044031078729859, -277.9841851222492437, -332.6806338033837847 ) ) ;
#18280 = CARTESIAN_POINT ( 'NONE',  ( -70.24808225174567156, -289.7017472216109013, -202.3428541240881202 ) ) ;
#18281 = CARTESIAN_POINT ( 'NONE',  ( -113.0656290635832306, -278.3766548836172205, -284.3937385022919102 ) ) ;
#18282 = CARTESIAN_POINT ( 'NONE',  ( -108.5816486204953861, -274.7547308092517255, -248.5930579052022154 ) ) ;
#18283 = CARTESIAN_POINT ( 'NONE',  ( -48.18343439339133027, -266.0193969580721500, -497.3422536412488739 ) ) ;
#18284 = CARTESIAN_POINT ( 'NONE',  ( -112.3193019311769802, -282.5090842981202854, -273.7025136179500464 ) ) ;
#18285 = DIRECTION ( 'NONE',  ( 0.000000000000000000, 1.000000000000000000, 0.000000000000000000 ) ) ;
#18286 = CARTESIAN_POINT ( 'NONE',  ( -100.5064813694413601, -277.2217546671208765, -231.2621292671309732 ) ) ;
#18287 = CARTESIAN_POINT ( 'NONE',  ( 33.70605846285116769, -279.8645509636867814, -294.5476827683453962 ) ) ;
#18288 = CARTESIAN_POINT ( 'NONE',  ( 140.6539576904058606, 250.5000000000000568, 12.00000000000000000 ) ) ;
#18289 = CARTESIAN_POINT ( 'NONE',  ( -70.02181117564433066, -275.9546630496021180, -339.3298907177352248 ) ) ;
#18290 = CARTESIAN_POINT ( 'NONE',  ( -106.4628282082076822, -298.4115358499530544, -244.6603995864948899 ) ) ;
#18291 = CARTESIAN_POINT ( 'NONE',  ( 32.10660875633151790, -280.8921610010549443, -303.0196274746199379 ) ) ;
#18292 = CARTESIAN_POINT ( 'NONE',  ( -110.4760157059144063, -297.4428570348641756, -274.2056377780733669 ) ) ;
#18293 = CARTESIAN_POINT ( 'NONE',  ( -112.1220714190733503, -298.0714665907510721, -254.1383988901473288 ) ) ;
#18294 = CARTESIAN_POINT ( 'NONE',  ( -63.31027542232896366, -273.3710172891319985, -202.1001258308832007 ) ) ;
#18295 = CARTESIAN_POINT ( 'NONE',  ( 36.17193796058025157, -295.3615418253664870, -255.5036058404894277 ) ) ;
#18296 = CARTESIAN_POINT ( 'NONE',  ( -0.9714313362855822032, -286.6880972751943091, -202.4921003638220043 ) ) ;
#18297 = CARTESIAN_POINT ( 'NONE',  ( -2.064208747467626726, -274.7296795769385085, -337.4118755073128568 ) ) ;
#18298 = CARTESIAN_POINT ( 'NONE',  ( -51.68738670159188331, -289.0641386776292734, -346.0129605326272895 ) ) ;
#18299 = CARTESIAN_POINT ( 'NONE',  ( 35.78837939086074726, -286.5480692379236416, -265.5832576960827964 ) ) ;
#18300 = CARTESIAN_POINT ( 'NONE',  ( -112.1902289058279649, -288.6131608084821778, -265.5968356571895015 ) ) ;
#18301 = VERTEX_POINT ( 'NONE', #4306 ) ;
#18302 = CARTESIAN_POINT ( 'NONE',  ( 138.4517698930976621, 181.0451598467585939, -241.7086681466011271 ) ) ;
#18303 = CARTESIAN_POINT ( 'NONE',  ( 1.338852219042856007, -288.0277098621103278, -332.3434002230237638 ) ) ;
#18304 = CARTESIAN_POINT ( 'NONE',  ( 209.2251716680733580, 29.17473719793202847, 13.08022668053246385 ) ) ;
#18305 = AXIS2_PLACEMENT_3D ( 'NONE', #9560, #9087, #60251 ) ;
#18306 = CARTESIAN_POINT ( 'NONE',  ( -100.8087374628426574, -286.0656555923040401, -227.0843837525586935 ) ) ;
#18307 = CARTESIAN_POINT ( 'NONE',  ( 24.63160540069702620, -292.0076466708025578, -225.0606807299236891 ) ) ;
#18308 = CARTESIAN_POINT ( 'NONE',  ( 38.08234982104021071, -283.2893557047473791, -281.2079195666263445 ) ) ;
#18309 = EDGE_CURVE ( 'NONE', #32677, #20110, #62327, .T. ) ;
#18310 = CARTESIAN_POINT ( 'NONE',  ( 37.76733636263002580, -282.6840814274303852, -255.8032709088620607 ) ) ;
#18311 = CARTESIAN_POINT ( 'NONE',  ( -24.06757760856137551, -282.7111811987912802, -342.1441081391535022 ) ) ;
#18312 = CARTESIAN_POINT ( 'NONE',  ( -13.11592327204001762, -278.7377274711695350, -341.3953809425485133 ) ) ;
#18313 = CARTESIAN_POINT ( 'NONE',  ( -111.9686479433488557, -296.3141915376422162, -289.3832339960862896 ) ) ;
#18314 = CARTESIAN_POINT ( 'NONE',  ( -74.53733417463298849, -274.8617465275469272, -206.9166063329775511 ) ) ;
#18315 = CARTESIAN_POINT ( 'NONE',  ( -96.40063748384056908, -289.2008518132910808, -224.7114879200104554 ) ) ;
#18316 = CARTESIAN_POINT ( 'NONE',  ( -77.67060023467416841, -296.4173304376658962, -209.0807987381998885 ) ) ;
#18317 = ORIENTED_EDGE ( 'NONE', *, *, #17688, .T. ) ;
#18318 = CARTESIAN_POINT ( 'NONE',  ( 145.2857639756989272, -299.5541904835127980, -195.3611179825600175 ) ) ;
#18319 = CARTESIAN_POINT ( 'NONE',  ( -91.77814820904001181, -285.7562145741270001, -321.1350022006735117 ) ) ;
#18320 = CARTESIAN_POINT ( 'NONE',  ( 11.01410912075678006, -295.4807995822081352, -329.9544167945544473 ) ) ;
#18321 = CARTESIAN_POINT ( 'NONE',  ( -110.3305589788174643, -285.2680457462315076, -265.4666329897965511 ) ) ;
#18322 = CARTESIAN_POINT ( 'NONE',  ( -17.43051541249591807, -275.8600503434624329, -344.4985912031687576 ) ) ;
#18323 = CARTESIAN_POINT ( 'NONE',  ( -94.64089820827537380, -291.9001253798788866, -219.0764742177589142 ) ) ;
#18324 = CARTESIAN_POINT ( 'NONE',  ( -94.86300598963997288, -283.3686914473223624, -220.9711510432449586 ) ) ;
#18325 = CARTESIAN_POINT ( 'NONE',  ( -42.05690816039972191, -292.3275221232314038, -193.5268085579447188 ) ) ;
#18326 = CARTESIAN_POINT ( 'NONE',  ( -58.69125990973581963, -289.6691393703586641, -340.2443291341762688 ) ) ;
#18327 = DIRECTION ( 'NONE',  ( -0.000000000000000000, -0.000000000000000000, -1.000000000000000000 ) ) ;
#18328 = DIRECTION ( 'NONE',  ( -0.000000000000000000, -0.000000000000000000, -1.000000000000000000 ) ) ;
#18329 = CARTESIAN_POINT ( 'NONE',  ( -93.40603346885242786, -239.0132304798418375, -338.5932674861245459 ) ) ;
#18330 = CARTESIAN_POINT ( 'NONE',  ( -87.31066565302292304, -286.8907088013344833, -212.6213123086534154 ) ) ;
#18331 = CARTESIAN_POINT ( 'NONE',  ( -37.37352853689063181, -274.5523547857346784, -350.3611179825600175 ) ) ;
#18332 = CARTESIAN_POINT ( 'NONE',  ( 24.38331233821165966, -281.0184361849308630, -310.0049992628653968 ) ) ;
#18333 = CARTESIAN_POINT ( 'NONE',  ( 18.88486615238925026, -275.9361726760148485, -322.9378955162528086 ) ) ;
#18334 = CARTESIAN_POINT ( 'NONE',  ( -35.64617060351280742, -282.0736016005465672, -195.5342762581041711 ) ) ;
#18335 = CARTESIAN_POINT ( 'NONE',  ( 201.0568784420084114, 286.4263594892526612, -96.83033023965205643 ) ) ;
#18336 = B_SPLINE_CURVE_WITH_KNOTS ( 'NONE', 3,
 ( #30186, #52421, #87918, #7474, #43460, #23069, #51947, #74198 ),
 .UNSPECIFIED., .F., .F.,
 ( 4, 2, 2, 4 ),
 ( 0.000000000000000000, 0.004220890787215657823, 0.006331336180823474158, 0.008441781574431289625 ),
 .UNSPECIFIED. ) ;
#18337 = CARTESIAN_POINT ( 'NONE',  ( -21.86321631561991197, -281.4322568384516217, -345.1877364426468375 ) ) ;
#18338 = CARTESIAN_POINT ( 'NONE',  ( -111.7370907227955286, -282.4935987225156850, -276.4580564721121618 ) ) ;
#18339 = CARTESIAN_POINT ( 'NONE',  ( 7.225731311262463485, -300.3629773498978466, -194.3612984979313296 ) ) ;
#18340 = CARTESIAN_POINT ( 'NONE',  ( -73.32725876020806766, -296.0356526961273858, -333.9459275809488759 ) ) ;
#18341 = EDGE_LOOP ( 'NONE', ( #58411, #43498, #17821, #33436 ) ) ;
#18342 = CARTESIAN_POINT ( 'NONE',  ( 32.27353337005490630, -291.9241983709223405, -246.6449432311666499 ) ) ;
#18343 = CARTESIAN_POINT ( 'NONE',  ( 18.83441953807343339, -276.9207081732492952, -322.8735580881307214 ) ) ;
#18344 = CARTESIAN_POINT ( 'NONE',  ( -14.06544176718584538, -274.3626910399229928, -201.1714092339545914 ) ) ;
#18345 = CARTESIAN_POINT ( 'NONE',  ( 26.68011411646424236, -273.9150457479317993, -228.1390880640642251 ) ) ;
#18346 = SPHERICAL_SURFACE ( 'NONE', #26517, 35.00000000000000000 ) ;
#18347 = CARTESIAN_POINT ( 'NONE',  ( -41.74507514058172575, -271.9966447099766924, -195.4400708904660178 ) ) ;
#18348 = CARTESIAN_POINT ( 'NONE',  ( 19.10674449089164284, -295.6836344961678265, -321.9375228146101904 ) ) ;
#18349 = DIRECTION ( 'NONE',  ( 0.000000000000000000, -0.000000000000000000, 1.000000000000000000 ) ) ;
#18350 = CARTESIAN_POINT ( 'NONE',  ( 196.3886764727502054, 69.83403101108301314, 15.08154681515735440 ) ) ;
#18351 = CARTESIAN_POINT ( 'NONE',  ( 10.11924011719783678, -283.4596903078389118, -326.2999295594663636 ) ) ;
#18352 = CARTESIAN_POINT ( 'NONE',  ( 24.29858650906719575, -283.9095344624773816, -314.8179868824415166 ) ) ;
#18353 = CARTESIAN_POINT ( 'NONE',  ( -108.1940675032278989, -283.6635518405900598, -288.3565258922605494 ) ) ;
#18354 = CARTESIAN_POINT ( 'NONE',  ( -4.730722392483621697, -275.0152028402754354, -336.5791208309219087 ) ) ;
#18355 = CARTESIAN_POINT ( 'NONE',  ( -51.22607520076802956, -285.0917998893116305, -343.3387975395382341 ) ) ;
#18356 = CARTESIAN_POINT ( 'NONE',  ( -70.78458020693736330, -275.9815293573620352, -336.0290822138302360 ) ) ;
#18357 = CARTESIAN_POINT ( 'NONE',  ( 7.509228036664423733, -275.7603803280447323, -212.3730130350662648 ) ) ;
#18358 = CARTESIAN_POINT ( 'NONE',  ( 76.08708295871279859, -293.9068999365417199, -472.6442049081569508 ) ) ;
#18359 = CARTESIAN_POINT ( 'NONE',  ( -79.83002468411946495, -280.2965779664895649, -206.2746259123988182 ) ) ;
#18360 = EDGE_LOOP ( 'NONE', ( #51758, #45305, #36181, #89373, #22755, #67260 ) ) ;
#18361 = CARTESIAN_POINT ( 'NONE',  ( 198.3325868694606129, 18.45344983985999576, 10.88803913699904058 ) ) ;
#18362 = CARTESIAN_POINT ( 'NONE',  ( -113.1056973315731966, -286.4170123369935936, -270.0115389209612999 ) ) ;
#18363 = CARTESIAN_POINT ( 'NONE',  ( -58.46460753996408499, -294.5295006818424781, -340.4069923010587786 ) ) ;
#18364 = CARTESIAN_POINT ( 'NONE',  ( -85.10785998166716126, -289.0402029797772343, -330.6927059614688460 ) ) ;
#18365 = CARTESIAN_POINT ( 'NONE',  ( 32.80808305380109857, -285.4827918182606368, -246.7606533143973309 ) ) ;
#18367 = CARTESIAN_POINT ( 'NONE',  ( -93.30825996101474118, -289.4727319290576020, -221.9285029829443943 ) ) ;
#18366 = CARTESIAN_POINT ( 'NONE',  ( -41.33691636436198991, -284.5756255925609253, -196.8678193536470644 ) ) ;
#18368 = CARTESIAN_POINT ( 'NONE',  ( -109.8884489380969995, -285.6067999126984773, -281.8267593677636000 ) ) ;
#18369 = CARTESIAN_POINT ( 'NONE',  ( 35.29523946558853709, -273.7919793457811011, -289.0393314526837116 ) ) ;
#18370 = CARTESIAN_POINT ( 'NONE',  ( 37.77176312748893139, -285.7890140262398972, -257.4620678854868743 ) ) ;
#18371 = CARTESIAN_POINT ( 'NONE',  ( -4.530601066288855172, -300.4630443658264198, -195.3499233714474883 ) ) ;
#18372 = CARTESIAN_POINT ( 'NONE',  ( 37.26752328373940770, -285.6744022905064639, -279.9160227446806175 ) ) ;
#18373=STYLED_ITEM('',(#93738),#58100);
#18374 = CARTESIAN_POINT ( 'NONE',  ( 35.75397222753428395, -282.4339738131332069, -265.8410371840897142 ) ) ;
#18375 = CARTESIAN_POINT ( 'NONE',  ( -96.69588962739648252, -291.9213121728802776, -316.4817057893731089 ) ) ;
#18376 = DIRECTION ( 'NONE',  ( 1.000000000000000000, 0.000000000000000000, 0.000000000000000000 ) ) ;
#18377 = CARTESIAN_POINT ( 'NONE',  ( 161.2244399300530233, 8.542400036368780647, 13.00000000000000178 ) ) ;
#18378 = CARTESIAN_POINT ( 'NONE',  ( -81.01900643457557294, -297.5599272582323351, -332.0821831314446513 ) ) ;
#18379 = AXIS2_PLACEMENT_3D ( 'NONE', #1278, #36796, #9287 ) ;
#18380 = CARTESIAN_POINT ( 'NONE',  ( -93.69480426405918649, -277.2397834031085040, -220.8509003234753152 ) ) ;
#18381 = CARTESIAN_POINT ( 'NONE',  ( -61.62783006586693091, -290.9417541253687318, -197.4055430577087122 ) ) ;
#18382 = CARTESIAN_POINT ( 'NONE',  ( -109.6728350530508749, -294.7600250780283204, -285.0749835905743339 ) ) ;
#18383 = CARTESIAN_POINT ( 'NONE',  ( 22.20171578081307828, -280.8358549310615899, -313.4619473941257866 ) ) ;
#18384 = CARTESIAN_POINT ( 'NONE',  ( 6.035317756951685375, -272.7251112422953838, -209.8015384451072975 ) ) ;
#18385 = CARTESIAN_POINT ( 'NONE',  ( 23.34964704074147335, -295.4412049857933766, -311.8965365310359061 ) ) ;
#18386 = CARTESIAN_POINT ( 'NONE',  ( -114.2704648735229114, -299.0519495502701943, -270.3937649182068981 ) ) ;
#18387 = CARTESIAN_POINT ( 'NONE',  ( -113.2750847673237473, -271.2343597877220418, -261.8330824893644149 ) ) ;
#18388 = CARTESIAN_POINT ( 'NONE',  ( -37.70690519882273861, -293.2964959873205544, -346.3598162958504645 ) ) ;
#18389 = CARTESIAN_POINT ( 'NONE',  ( 0.1941150956643828696, -293.9878825109966556, -207.0646923910180703 ) ) ;
#18390 = CARTESIAN_POINT ( 'NONE',  ( 175.2296996224750103, 246.0000000000001137, 9.550761578869391144 ) ) ;
#18391 = CARTESIAN_POINT ( 'NONE',  ( 28.88033943207292964, -293.9343733726302617, -239.1410542765987941 ) ) ;
#18392 = CARTESIAN_POINT ( 'NONE',  ( -47.80257052418233599, -229.5268262511776527, -22.50000000000000000 ) ) ;
#18394 = CARTESIAN_POINT ( 'NONE',  ( -72.12457855193380851, -295.5257536212666878, -334.5560021791729923 ) ) ;
#18393 = CARTESIAN_POINT ( 'NONE',  ( -31.78331882588462776, -281.0024623258355518, -345.5240273004843630 ) ) ;
#18395 = CARTESIAN_POINT ( 'NONE',  ( -38.73254726487297717, -283.0691454756642429, -347.3485555567647793 ) ) ;
#18396 = CARTESIAN_POINT ( 'NONE',  ( -113.1169260718744880, -284.0455835643530804, -284.2133555584199485 ) ) ;
#18397 = CARTESIAN_POINT ( 'NONE',  ( -87.98845329025873241, -287.7618270266485752, -325.5216806314459177 ) ) ;
#18398 = CARTESIAN_POINT ( 'NONE',  ( -31.70697657339797360, -281.4621583456681719, -346.4726083548007978 ) ) ;
#18399 = CARTESIAN_POINT ( 'NONE',  ( 37.52018884129815035, -286.6822969570134205, -287.0700498393146631 ) ) ;
#18400 = CYLINDRICAL_SURFACE ( 'NONE', #5292, 4.025000000000000355 ) ;
#18401 = CARTESIAN_POINT ( 'NONE',  ( -28.78319214298199924, -296.5421137496775259, -343.7147542609420725 ) ) ;
#18402 = CARTESIAN_POINT ( 'NONE',  ( -42.74624004448296688, -278.5443619850103119, -346.5805199832682320 ) ) ;
#18403 = CARTESIAN_POINT ( 'NONE',  ( -107.9919616646128020, -278.4630570509071390, -251.8559034820763145 ) ) ;
#18404 = CARTESIAN_POINT ( 'NONE',  ( 36.28635803359426149, -293.4358472490957297, -247.8242802307763668 ) ) ;
#18405 = CARTESIAN_POINT ( 'NONE',  ( -78.39818155954780821, -281.6799034817786378, -333.7935980615562244 ) ) ;
#18406 = EDGE_CURVE ( 'NONE', #48629, #83166, #44192, .T. ) ;
#18407 = CARTESIAN_POINT ( 'NONE',  ( 18.66424552418422067, -291.9426537540517756, -223.1727454704056299 ) ) ;
#18408 = CARTESIAN_POINT ( 'NONE',  ( -112.3378101070132118, -294.5618006904203980, -269.5968316089573023 ) ) ;
#18409 = ORIENTED_EDGE ( 'NONE', *, *, #36263, .F. ) ;
#18410 = CARTESIAN_POINT ( 'NONE',  ( 18.87643636612662590, -293.7211003753546947, -317.0249109163572143 ) ) ;
#18411 = CARTESIAN_POINT ( 'NONE',  ( 205.7381008070598227, 0.000000000000000000, -7.000000000000000888 ) ) ;
#18412 = CARTESIAN_POINT ( 'NONE',  ( -67.74223827176246004, -292.9809262143061233, -333.4151289067050357 ) ) ;
#18413 = CARTESIAN_POINT ( 'NONE',  ( -105.4610463756093282, -272.2102085557035593, -234.6945883984020895 ) ) ;
#18414 = CARTESIAN_POINT ( 'NONE',  ( 37.95797195979628924, -279.5793392145899929, -261.5180435393053244 ) ) ;
#18415 = CARTESIAN_POINT ( 'NONE',  ( 25.13266511648668455, -288.2788703601202656, -226.1768802954254056 ) ) ;
#18416 = CARTESIAN_POINT ( 'NONE',  ( -10.72607798969518100, -288.5285787855301010, -338.3903922582085784 ) ) ;
#18417 = CARTESIAN_POINT ( 'NONE',  ( -109.9660872728296823, -279.9078790343306764, -282.9418373914640483 ) ) ;
#18418 = CARTESIAN_POINT ( 'NONE',  ( -35.13193294281806089, -299.8403252642999064, -196.3471044052115531 ) ) ;
#18419 = CARTESIAN_POINT ( 'NONE',  ( -41.89647546744252082, -275.9057098341030496, -343.6293937646144059 ) ) ;
#18420 = ORIENTED_EDGE ( 'NONE', *, *, #41482, .F. ) ;
#18421 = CARTESIAN_POINT ( 'NONE',  ( -46.12324694399156755, -297.6103718778445568, -193.8847900960857373 ) ) ;
#18422 = CARTESIAN_POINT ( 'NONE',  ( -106.4407881742127415, -292.1072631825048802, -298.1874343066943993 ) ) ;
#18423 = CARTESIAN_POINT ( 'NONE',  ( 38.91105295877255088, -295.1513832562801554, -270.2901514668143363 ) ) ;
#18424 = CARTESIAN_POINT ( 'NONE',  ( 197.0359635097977389, 71.72764050497774235, -10.24344765926147893 ) ) ;
#18425 = EDGE_CURVE ( 'NONE', #44526, #43675, #70598, .T. ) ;
#18426 = CARTESIAN_POINT ( 'NONE',  ( -95.20014861465652700, -291.8317314030039711, -225.6812275701722967 ) ) ;
#18427 = CARTESIAN_POINT ( 'NONE',  ( -48.18343439339133027, -256.0722001993605090, -452.3316844813846842 ) ) ;
#18428 = EDGE_LOOP ( 'NONE', ( #18645, #81540, #84775, #63444 ) ) ;
#18429 = CARTESIAN_POINT ( 'NONE',  ( 37.11581992329399782, -291.5136227898073571, -256.3474392927533927 ) ) ;
#18430 = CARTESIAN_POINT ( 'NONE',  ( -34.76457602019346638, -298.4168711406839520, -193.3821205562305749 ) ) ;
#18431 = LINE ( 'NONE', #12270, #89616 ) ;
#18432 = CIRCLE ( 'NONE', #24447, 1.000000000000000000 ) ;
#18433 = CARTESIAN_POINT ( 'NONE',  ( 195.9492931686500583, 25.28061950067115404, 13.99099524138373418 ) ) ;
#18434 = CARTESIAN_POINT ( 'NONE',  ( -88.20189736861073015, -292.8751920107506521, -213.4757236552805466 ) ) ;
#18435 = CARTESIAN_POINT ( 'NONE',  ( 13.79469577742117714, -289.1948066931273615, -206.1857440867352693 ) ) ;
#18436 = CARTESIAN_POINT ( 'NONE',  ( -90.99463444515654942, -287.2888084190585118, -218.1197759237803382 ) ) ;
#18437 = CARTESIAN_POINT ( 'NONE',  ( 29.51023075727174572, -273.1067905951841226, -236.7330380446502716 ) ) ;
#18438 = CARTESIAN_POINT ( 'NONE',  ( -11.00315423067759291, -276.3181981698037362, -200.6813397741311462 ) ) ;
#18440 = CARTESIAN_POINT ( 'NONE',  ( -82.58524743923179301, -289.5088510396396373, -211.1830014874893493 ) ) ;
#18439 = CIRCLE ( 'NONE', #9375, 0.9999999999999977796 ) ;
#18441 = CARTESIAN_POINT ( 'NONE',  ( -71.00047182164078663, -279.3519837230407461, -338.2388947022027423 ) ) ;
#18442 = EDGE_CURVE ( 'NONE', #60346, #70318, #88042, .T. ) ;
#18444 = CARTESIAN_POINT ( 'NONE',  ( 29.40414618432475180, -281.3031394763017943, -300.2995432541271157 ) ) ;
#18443 = CARTESIAN_POINT ( 'NONE',  ( -70.94166808009228475, -279.5959073069824967, -205.5392982787042513 ) ) ;
#18445 = CARTESIAN_POINT ( 'NONE',  ( -38.52634079958206570, -278.1463461582590071, -347.0428572528606992 ) ) ;
#18446 = CARTESIAN_POINT ( 'NONE',  ( 36.80359155852602981, -280.5892394684449869, -289.6090903544763364 ) ) ;
#18447 = CARTESIAN_POINT ( 'NONE',  ( 199.7552170467075712, 291.4512671170426188, -82.50257151101990871 ) ) ;
#18448 = CARTESIAN_POINT ( 'NONE',  ( 7.089010765944712134, -275.5818951274637243, -207.6961129891504640 ) ) ;
#18449 = CARTESIAN_POINT ( 'NONE',  ( -92.68278473143705298, -274.7969085751452667, -217.8056560969009183 ) ) ;
#18450 = CARTESIAN_POINT ( 'NONE',  ( -109.1418805571601069, -281.0519495502701943, -270.3937649182068412 ) ) ;
#18451 = EDGE_LOOP ( 'NONE', ( #81543, #43240, #57627, #38795 ) ) ;
#18452 = CARTESIAN_POINT ( 'NONE',  ( 132.9888089158688445, -299.5541904835127980, -195.3611179825600175 ) ) ;
#18453 = CARTESIAN_POINT ( 'NONE',  ( -74.86234805680348359, -290.6440936569449605, -333.3554419440064294 ) ) ;
#18454 = CARTESIAN_POINT ( 'NONE',  ( 9.172542058821463229, -288.4412471137406442, -210.2745197673373525 ) ) ;
#18455 = CARTESIAN_POINT ( 'NONE',  ( -61.29623385734826968, -288.7202146284037667, -339.4268329349933992 ) ) ;
#18456 = CARTESIAN_POINT ( 'NONE',  ( -52.15528865565833172, -285.3751840040727075, -194.8078682744807963 ) ) ;
#18457 = CARTESIAN_POINT ( 'NONE',  ( 164.7123623445222904, 3.000000000000000000, -9.000000000000001776 ) ) ;
#18458 = CARTESIAN_POINT ( 'NONE',  ( -38.92242558352145920, -281.4721431534111957, -344.1568175633397004 ) ) ;
#18459 = CARTESIAN_POINT ( 'NONE',  ( -26.26761788924477159, -290.7702737032774394, -343.8175978330015141 ) ) ;
#18460 = CARTESIAN_POINT ( 'NONE',  ( -98.11500255970440776, -282.4562482126055443, -312.1311791736333703 ) ) ;
#18461 = CARTESIAN_POINT ( 'NONE',  ( -99.89622763267232131, -280.3968329430364861, -231.6871321728701787 ) ) ;
#18462 =( REPRESENTATION_RELATIONSHIP ('NONE','NONE', #78428, #54338 ) REPRESENTATION_RELATIONSHIP_WITH_TRANSFORMATION ( #79034 )SHAPE_REPRESENTATION_RELATIONSHIP( ) );
#18463 = CARTESIAN_POINT ( 'NONE',  ( -37.80386070040891866, -277.5504071699263022, -343.4336584521614100 ) ) ;
#18464 = CARTESIAN_POINT ( 'NONE',  ( -112.2484377030699392, -289.5493506667588122, -254.2684024630390525 ) ) ;
#18465 = CARTESIAN_POINT ( 'NONE',  ( -64.49970297386390428, -286.5093623257991453, -198.4679023020324564 ) ) ;
#18466 = CARTESIAN_POINT ( 'NONE',  ( -68.48160212870322994, -286.1462142809880902, -199.9917000953179524 ) ) ;
#18467 = CARTESIAN_POINT ( 'NONE',  ( -78.37487713596070193, -283.7883067704338487, -330.7372588755456491 ) ) ;
#18468 = ORIENTED_EDGE ( 'NONE', *, *, #44642, .F. ) ;
#18469 = CARTESIAN_POINT ( 'NONE',  ( 158.6539576904058606, 293.9636489450775230, 9.103929867429224387 ) ) ;
#18470 = CARTESIAN_POINT ( 'NONE',  ( -95.42856207035013938, -291.7469979246462799, -319.0250604810841537 ) ) ;
#18471 = CARTESIAN_POINT ( 'NONE',  ( 25.30118074852753907, -292.8218021461206604, -314.3062669074489008 ) ) ;
#18472 = CARTESIAN_POINT ( 'NONE',  ( 7.484358705474618567, -273.7397821557955240, -212.4471050251708846 ) ) ;
#18473 = CARTESIAN_POINT ( 'NONE',  ( -95.50983521154761036, -295.2203989268954842, -320.6580448047077994 ) ) ;
#18474 = CARTESIAN_POINT ( 'NONE',  ( -47.06698309518480272, -290.4062500512792440, -197.3123218074406964 ) ) ;
#18475 = CARTESIAN_POINT ( 'NONE',  ( -97.24153419482951222, -294.1917087564575581, -313.8567035752797665 ) ) ;
#18476 = CARTESIAN_POINT ( 'NONE',  ( -101.9856345685396661, -291.2844843612261343, -305.2293317523063365 ) ) ;
#18477 = DIRECTION ( 'NONE',  ( 1.000000000000000000, 0.000000000000000000, 0.000000000000000000 ) ) ;
#18478 = CARTESIAN_POINT ( 'NONE',  ( 31.65196417039437549, -291.1625969193617038, -240.5298808247407294 ) ) ;
#18479 = CARTESIAN_POINT ( 'NONE',  ( 29.77500962608763402, -295.1091140089343412, -236.7746029264955610 ) ) ;
#18480 = CARTESIAN_POINT ( 'NONE',  ( 27.86218812237793685, -288.0404830029386289, -236.9047559861107004 ) ) ;
#18481 = CARTESIAN_POINT ( 'NONE',  ( 18.79336908817745311, -276.8345957236899153, -220.0125979619869270 ) ) ;
#18482 = CARTESIAN_POINT ( 'NONE',  ( -42.79330527075682511, -275.9144385164120195, -346.7698132997780931 ) ) ;
#18483 = CARTESIAN_POINT ( 'NONE',  ( -106.3637795446746139, -296.1838346164104223, -236.5955826987196815 ) ) ;
#18484 = CARTESIAN_POINT ( 'NONE',  ( 35.70358694253413034, -273.9512698972658882, -282.6016998127785769 ) ) ;
#18485 = CARTESIAN_POINT ( 'NONE',  ( -77.58008269017265945, -277.5877919087350847, -207.6723184437707062 ) ) ;
#18486 = CARTESIAN_POINT ( 'NONE',  ( -59.61064535139623644, -274.9624389552184880, -200.3706139979180421 ) ) ;
#18487 = CARTESIAN_POINT ( 'NONE',  ( -67.41186304433895771, -275.8399085361755851, -340.3770141698942666 ) ) ;
#18488 = DIRECTION ( 'NONE',  ( -0.000000000000000000, 1.000000000000000000, -0.000000000000000000 ) ) ;
#18489 = CARTESIAN_POINT ( 'NONE',  ( -59.51444554745580717, -274.4088655965707630, -200.6499403494055116 ) ) ;
#18490 = CARTESIAN_POINT ( 'NONE',  ( 85.55100297371598117, -373.0521521680024648, -421.1172536214571096 ) ) ;
#18491 = AXIS2_PLACEMENT_3D ( 'NONE', #43749, #1146, #8244 ) ;
#18493 = CARTESIAN_POINT ( 'NONE',  ( -6.527050292322345015, -274.3018033424677355, -204.1836493090405895 ) ) ;
#18492 = CARTESIAN_POINT ( 'NONE',  ( -29.18091182051923482, -286.9694728694363448, -345.3255032745319681 ) ) ;
#18494 = VECTOR ( 'NONE', #68602, 1000.000000000000000 ) ;
#18495 = CARTESIAN_POINT ( 'NONE',  ( 32.86487654107115475, -287.9560881104892474, -301.9844731555711519 ) ) ;
#18496 = CARTESIAN_POINT ( 'NONE',  ( -110.7629650729319195, -289.9261408980842702, -293.6667020781873134 ) ) ;
#18497 = CARTESIAN_POINT ( 'NONE',  ( -112.5093130267115811, -274.5878523694335058, -267.5873348197950463 ) ) ;
#18498 = CARTESIAN_POINT ( 'NONE',  ( -107.5163721759210489, -294.8918204388995150, -244.2205633017366040 ) ) ;
#18499 = AXIS2_PLACEMENT_3D ( 'NONE', #2212, #30616, #60906 ) ;
#18500 = CARTESIAN_POINT ( 'NONE',  ( -2.454303412367441872, -279.6989473726712845, -201.8845450564031978 ) ) ;
#18501 = CARTESIAN_POINT ( 'NONE',  ( 165.2688068684385883, 275.0000000000000568, 21.83530662808711398 ) ) ;
#18502 = AXIS2_PLACEMENT_3D ( 'NONE', #792, #21160, #51419 ) ;
#18503 = CARTESIAN_POINT ( 'NONE',  ( -109.1708615965814033, -276.2734586993274775, -291.9824285362325895 ) ) ;
#18504 = FACE_OUTER_BOUND ( 'NONE', #73551, .T. ) ;
#18505 = CARTESIAN_POINT ( 'NONE',  ( -110.7646170361288114, -289.3723260364604357, -268.4361161895217265 ) ) ;
#18506 = CARTESIAN_POINT ( 'NONE',  ( 160.5350683151633291, 250.5000000000000568, 20.22542485937379908 ) ) ;
#18507 = CARTESIAN_POINT ( 'NONE',  ( -110.6605081141568832, -288.7547481662529094, -254.5702013393155596 ) ) ;
#18508 = CARTESIAN_POINT ( 'NONE',  ( -51.71546725106541942, -275.3851976807318351, -198.0308801878181839 ) ) ;
#18509 = CARTESIAN_POINT ( 'NONE',  ( 37.67274262819614705, -282.7941619088899188, -255.8201526687256546 ) ) ;
#18511 = CARTESIAN_POINT ( 'NONE',  ( -84.86177938539310617, -283.7293326280835117, -325.7762970166370451 ) ) ;
#18510 = CARTESIAN_POINT ( 'NONE',  ( 51.20065605406508524, -297.1753657202241925, -195.0356064417869959 ) ) ;
#18512 = CARTESIAN_POINT ( 'NONE',  ( -87.75003621855245228, -274.7568427906131205, -216.6781383874958351 ) ) ;
#18513 = CARTESIAN_POINT ( 'NONE',  ( 30.32026780601015759, -275.9812329556879718, -242.3990187832259267 ) ) ;
#18514 = CARTESIAN_POINT ( 'NONE',  ( -72.52545093352124184, -287.5939705805653261, -337.2442618739322597 ) ) ;
#18515 = CARTESIAN_POINT ( 'NONE',  ( -73.29425776864243858, -285.5286868697865543, -336.2401334786221696 ) ) ;
#18516 = EDGE_CURVE ( 'NONE', #78809, #49098, #81957, .T. ) ;
#18517 = CARTESIAN_POINT ( 'NONE',  ( -98.09166856217510144, -272.0415002934558970, -229.2380635246693714 ) ) ;
#18518 = ORIENTED_EDGE ( 'NONE', *, *, #62083, .T. ) ;
#18519 = CARTESIAN_POINT ( 'NONE',  ( 175.2296996224750103, 149.6461846693799487, 0.000000000000000000 ) ) ;
#18520 = CARTESIAN_POINT ( 'NONE',  ( 15.47714442649860977, -294.1630452527837747, -326.3894114101727837 ) ) ;
#18521 = CARTESIAN_POINT ( 'NONE',  ( -80.27548315869583462, -287.4478143251849360, -209.2358994350518913 ) ) ;
#18522 = CARTESIAN_POINT ( 'NONE',  ( 143.2307367095235406, -0.4142135623730943128, 22.50000000000000000 ) ) ;
#18523 = CARTESIAN_POINT ( 'NONE',  ( -99.86837403722181250, -270.6952119285918457, -220.4570493818173702 ) ) ;
#18524 = CARTESIAN_POINT ( 'NONE',  ( -114.2160391143859357, -277.7697950614236220, -268.7274546917865337 ) ) ;
#18525 = CARTESIAN_POINT ( 'NONE',  ( -103.1182682241300483, -288.4449194479786343, -308.9347854765167085 ) ) ;
#18526 = CARTESIAN_POINT ( 'NONE',  ( -38.88032747611086393, -284.5918887233277133, -344.0509995412723470 ) ) ;
#18527 = CARTESIAN_POINT ( 'NONE',  ( -74.50293818045901162, -279.3139269816320507, -334.3690581167077767 ) ) ;
#18528 = CARTESIAN_POINT ( 'NONE',  ( -102.0293772130001742, -286.5140770273969224, -229.6903579021214910 ) ) ;
#18529 = CARTESIAN_POINT ( 'NONE',  ( 3.779841757612731890, -282.6053565897504996, -207.5770524743816452 ) ) ;
#18530 = CARTESIAN_POINT ( 'NONE',  ( -21.35686202443334736, -274.4184003559284406, -195.0385784921492984 ) ) ;
#18531 = CARTESIAN_POINT ( 'NONE',  ( -20.12816954715411910, -276.6703201100349361, -345.4671147148210366 ) ) ;
#18532 = CARTESIAN_POINT ( 'NONE',  ( -35.59274164050663103, -296.9502258989028292, -344.7933157173953873 ) ) ;
#18533 = SPHERICAL_SURFACE ( 'NONE', #53551, 1.000000000000000000 ) ;
#18534 = EDGE_CURVE ( 'NONE', #25794, #32648, #6433, .T. ) ;
#18535 = CARTESIAN_POINT ( 'NONE',  ( 139.6539576904058606, 132.0000000000000568, 12.50000000000000000 ) ) ;
#18536 = CARTESIAN_POINT ( 'NONE',  ( -86.64028556492256428, -295.5154585552031676, -212.7597672193894027 ) ) ;
#18537 = CARTESIAN_POINT ( 'NONE',  ( -40.51470909172113721, -276.6007421237648032, -343.3661982498928182 ) ) ;
#18538 = CARTESIAN_POINT ( 'NONE',  ( -112.6806232171716147, -273.9350040771517456, -256.2192089527511598 ) ) ;
#18539 = CARTESIAN_POINT ( 'NONE',  ( -46.87733123603825192, -287.6897051722824585, -196.9131398999693090 ) ) ;
#18540 = CARTESIAN_POINT ( 'NONE',  ( -58.63907948225442368, -296.8426682684632851, -343.6905287430371914 ) ) ;
#18541 = CARTESIAN_POINT ( 'NONE',  ( -113.7261772695988498, -297.8382084821406011, -263.9192050118442694 ) ) ;
#18542 = CARTESIAN_POINT ( 'NONE',  ( -111.9482925418126200, -292.4692947655991588, -276.8126949973831188 ) ) ;
#18543 = CARTESIAN_POINT ( 'NONE',  ( -95.34582016535756566, -277.2049161315813421, -223.0795096187027582 ) ) ;
#18544 = CARTESIAN_POINT ( 'NONE',  ( -107.8157848462118267, -280.7865802559705344, -246.2293998910118944 ) ) ;
#18545 = CARTESIAN_POINT ( 'NONE',  ( -109.5242528875122758, -270.8201157981344522, -251.1493279800756682 ) ) ;
#18546 = CARTESIAN_POINT ( 'NONE',  ( -108.1401228059177413, -286.0638054887901376, -297.4866024634024484 ) ) ;
#18547 = CARTESIAN_POINT ( 'NONE',  ( 30.76729199987585517, -286.8354246339021074, -297.6160624550819875 ) ) ;
#18548 = CARTESIAN_POINT ( 'NONE',  ( 86.20037202169200441, 82.24261404803831965, -301.9681809940666426 ) ) ;
#18549 = ORIENTED_EDGE ( 'NONE', *, *, #73250, .T. ) ;
#18550 = CARTESIAN_POINT ( 'NONE',  ( -7.003848871517688757, -286.1282589226604500, -203.9267403824592009 ) ) ;
#18551 = VERTEX_POINT ( 'NONE', #78166 ) ;
#18552 = CARTESIAN_POINT ( 'NONE',  ( -18.97902861234918603, -283.9009467438962133, -344.8759460500657497 ) ) ;
#18553 = CARTESIAN_POINT ( 'NONE',  ( -36.74015813344699666, -274.3931973679943894, -197.3300331140614503 ) ) ;
#18554 = CARTESIAN_POINT ( 'NONE',  ( -4.927943124689051047, -285.2644750169177428, -200.9539348009649302 ) ) ;
#18555 = EDGE_CURVE ( 'NONE', #27314, #15179, #70130, .T. ) ;
#18556 = CARTESIAN_POINT ( 'NONE',  ( -14.30981169128479635, -281.2848034912624939, -197.0773072859016395 ) ) ;
#18557 = CARTESIAN_POINT ( 'NONE',  ( -187.9122233887894140, -89.54582641780471874, 21.50000000000000000 ) ) ;
#18558 = CARTESIAN_POINT ( 'NONE',  ( -17.19385563167945463, -281.8277685797074241, -196.7623943987474888 ) ) ;
#18559 = CARTESIAN_POINT ( 'NONE',  ( 6.168808037376875220, -280.9585432400838840, -206.8585198417224262 ) ) ;
#18560 = CARTESIAN_POINT ( 'NONE',  ( -102.0172624299487154, -288.4809262143061801, -239.1787733560258289 ) ) ;
#18561 = CARTESIAN_POINT ( 'NONE',  ( -103.5911469518875379, -256.6625002471756147, -326.7956433880881377 ) ) ;
#18562 = ORIENTED_EDGE ( 'NONE', *, *, #56142, .T. ) ;
#18563 = VECTOR ( 'NONE', #55539, 1000.000000000000000 ) ;
#18564 = CARTESIAN_POINT ( 'NONE',  ( 20.39755320262476346, -276.8941315215337227, -222.7564222560362452 ) ) ;
#18565 = CARTESIAN_POINT ( 'NONE',  ( 24.83231157103504927, -22.65643835391063021, -344.9118043155972373 ) ) ;
#18566 = AXIS2_PLACEMENT_3D ( 'NONE', #91481, #12420, #70209 ) ;
#18567 = CARTESIAN_POINT ( 'NONE',  ( 30.80602539222534020, -279.9748742791759923, -300.9466636241256765 ) ) ;
#18568 = CARTESIAN_POINT ( 'NONE',  ( 28.58519336549668566, -294.8148115627031416, -232.5772758524784365 ) ) ;
#18569 = CARTESIAN_POINT ( 'NONE',  ( -78.01333230909250460, -294.9630719902157807, -331.1652550965862929 ) ) ;
#18570 = CARTESIAN_POINT ( 'NONE',  ( -84.22388375057433052, -290.9347692804208236, -209.2891578344852519 ) ) ;
#18571 = CARTESIAN_POINT ( 'NONE',  ( 82.64890176555634582, -297.1582149144751384, -195.3611179825600175 ) ) ;
#18572 = AXIS2_PLACEMENT_3D ( 'NONE', #52616, #60220, #600 ) ;
#18574 = CARTESIAN_POINT ( 'NONE',  ( 36.42873542136356235, -285.9971159549807567, -273.8173957554118942 ) ) ;
#18573 = CARTESIAN_POINT ( 'NONE',  ( -109.7928274324748799, -294.8188106286953030, -294.6395125900769472 ) ) ;
#18575 = CARTESIAN_POINT ( 'NONE',  ( 13.73616695035188506, -294.6377686880034048, -216.4916742013536748 ) ) ;
#18576 = CARTESIAN_POINT ( 'NONE',  ( -107.8604164539242305, -285.5948094133122481, -291.1027325633305622 ) ) ;
#18577 = ORIENTED_EDGE ( 'NONE', *, *, #34294, .F. ) ;
#18578 = CARTESIAN_POINT ( 'NONE',  ( 21.12343286581323554, -293.8204302666478611, -220.5952018966825960 ) ) ;
#18579 = CIRCLE ( 'NONE', #63976, 8.222204860432958284 ) ;
#18580 = CARTESIAN_POINT ( 'NONE',  ( -48.33175769892876161, -283.6881636979160817, -342.5913545605537252 ) ) ;
#18581 = CARTESIAN_POINT ( 'NONE',  ( -110.4296214064108455, -295.6387926320588804, -247.2471196708307559 ) ) ;
#18582 = CARTESIAN_POINT ( 'NONE',  ( -114.0273298749362567, -291.4157025437480684, -265.5162226897136293 ) ) ;
#18583 = CARTESIAN_POINT ( 'NONE',  ( -44.89724817652989941, -292.4514122476036846, -193.7416616088525529 ) ) ;
#18584 = CARTESIAN_POINT ( 'NONE',  ( -86.72781777403862691, -289.9283186857657029, -324.1885169088473617 ) ) ;
#18585 = ORIENTED_EDGE ( 'NONE', *, *, #17028, .F. ) ;
#18586 = DIRECTION ( 'NONE',  ( 0.000000000000000000, 1.000000000000000000, 0.000000000000000000 ) ) ;
#18587 = CARTESIAN_POINT ( 'NONE',  ( -97.28247472248484939, -297.7838843707907586, -316.7012628366149443 ) ) ;
#18588 = CARTESIAN_POINT ( 'NONE',  ( -113.9446275073758841, -271.3472703805991273, -270.3458084817817735 ) ) ;
#18589 = CARTESIAN_POINT ( 'NONE',  ( -62.37815739355075095, -278.7771840396258654, -201.4847457254723793 ) ) ;
#18590 = VERTEX_POINT ( 'NONE', #92338 ) ;
#18591 = ORIENTED_EDGE ( 'NONE', *, *, #88682, .T. ) ;
#18592 = CARTESIAN_POINT ( 'NONE',  ( 9.477860672189608593, -274.1843785355497403, -209.3082259173498869 ) ) ;
#18593 = CARTESIAN_POINT ( 'NONE',  ( -82.35243724732998771, -295.9052413621246274, -211.9462956158240559 ) ) ;
#18594 = CARTESIAN_POINT ( 'NONE',  ( 20.15304636032786689, -278.0665701533766878, -317.3409233854697504 ) ) ;
#18595 = CARTESIAN_POINT ( 'NONE',  ( 26.34754225808038441, -273.1747192196713172, -232.1229909113000360 ) ) ;
#18596 = CARTESIAN_POINT ( 'NONE',  ( -55.88890868371046139, -296.5012793220153071, -341.4287923844375996 ) ) ;
#18597 = CARTESIAN_POINT ( 'NONE',  ( -96.35730656854710219, -298.2390007016339268, -226.8498718945271264 ) ) ;
#18598 = CARTESIAN_POINT ( 'NONE',  ( 155.3778607292159961, 21.00000000000000000, 15.20506116941399277 ) ) ;
#18599 = CARTESIAN_POINT ( 'NONE',  ( -67.87580672487833056, -299.2582721280604119, -200.4900846345941261 ) ) ;
#18600 = B_SPLINE_CURVE_WITH_KNOTS ( 'NONE', 3,
 ( #46211, #21910, #87667, #43665, #80119, #49837, #36567, #22817 ),
 .UNSPECIFIED., .F., .F.,
 ( 4, 2, 2, 4 ),
 ( 0.000000000000000000, 0.0004362529587405823499, 0.0008725059174811646999, 0.001745011834962329400 ),
 .UNSPECIFIED. ) ;
#18601 = CARTESIAN_POINT ( 'NONE',  ( 6.674283129644242862, -296.6017529348180801, -195.2094072685388255 ) ) ;
#18602 = CARTESIAN_POINT ( 'NONE',  ( 30.68345933375126222, -294.5626650876890267, -297.2666195342657716 ) ) ;
#18603 = CARTESIAN_POINT ( 'NONE',  ( -92.09956273180337405, -289.8250576462705226, -221.1797759443949758 ) ) ;
#18604 = CARTESIAN_POINT ( 'NONE',  ( 17.53318101573682242, -300.7392505651913552, -195.3424018486777527 ) ) ;
#18605 = CARTESIAN_POINT ( 'NONE',  ( 32.96607768530838456, -276.4436151914591733, -301.6076102977514779 ) ) ;
#18606 = CARTESIAN_POINT ( 'NONE',  ( -96.28262770702696116, -273.3229362806323479, -227.2078027785737788 ) ) ;
#18607 = CARTESIAN_POINT ( 'NONE',  ( 24.59315650731292635, -284.1116823501766362, -313.3079452837239955 ) ) ;
#18608 = CARTESIAN_POINT ( 'NONE',  ( -13.59102928407611799, -281.4349390235323085, -343.0880312014667197 ) ) ;
#18609 = AXIS2_PLACEMENT_3D ( 'NONE', #54978, #34149, #69656 ) ;
#18610 = CARTESIAN_POINT ( 'NONE',  ( -95.13966416192549502, -277.2134565693370973, -321.0829884165950148 ) ) ;
#18611 = PLANE ( 'NONE',  #12787 ) ;
#18612 = CARTESIAN_POINT ( 'NONE',  ( -107.5497577288777507, -283.4771448171619568, -290.9832934294973370 ) ) ;
#18613 = CARTESIAN_POINT ( 'NONE',  ( 18.40626901811734584, -280.2540963079276253, -320.8573954732515290 ) ) ;
#18614 = EDGE_CURVE ( 'NONE', #71727, #43403, #19914, .T. ) ;
#18615 = CARTESIAN_POINT ( 'NONE',  ( 33.45984166988934305, -274.3905349517042964, -290.4700070139122658 ) ) ;
#18616 = CARTESIAN_POINT ( 'NONE',  ( -62.21566128194445611, -279.3756608151099954, -341.1700691521882618 ) ) ;
#18617 = CARTESIAN_POINT ( 'NONE',  ( 201.0776230153480526, -147.7221692137691775, -8.778910157967986905 ) ) ;
#18618 = FACE_OUTER_BOUND ( 'NONE', #12059, .T. ) ;
#18619 = CARTESIAN_POINT ( 'NONE',  ( -35.83038556322976831, -296.3106919061331155, -194.3748902813860866 ) ) ;
#18620 = CARTESIAN_POINT ( 'NONE',  ( -68.23796041456832029, -279.4571092230173122, -338.8985272977748195 ) ) ;
#18621 = DIRECTION ( 'NONE',  ( 0.000000000000000000, -0.000000000000000000, 1.000000000000000000 ) ) ;
#18622 = CARTESIAN_POINT ( 'NONE',  ( -107.9484528984091867, -286.1235339959541193, -297.4140488612280251 ) ) ;
#18623 = ORIENTED_EDGE ( 'NONE', *, *, #12440, .F. ) ;
#18624 = CARTESIAN_POINT ( 'NONE',  ( 156.2095471516448413, 16.65459343288320682, -7.440913067427157301 ) ) ;
#18625 = CARTESIAN_POINT ( 'NONE',  ( 17.99197929496902049, -284.8448689015404511, -219.7144744771975127 ) ) ;
#18626 = CARTESIAN_POINT ( 'NONE',  ( 206.6398282674434483, 29.68967932838811663, 13.90950695095619771 ) ) ;
#18627 = CARTESIAN_POINT ( 'NONE',  ( -105.3354824887800305, -294.9788323073088350, -298.0012349176078601 ) ) ;
#18628 = CARTESIAN_POINT ( 'NONE',  ( 1.945534855811330122, -286.6598616586912271, -333.3482487854449232 ) ) ;
#18629 = CARTESIAN_POINT ( 'NONE',  ( 157.1249521815083483, 17.17215575532036453, -9.360165637272727324 ) ) ;
#18630 = CARTESIAN_POINT ( 'NONE',  ( -108.5992076279081004, -294.8561388165281869, -246.8007446595710235 ) ) ;
#18631 = CARTESIAN_POINT ( 'NONE',  ( 9.401446153870715250, -285.1615118574719645, -210.0470563836351801 ) ) ;
#18632 = CARTESIAN_POINT ( 'NONE',  ( 36.14698507957970008, -283.0569138900773396, -263.0520707572362085 ) ) ;
#18633 = CARTESIAN_POINT ( 'NONE',  ( -52.73454351943054519, -281.4864868028225828, -344.8261480084637469 ) ) ;
#18634 = CARTESIAN_POINT ( 'NONE',  ( -82.54626709963542908, -289.6897868643849847, -327.6808102786136487 ) ) ;
#18635 = AXIS2_PLACEMENT_3D ( 'NONE', #38279, #8931, #37809 ) ;
#18636 = CARTESIAN_POINT ( 'NONE',  ( -102.6873955946119565, -280.4352975536023678, -236.4076610719573068 ) ) ;
#18637 = CARTESIAN_POINT ( 'NONE',  ( 30.16656945971872972, -281.9775348375103476, -242.1612019583262736 ) ) ;
#18638 = CARTESIAN_POINT ( 'NONE',  ( 32.52697351381365820, -289.8998175570631588, -298.7274278242689434 ) ) ;
#18639 = ORIENTED_EDGE ( 'NONE', *, *, #76268, .T. ) ;
#18640 = AXIS2_PLACEMENT_3D ( 'NONE', #87630, #36527, #89 ) ;
#18641 = CARTESIAN_POINT ( 'NONE',  ( -104.2295303334646945, -273.0487839751910997, -232.1094138764649415 ) ) ;
#18642 = CARTESIAN_POINT ( 'NONE',  ( -96.43155670463150386, -293.1599954154496572, -224.7515174997466829 ) ) ;
#18643 = DIRECTION ( 'NONE',  ( -1.000000000000000000, -0.000000000000000000, -0.000000000000000000 ) ) ;
#18644 = CARTESIAN_POINT ( 'NONE',  ( 25.18497378105907814, -295.4090924074130839, -220.4570493818173702 ) ) ;
#18645 = ORIENTED_EDGE ( 'NONE', *, *, #24497, .F. ) ;
#18646 = CARTESIAN_POINT ( 'NONE',  ( 28.91473217082226554, -274.0232732294889502, -305.9690302599933034 ) ) ;
#18647 = DIRECTION ( 'NONE',  ( 0.000000000000000000, 0.000000000000000000, -1.000000000000000000 ) ) ;
#18648 = CARTESIAN_POINT ( 'NONE',  ( -39.10991420598376322, -293.4738731897464277, -346.5406023381209479 ) ) ;
#18649 = CARTESIAN_POINT ( 'NONE',  ( -40.51437295184805265, -297.5188686772299320, -197.3559385014798977 ) ) ;
#18650 = AXIS2_PLACEMENT_3D ( 'NONE', #61297, #39934, #10600 ) ;
#18651 = CARTESIAN_POINT ( 'NONE',  ( 32.05879219835336613, -289.3991662531844895, -295.1457788952432111 ) ) ;
#18652 = CARTESIAN_POINT ( 'NONE',  ( 31.28234780054427944, -283.6784855533242649, -298.0868110734988363 ) ) ;
#18653 = CARTESIAN_POINT ( 'NONE',  ( -109.8773459360917997, -292.2840325697873709, -246.1707123410854763 ) ) ;
#18654 = CARTESIAN_POINT ( 'NONE',  ( -47.69335392109125138, -293.2384739100841671, -194.5043583501977764 ) ) ;
#18655 = CARTESIAN_POINT ( 'NONE',  ( -64.06963382229783122, -291.5268855571030144, -202.4166086296711740 ) ) ;
#18656 = CARTESIAN_POINT ( 'NONE',  ( -99.01468426797714528, -287.1312837319169375, -227.6600314654222927 ) ) ;
#18657 = CARTESIAN_POINT ( 'NONE',  ( -68.67446841571224070, -279.8182932477030818, -200.0099874910655444 ) ) ;
#18658 = CARTESIAN_POINT ( 'NONE',  ( -109.8407719097109521, -294.3593574740602890, -291.6952726328509016 ) ) ;
#18659 = CARTESIAN_POINT ( 'NONE',  ( -71.74064495157217891, -283.3275090847915294, -339.2502506492066914 ) ) ;
#18660 = CIRCLE ( 'NONE', #71609, 1.000000000000000888 ) ;
#18661 = CARTESIAN_POINT ( 'NONE',  ( 35.83938354246152613, -277.2498857938909964, -257.8200225499571161 ) ) ;
#18662 = CARTESIAN_POINT ( 'NONE',  ( -21.39648532958013050, -282.7662352645559167, -200.3538533559491555 ) ) ;
#18663 = CARTESIAN_POINT ( 'NONE',  ( -38.54941638853789954, -275.2067345497992505, -346.1162953996163765 ) ) ;
#18664 = DIRECTION ( 'NONE',  ( 0.000000000000000000, -1.000000000000000000, 0.000000000000000000 ) ) ;
#18665 = CARTESIAN_POINT ( 'NONE',  ( 5.623224251494886694, -281.9598166007838245, -329.4542962228417196 ) ) ;
#18666 = AXIS2_PLACEMENT_3D ( 'NONE', #60916, #53801, #89762 ) ;
#18667 = CARTESIAN_POINT ( 'NONE',  ( -101.5667326911130175, -280.3094560961239949, -228.5140120107250254 ) ) ;
#18668 = CARTESIAN_POINT ( 'NONE',  ( 34.84709516768052140, -286.9433776802270586, -296.6231371575196931 ) ) ;
#18669 = CARTESIAN_POINT ( 'NONE',  ( 34.62793203682779364, -295.0868981206335206, -253.0343474516622564 ) ) ;
#18670 = CARTESIAN_POINT ( 'NONE',  ( 37.40168358230796741, -277.3396654041292209, -285.1890311517540795 ) ) ;
#18671 = CARTESIAN_POINT ( 'NONE',  ( 37.70194245288274004, -277.0547571151574289, -285.2523900011760247 ) ) ;
#18672 = CARTESIAN_POINT ( 'NONE',  ( -8.740633481064914889, -276.5005435795611106, -337.5384822809604657 ) ) ;
#18673 = CARTESIAN_POINT ( 'NONE',  ( -96.20001071998778741, -297.9165606053701936, -316.5750520847586245 ) ) ;
#18674 = CARTESIAN_POINT ( 'NONE',  ( -99.61902232865598705, -283.1138997044207031, -228.8693890952451397 ) ) ;
#18675 = CARTESIAN_POINT ( 'NONE',  ( -19.38758490519804312, -291.9436003450615544, -195.4504883300527638 ) ) ;
#18676 = CARTESIAN_POINT ( 'NONE',  ( -15.16539300411809776, -290.3699287529752837, -343.3179531839842298 ) ) ;
#18677 = AXIS2_PLACEMENT_3D ( 'NONE', #58278, #92351, #27995 ) ;
#18678 = ADVANCED_FACE ( 'NONE', ( #85253 ), #15471, .F. ) ;
#18679 = CARTESIAN_POINT ( 'NONE',  ( 6.873573640867734369, -291.5905150399097465, -211.8868874343441178 ) ) ;
#18680 = ORIENTED_EDGE ( 'NONE', *, *, #32302, .T. ) ;
#18681 = CARTESIAN_POINT ( 'NONE',  ( -88.24335383574977243, -289.9302719649409710, -213.3731548560725173 ) ) ;
#18682 = CARTESIAN_POINT ( 'NONE',  ( -60.26157742424427965, -291.4135099391671702, -200.9772142064452396 ) ) ;
#18683 = ORIENTED_EDGE ( 'NONE', *, *, #91573, .F. ) ;
#18684 = CARTESIAN_POINT ( 'NONE',  ( -70.49295314886026631, -290.5585967235142562, -339.5310717999277585 ) ) ;
#18685 = CARTESIAN_POINT ( 'NONE',  ( -103.3907855263951490, -279.3074695478624676, -239.1037614368844686 ) ) ;
#18686 = EDGE_CURVE ( 'NONE', #56456, #53974, #17316, .T. ) ;
#18687 = CARTESIAN_POINT ( 'NONE',  ( -110.9227162735125916, -295.1997044258587266, -292.0252043671100637 ) ) ;
#18688 = CARTESIAN_POINT ( 'NONE',  ( -36.57479149920327899, -286.7129501317197651, -193.4538532475847603 ) ) ;
#18689 = CARTESIAN_POINT ( 'NONE',  ( 38.08841996104084870, -288.0776278303706022, -285.7247528051314589 ) ) ;
#18690 = CARTESIAN_POINT ( 'NONE',  ( -110.4115472345471574, -284.8781483011757132, -270.9136937307862354 ) ) ;
#18691 = CARTESIAN_POINT ( 'NONE',  ( -104.5909623734863345, -255.9058999860209269, -326.6256074632946707 ) ) ;
#18692 = CARTESIAN_POINT ( 'NONE',  ( 4.381996518072155844, -57.88619191719195101, -353.6676151370956518 ) ) ;
#18693 = CARTESIAN_POINT ( 'NONE',  ( -63.40552176226377412, -182.3960580802271920, -358.6459566522576097 ) ) ;
#18694 = CARTESIAN_POINT ( 'NONE',  ( 30.32806307829934767, -274.3758262439469604, -242.4178872203009689 ) ) ;
#18695 = CARTESIAN_POINT ( 'NONE',  ( -35.12199346387371435, -275.9439523763949182, -343.6366185044350914 ) ) ;
#18696 = CARTESIAN_POINT ( 'NONE',  ( -114.0589307625553630, -296.1410589333410712, -263.8694035640912148 ) ) ;
#18697 = CARTESIAN_POINT ( 'NONE',  ( 122.5836672862912309, 147.2107594463095381, -260.7345742909203636 ) ) ;
#18698 = CARTESIAN_POINT ( 'NONE',  ( 16.59559936688325621, -274.9897309909188721, -324.6943247859525172 ) ) ;
#18699 = CARTESIAN_POINT ( 'NONE',  ( -63.68810199495433721, -275.4641019763753320, -201.1821179894019451 ) ) ;
#18700 = CARTESIAN_POINT ( 'NONE',  ( -26.26400523166820022, -299.1289105048854253, -193.5946887281719455 ) ) ;
#18701 = CARTESIAN_POINT ( 'NONE',  ( -42.66214133136008968, -289.6132901962125175, -343.2793248315861661 ) ) ;
#18702 = CARTESIAN_POINT ( 'NONE',  ( -86.28458531810886711, -296.5145445294927526, -329.5958443622394043 ) ) ;
#18703 = CARTESIAN_POINT ( 'NONE',  ( -98.18916324516062843, -297.6738231037157334, -223.2536223037349146 ) ) ;
#18704 = CARTESIAN_POINT ( 'NONE',  ( -73.30055592941759812, -295.7100381190964526, -333.8903293264039576 ) ) ;
#18705 = EDGE_LOOP ( 'NONE', ( #38783, #28105, #56712, #32557 ) ) ;
#18706 = CIRCLE ( 'NONE', #30804, 35.00000000000002842 ) ;
#18707 = CARTESIAN_POINT ( 'NONE',  ( -28.74021323455523813, -278.8641874720310625, -345.4825186157805774 ) ) ;
#18708 = EDGE_LOOP ( 'NONE', ( #40335, #8615, #61420, #89935 ) ) ;
#18709 = CARTESIAN_POINT ( 'NONE',  ( 1.348456666218617261, -280.0618252109069317, -203.7978372947814307 ) ) ;
#18710 = CIRCLE ( 'NONE', #71658, 7.910944475430059519 ) ;
#18711 = CARTESIAN_POINT ( 'NONE',  ( 3.274527898685858140, -277.4326124039857291, -331.3015025282545025 ) ) ;
#18712 = CARTESIAN_POINT ( 'NONE',  ( -45.51800456970485698, -278.9144098953296975, -345.9589743188711850 ) ) ;
#18713 = CARTESIAN_POINT ( 'NONE',  ( -110.5826439677304194, -276.3450621847935054, -288.1401053648218635 ) ) ;
#18714 = CARTESIAN_POINT ( 'NONE',  ( -109.9476206690420526, -273.1518800605063007, -262.2144165637978972 ) ) ;
#18715 = CARTESIAN_POINT ( 'NONE',  ( -93.17974848793016918, -295.8039727188680104, -222.4096305120141039 ) ) ;
#18716 = FACE_OUTER_BOUND ( 'NONE', #67744, .T. ) ;
#18717 = CARTESIAN_POINT ( 'NONE',  ( -104.2705400919363399, -278.3254169924786652, -299.6344783160370184 ) ) ;
#18718 = CIRCLE ( 'NONE', #30825, 1.500000000000003997 ) ;
#18719 = CARTESIAN_POINT ( 'NONE',  ( -3.295332338453454746, -287.2968809615135797, -338.8894685324717670 ) ) ;
#18720 = CARTESIAN_POINT ( 'NONE',  ( -93.60348516543066921, -275.2416943134270468, -220.7666405177664330 ) ) ;
#18721 = FACE_BOUND ( 'NONE', #88914, .T. ) ;
#18722 = CIRCLE ( 'NONE', #83730, 4.000000000000003553 ) ;
#18723 = CARTESIAN_POINT ( 'NONE',  ( -109.0991129620712030, -289.5607162052871217, -284.6897228256451058 ) ) ;
#18724 = VECTOR ( 'NONE', #42905, 1000.000000000000000 ) ;
#18725 = CARTESIAN_POINT ( 'NONE',  ( -96.19765763992201357, -283.2332725913774425, -319.8717871418928098 ) ) ;
#18726 = CARTESIAN_POINT ( 'NONE',  ( 29.05028276768653228, -280.2306043492196750, -303.1894127679742610 ) ) ;
#18728 = CARTESIAN_POINT ( 'NONE',  ( -44.13185445101422744, -284.0454626924659465, -196.2314477962858064 ) ) ;
#18727 = CARTESIAN_POINT ( 'NONE',  ( 17.51406107999513395, -279.4307402858245837, -221.3078777209174746 ) ) ;
#18729 = CARTESIAN_POINT ( 'NONE',  ( 32.54108383381068137, -289.1964505211116716, -242.9922279296531258 ) ) ;
#18730 = CARTESIAN_POINT ( 'NONE',  ( -98.33207288189734641, -280.3223544212774527, -229.4381993958763815 ) ) ;
#18731 = FACE_BOUND ( 'NONE', #71920, .T. ) ;
#18732 = CARTESIAN_POINT ( 'NONE',  ( -11.85742624963008218, -294.3839197310990698, -199.7689481161864364 ) ) ;
#18734 = CARTESIAN_POINT ( 'NONE',  ( -69.51268503985730263, -277.8744631738266548, -201.5065117220206048 ) ) ;
#18733 = AXIS2_PLACEMENT_3D ( 'NONE', #32125, #54819, #77077 ) ;
#18735 = CARTESIAN_POINT ( 'NONE',  ( -68.07273214200738209, -278.1180596106455027, -336.7035830925050846 ) ) ;
#18736 = CARTESIAN_POINT ( 'NONE',  ( -93.93716410975736153, -285.8669174671474025, -319.8280957088907144 ) ) ;
#18737 = EDGE_CURVE ( 'NONE', #69962, #62086, #26483, .T. ) ;
#18738 = EDGE_CURVE ( 'NONE', #79497, #45087, #4868, .T. ) ;
#18739 = CARTESIAN_POINT ( 'NONE',  ( 197.2081551558208048, 68.08088840871901937, 10.51999689724803311 ) ) ;
#18740 = CARTESIAN_POINT ( 'NONE',  ( -99.48216543947647494, -291.8937510049568118, -313.3480551792785036 ) ) ;
#18741 = CARTESIAN_POINT ( 'NONE',  ( -99.21249642911720912, -293.9774479272222152, -312.7747351184175955 ) ) ;
#18742 = AXIS2_PLACEMENT_3D ( 'NONE', #93644, #28342, #57232 ) ;
#18743 = CARTESIAN_POINT ( 'NONE',  ( -1.036807435070341565, -285.7187413196473358, -202.6402675199855139 ) ) ;
#18744 = CARTESIAN_POINT ( 'NONE',  ( -108.8789730053623828, -289.1893774704858515, -252.1753094629680163 ) ) ;
#18745 = CARTESIAN_POINT ( 'NONE',  ( 152.4536156746142410, 276.0000000000000568, -14.50000000000000000 ) ) ;
#18746 = CARTESIAN_POINT ( 'NONE',  ( 36.08060790628862691, -274.1814927167730502, -266.1271425914335396 ) ) ;
#18747 = CARTESIAN_POINT ( 'NONE',  ( 20.64398495721016502, -292.3358468826331773, -316.7335665964382088 ) ) ;
#18748 = CARTESIAN_POINT ( 'NONE',  ( 202.9737475146022803, 296.4636489462809550, -68.70538243550777224 ) ) ;
#18749 = DIRECTION ( 'NONE',  ( 0.7957555401921962979, 0.6056179655966504871, 0.000000000000000000 ) ) ;
#18750 = CARTESIAN_POINT ( 'NONE',  ( -53.22592131223413503, -290.3320553694580326, -195.6720060197304747 ) ) ;
#18751 = CARTESIAN_POINT ( 'NONE',  ( -93.88098580630865797, -286.8185093421110423, -222.9295926848291742 ) ) ;
#18752 = CARTESIAN_POINT ( 'NONE',  ( 28.02053394467954206, -286.3036576663770347, -309.1135678290094688 ) ) ;
#18753 = CARTESIAN_POINT ( 'NONE',  ( -100.1214030483830584, -286.5033629326264872, -231.8701936466242728 ) ) ;
#18754 = CARTESIAN_POINT ( 'NONE',  ( 186.6539576904058890, 276.0000000000000568, -11.60392986742922439 ) ) ;
#18755 = CARTESIAN_POINT ( 'NONE',  ( -17.13707143614291439, -287.1224446259592469, -199.9919077277388908 ) ) ;
#18756 = CARTESIAN_POINT ( 'NONE',  ( 21.80111255894472677, -294.8935796563231406, -223.6443142798336794 ) ) ;
#18757 = CARTESIAN_POINT ( 'NONE',  ( -111.3874922928703199, -276.4393645415207743, -285.4762350049023212 ) ) ;
#18758 = CARTESIAN_POINT ( 'NONE',  ( 23.50394265873821809, -276.5154624084473198, -317.5370524052583505 ) ) ;
#18759 = CARTESIAN_POINT ( 'NONE',  ( -44.73141521653276698, -290.0392999602618147, -195.1114043686207538 ) ) ;
#18760 = CARTESIAN_POINT ( 'NONE',  ( -101.8912199224298121, -279.1045746747556109, -228.2841715781802918 ) ) ;
#18761 = CARTESIAN_POINT ( 'NONE',  ( -101.5691566137259372, -298.0197120064832461, -308.4980914793898705 ) ) ;
#18762 = CARTESIAN_POINT ( 'NONE',  ( -48.18343439339133027, -253.8127106430984554, -479.5013660720755979 ) ) ;
#18763 = LINE ( 'NONE', #55220, #11818 ) ;
#18764 = CARTESIAN_POINT ( 'NONE',  ( -22.34293603469879130, -284.9329319644132852, -198.3625115006764759 ) ) ;
#18765 = CARTESIAN_POINT ( 'NONE',  ( -111.1345464317928560, -276.5808475524162304, -278.9089071990499633 ) ) ;
#18766 = CARTESIAN_POINT ( 'NONE',  ( 37.70923014681355312, -279.5469251451431774, -269.9668807185926198 ) ) ;
#18767 = DIRECTION ( 'NONE',  ( 0.000000000000000000, 0.000000000000000000, -1.000000000000000000 ) ) ;
#18768 = CARTESIAN_POINT ( 'NONE',  ( -5.386818766784664092, -272.9448910365494498, -201.0675878931002956 ) ) ;
#18769 = CARTESIAN_POINT ( 'NONE',  ( 34.12312648197760723, -295.3074112094442398, -288.3468432064793205 ) ) ;
#18770 = CARTESIAN_POINT ( 'NONE',  ( -22.61202491430037398, -279.1566409615292628, -195.0440122638999583 ) ) ;
#18771 = CARTESIAN_POINT ( 'NONE',  ( -67.38079478197782635, -296.3973111853301248, -337.1660434018394881 ) ) ;
#18772 = CARTESIAN_POINT ( 'NONE',  ( -112.7150780685094418, -297.6984083220048092, -283.7807934834755201 ) ) ;
#18773 = CARTESIAN_POINT ( 'NONE',  ( -105.4344203833179989, -272.5728162133851811, -243.8499151147408952 ) ) ;
#18774 = CARTESIAN_POINT ( 'NONE',  ( -32.04067039278705664, -294.1191701816941304, -195.5357215786828533 ) ) ;
#18775 = CARTESIAN_POINT ( 'NONE',  ( -105.4330856520122666, -285.1843091593478903, -234.2947129231015140 ) ) ;
#18776 = CARTESIAN_POINT ( 'NONE',  ( 14.02801243071343507, -274.4803023513711082, -326.1232382290839382 ) ) ;
#18777 = CARTESIAN_POINT ( 'NONE',  ( -14.95427692247031715, -288.6034048032812507, -344.0904954832176372 ) ) ;
#18778 = CARTESIAN_POINT ( 'NONE',  ( 19.68919536766276579, -287.2584060330154330, -316.3054909557052952 ) ) ;
#18779 = CARTESIAN_POINT ( 'NONE',  ( -47.44800378367437332, -289.9236734078226618, -195.9927533761947416 ) ) ;
#18780 = ORIENTED_EDGE ( 'NONE', *, *, #34635, .T. ) ;
#18781 = CARTESIAN_POINT ( 'NONE',  ( -96.12512592106646991, -239.9971452530988358, -342.0757611934672582 ) ) ;
#18782 = CIRCLE ( 'NONE', #62674, 24.00000000000000355 ) ;
#18783 = CARTESIAN_POINT ( 'NONE',  ( -50.76892163754745013, -288.7358408542963275, -342.2299572942357599 ) ) ;
#18784 = DIRECTION ( 'NONE',  ( 0.000000000000000000, 1.000000000000000000, 0.000000000000000000 ) ) ;
#18785 = CARTESIAN_POINT ( 'NONE',  ( -106.7876728478178592, -285.0730976505982994, -303.0731507119510866 ) ) ;
#18786 = CARTESIAN_POINT ( 'NONE',  ( 21.13900441459611557, -291.9382306270628646, -220.6135005519547860 ) ) ;
#18787 = CARTESIAN_POINT ( 'NONE',  ( -35.37728931260219412, -281.6765127216661995, -194.1734398434828393 ) ) ;
#18788 = CARTESIAN_POINT ( 'NONE',  ( 12.65715879840846192, -282.0477568243366591, -212.4524625194193277 ) ) ;
#18789 = CARTESIAN_POINT ( 'NONE',  ( -91.66646550385388537, -283.6873924885454699, -319.1428224308774588 ) ) ;
#18790 = CARTESIAN_POINT ( 'NONE',  ( -7.931557987147630051, -278.6670339991420633, -339.3681074497190480 ) ) ;
#18791 = CARTESIAN_POINT ( 'NONE',  ( -103.1155859552882106, -296.0293825643942682, -310.3960520175944566 ) ) ;
#18792 = VECTOR ( 'NONE', #53442, 1000.000000000000000 ) ;
#18793 = CARTESIAN_POINT ( 'NONE',  ( -91.94556639466898673, -289.2881740036900737, -219.4475847320395303 ) ) ;
#18794 = CARTESIAN_POINT ( 'NONE',  ( -85.55952679142329487, -272.1628310167454288, -214.9564980983543308 ) ) ;
#18795 = ORIENTED_EDGE ( 'NONE', *, *, #68972, .F. ) ;
#18796 = ORIENTED_EDGE ( 'NONE', *, *, #92268, .T. ) ;
#18797 = CARTESIAN_POINT ( 'NONE',  ( 29.33919985515026596, -232.1443419142230766, 25.50000000000000000 ) ) ;
#18798 = CARTESIAN_POINT ( 'NONE',  ( -111.6676273700015969, -286.5365823340550264, -265.3929911944862283 ) ) ;
#18799 = CARTESIAN_POINT ( 'NONE',  ( 33.13794856051175941, -295.0199738230660955, -300.7295683472426617 ) ) ;
#18800 = CIRCLE ( 'NONE', #70256, 1.000000000000000888 ) ;
#18801 = CARTESIAN_POINT ( 'NONE',  ( -34.83474700214905084, -283.6712813188154314, -343.4325059376524223 ) ) ;
#18802 = CARTESIAN_POINT ( 'NONE',  ( -5.393661690203832570, -275.7007345470771611, -340.1618561865695938 ) ) ;
#18803 = CARTESIAN_POINT ( 'NONE',  ( -111.1366832903113533, -291.4751518976114539, -248.7367510143157858 ) ) ;
#18804 = CARTESIAN_POINT ( 'NONE',  ( -104.3287467996063498, -283.1575394208524585, -234.8505318502745354 ) ) ;
#18805 = CARTESIAN_POINT ( 'NONE',  ( -79.58636089973413164, -291.8318217577649989, -205.9457621981620719 ) ) ;
#18806 = CARTESIAN_POINT ( 'NONE',  ( -29.16654210983734785, -289.2789784196760934, -342.9231898805035144 ) ) ;
#18807 = CARTESIAN_POINT ( 'NONE',  ( 219.8344101925596021, 35.72494958537217968, 9.000000000000001776 ) ) ;
#18808 = AXIS2_PLACEMENT_3D ( 'NONE', #18963, #61589, #63480 ) ;
#18809 = DIRECTION ( 'NONE',  ( -0.000000000000000000, -1.000000000000000000, -0.000000000000000000 ) ) ;
#18810 = CARTESIAN_POINT ( 'NONE',  ( -107.3854158231707459, -264.5521555645648846, -305.4145383826947295 ) ) ;
#18811 = CARTESIAN_POINT ( 'NONE',  ( -60.99817021723886512, -284.8737349944302082, -342.9633780162285461 ) ) ;
#18812 = CARTESIAN_POINT ( 'NONE',  ( -4.771743288812454686, -283.9809262143061233, -202.8022627189028810 ) ) ;
#18813 = ORIENTED_EDGE ( 'NONE', *, *, #92502, .T. ) ;
#18814 = CARTESIAN_POINT ( 'NONE',  ( 31.36480513695133610, -280.1311898739672301, -244.6489803408817636 ) ) ;
#18815 = CARTESIAN_POINT ( 'NONE',  ( 36.04119379637801046, -275.5112173964161002, -293.6139709427035314 ) ) ;
#18816 = CARTESIAN_POINT ( 'NONE',  ( -70.57688936365295262, -281.6130930180749488, -203.2988001691300326 ) ) ;
#18817 = CARTESIAN_POINT ( 'NONE',  ( 47.02842677011826567, 10.69185302179798214, -329.9758182323871551 ) ) ;
#18818 = CARTESIAN_POINT ( 'NONE',  ( 39.05232701943413076, -280.0857914278421958, -267.1007619881191317 ) ) ;
#18819 = CARTESIAN_POINT ( 'NONE',  ( -103.6890943860418588, -283.0270031874921415, -236.1577544805183209 ) ) ;
#18820 = CARTESIAN_POINT ( 'NONE',  ( -26.41416471961995072, -299.9473087259986528, -194.3712223735663542 ) ) ;
#18821 = CIRCLE ( 'NONE', #12748, 8.222204860432958284 ) ;
#18822 = CARTESIAN_POINT ( 'NONE',  ( -42.38772121344757693, -295.6098550707359891, -343.2481958011119900 ) ) ;
#18824 = ORIENTED_EDGE ( 'NONE', *, *, #90373, .F. ) ;
#18823 = EDGE_CURVE ( 'NONE', #64042, #13568, #12443, .T. ) ;
#18825 = CARTESIAN_POINT ( 'NONE',  ( -34.82372468284911093, -290.7692668114616481, -196.9111126810951191 ) ) ;
#18826 = CARTESIAN_POINT ( 'NONE',  ( -14.61189703666436657, -277.4166366283656089, -343.8788947095050048 ) ) ;
#18827 = CARTESIAN_POINT ( 'NONE',  ( 35.69883683584532008, -275.5682967614529844, -271.5849663936369325 ) ) ;
#18828 = CARTESIAN_POINT ( 'NONE',  ( 1.052625872994708667, -273.4723967524362820, -203.9578800592401819 ) ) ;
#18829 = CARTESIAN_POINT ( 'NONE',  ( -74.94434090351494149, -285.8906705383787994, 25.50000000000000000 ) ) ;
#18830 = CARTESIAN_POINT ( 'NONE',  ( -111.1113389439735215, -270.7292401098747519, -256.5566746695058100 ) ) ;
#18831 = CARTESIAN_POINT ( 'NONE',  ( -47.80257052418233599, -229.5268262511776527, 22.47499999999998721 ) ) ;
#18832 = CARTESIAN_POINT ( 'NONE',  ( -43.18343439339132317, -283.1093320178187582, -507.6442049081570076 ) ) ;
#18833 = CARTESIAN_POINT ( 'NONE',  ( 28.43447001966500665, -283.0699600556689006, -302.8448902439720314 ) ) ;
#18834 = CARTESIAN_POINT ( 'NONE',  ( 38.27215002563985280, -283.4140294380544560, -278.3888974233419162 ) ) ;
#18835 = CARTESIAN_POINT ( 'NONE',  ( -109.7119693298962204, -284.0366421004114841, -260.0442965786539276 ) ) ;
#18836 = CARTESIAN_POINT ( 'NONE',  ( -16.17065397512084957, -275.1738379208329093, -341.1128447602646929 ) ) ;
#18837 = CARTESIAN_POINT ( 'NONE',  ( 14.80900492802579116, -284.1686893440596009, -323.2650374949166689 ) ) ;
#18838 = CARTESIAN_POINT ( 'NONE',  ( -56.80172443905418334, -275.7873937937401934, -341.4916484449256586 ) ) ;
#18839 = LINE ( 'NONE', #84608, #74473 ) ;
#18840 = CARTESIAN_POINT ( 'NONE',  ( 33.54459041757150572, -276.8775938307750266, -289.0522893488450222 ) ) ;
#18841 = CARTESIAN_POINT ( 'NONE',  ( 195.6084660501286692, 42.25382305297375041, 12.67848964989311611 ) ) ;
#18842 = CARTESIAN_POINT ( 'NONE',  ( -33.93268722918507052, -280.8968451076613633, -193.5982529248710478 ) ) ;
#18843 = EDGE_LOOP ( 'NONE', ( #20360, #26128, #11665, #73887 ) ) ;
#18844 = DIRECTION ( 'NONE',  ( -0.000000000000000000, -0.000000000000000000, 1.000000000000000000 ) ) ;
#18845 = CARTESIAN_POINT ( 'NONE',  ( -75.50535936348644839, -287.4096260397911351, -204.8496377679980185 ) ) ;
#18846 = CARTESIAN_POINT ( 'NONE',  ( -96.54509013646611493, -295.1488627145922692, -313.3657614661292996 ) ) ;
#18847 = CARTESIAN_POINT ( 'NONE',  ( -112.4675391785426513, -289.6951900939840243, -286.7751697093871144 ) ) ;
#18848 = CARTESIAN_POINT ( 'NONE',  ( 17.65845366658705018, -285.0924184874581897, -220.8148535762663016 ) ) ;
#18850 = CARTESIAN_POINT ( 'NONE',  ( -65.69470122671074819, -289.9160471312525260, -201.9801649349061847 ) ) ;
#18849 = CARTESIAN_POINT ( 'NONE',  ( -10.51842168073719996, -284.9837870934871944, -201.8209416347469300 ) ) ;
#18851 = CARTESIAN_POINT ( 'NONE',  ( -104.9693623747481155, -286.1395522297913203, -241.7062207245768093 ) ) ;
#18852 = CARTESIAN_POINT ( 'NONE',  ( 35.63964157812512212, -273.7745680289260690, -287.7000002103532097 ) ) ;
#18853 = CARTESIAN_POINT ( 'NONE',  ( -51.99922893755491060, -284.2675810868524309, -195.5303123219319446 ) ) ;
#18854 = CARTESIAN_POINT ( 'NONE',  ( -37.28144809524221159, -300.0530651647117679, -195.3603449120130335 ) ) ;
#18855 = CARTESIAN_POINT ( 'NONE',  ( 36.97687297005811047, -285.4066402836695602, -259.0156515848358367 ) ) ;
#18856 = CARTESIAN_POINT ( 'NONE',  ( -1.862551923666285747, -281.4757557258479324, -206.2936653162772132 ) ) ;
#18857 = CARTESIAN_POINT ( 'NONE',  ( -71.06067032536718386, -291.4962940531041227, -337.5404263991663925 ) ) ;
#18858 = CARTESIAN_POINT ( 'NONE',  ( 189.9243309297870610, 276.0000000000000568, 20.22542485937349355 ) ) ;
#18859 = EDGE_CURVE ( 'NONE', #34447, #8082, #86565, .T. ) ;
#18860 = CARTESIAN_POINT ( 'NONE',  ( 196.2494062209129027, 40.89692782860188913, 13.06344435505938861 ) ) ;
#18861 = CARTESIAN_POINT ( 'NONE',  ( -104.6633888595714410, -298.0207288525874105, -304.7852571985416148 ) ) ;
#18862 = CARTESIAN_POINT ( 'NONE',  ( -60.32288788999900930, -277.7541595749368071, -198.9140230212935307 ) ) ;
#18863 = CARTESIAN_POINT ( 'NONE',  ( -73.34897678022525724, -290.7841774309087555, -202.4666890109656379 ) ) ;
#18864 = CARTESIAN_POINT ( 'NONE',  ( -73.21815732447144853, -295.9678506135770135, -205.8683258656144233 ) ) ;
#18865 = CARTESIAN_POINT ( 'NONE',  ( 30.78544833183558183, -280.6036654770975360, -297.9280387326817845 ) ) ;
#18866 = CARTESIAN_POINT ( 'NONE',  ( 21.84098360022365171, -273.0091043858556077, -225.1878949879414051 ) ) ;
#18867 = CARTESIAN_POINT ( 'NONE',  ( 20.56114944821640833, -294.2333855278292845, -225.0803533602745858 ) ) ;
#18868 = CARTESIAN_POINT ( 'NONE',  ( -85.28047601435906699, -298.1948066931273615, -330.5268031993605859 ) ) ;
#18869 = CARTESIAN_POINT ( 'NONE',  ( -54.42098962299014175, -296.3164577819803753, -195.9903870379907005 ) ) ;
#18870 = CARTESIAN_POINT ( 'NONE',  ( 38.48921935921545412, -291.8633059406286065, -275.9867490454769268 ) ) ;
#18871 = VECTOR ( 'NONE', #8555, 1000.000000000000000 ) ;
#18872 = CARTESIAN_POINT ( 'NONE',  ( -105.6533031316659503, -291.6124610939351669, -297.8638286415605307 ) ) ;
#18873 = CARTESIAN_POINT ( 'NONE',  ( 195.7510731661265595, -164.3527196417747405, -21.50000000000000000 ) ) ;
#18874 = CARTESIAN_POINT ( 'NONE',  ( -69.09691759994316840, -292.4263627289237775, -204.4366782582059159 ) ) ;
#18875 = CARTESIAN_POINT ( 'NONE',  ( 184.7149167944524493, -12.49482340714361506, 9.974999999999996092 ) ) ;
#18877 = CARTESIAN_POINT ( 'NONE',  ( -14.84640119613110087, -292.3518903259908939, -200.9135728426330445 ) ) ;
#18876 = CARTESIAN_POINT ( 'NONE',  ( -101.5304992912097788, -282.0451015658453571, -309.8352216879276853 ) ) ;
#18878 = CARTESIAN_POINT ( 'NONE',  ( 39.52916933180058834, -281.6184332394641956, -275.6608986983745808 ) ) ;
#18879 = CARTESIAN_POINT ( 'NONE',  ( -81.55288412240864204, -283.3021188180685499, -333.4427560718260111 ) ) ;
#18880 = CIRCLE ( 'NONE', #91651, 24.50000000000000355 ) ;
#18881 = CARTESIAN_POINT ( 'NONE',  ( -70.81484320899905072, -287.4945361477072652, -337.3049711775195192 ) ) ;
#18882 = CARTESIAN_POINT ( 'NONE',  ( -1.444335248645383984, -278.9992547610586939, -203.0254888646603320 ) ) ;
#18883 = TOROIDAL_SURFACE ( 'NONE', #71832, 24.49999999999999645, 0.5000000000000000000 ) ;
#18884 = CARTESIAN_POINT ( 'NONE',  ( 18.41062218692302110, -287.1945738057424933, -323.0220244139024430 ) ) ;
#18885 = CARTESIAN_POINT ( 'NONE',  ( 195.2312239546291437, 39.36132622696000283, 15.00000000000000000 ) ) ;
#18886 = CARTESIAN_POINT ( 'NONE',  ( 34.42095219661052141, -294.9269111771769190, -253.0862142663106624 ) ) ;
#18887 = CARTESIAN_POINT ( 'NONE',  ( 35.50640090569080343, -277.2694871423444170, -293.4210500843008163 ) ) ;
#18888 = CARTESIAN_POINT ( 'NONE',  ( -93.10359974968768881, -278.8888814517983405, -223.1963870265717560 ) ) ;
#18889 = CARTESIAN_POINT ( 'NONE',  ( 6.494488533721804124, -292.7966951989048994, -207.0571799684375378 ) ) ;
#18890 = CARTESIAN_POINT ( 'NONE',  ( -64.75302457340447404, -281.4871486737209807, -340.7876528721564000 ) ) ;
#18891 = CARTESIAN_POINT ( 'NONE',  ( 15.05219701163399826, -291.8722858071603810, -219.1192616871452685 ) ) ;
#18892 = CARTESIAN_POINT ( 'NONE',  ( -111.6740538544493830, -294.4188869389090542, -280.7275134834287087 ) ) ;
#18893 = ORIENTED_EDGE ( 'NONE', *, *, #58679, .T. ) ;
#18894 = DIRECTION ( 'NONE',  ( 0.6056179655966488218, -0.7957555401921976301, 0.000000000000000000 ) ) ;
#18895 = CARTESIAN_POINT ( 'NONE',  ( 27.20950507223730241, -293.5268924276162466, -304.6909914870873308 ) ) ;
#18896 = DIRECTION ( 'NONE',  ( 1.000000000000000000, -0.000000000000000000, -0.000000000000000000 ) ) ;
#18897 = CARTESIAN_POINT ( 'NONE',  ( -102.0455923789670294, -293.6237833571632905, -301.4846348637937581 ) ) ;
#18898 = CARTESIAN_POINT ( 'NONE',  ( -99.43051780650718285, -272.3524075826391027, -225.0055052814526846 ) ) ;
#18899 = CARTESIAN_POINT ( 'NONE',  ( 5.505539833809690364, -278.7651994057787306, -207.8757636499558714 ) ) ;
#18900 = CARTESIAN_POINT ( 'NONE',  ( 30.97387595866132415, -288.4212507545352651, -235.9186974031164254 ) ) ;
#18901 = CARTESIAN_POINT ( 'NONE',  ( 27.02946414984780432, -287.8560809070183950, -304.8976562627448175 ) ) ;
#18902 = CARTESIAN_POINT ( 'NONE',  ( -37.79477499226169357, -278.5780155439665009, -344.0656325535945257 ) ) ;
#18903 = CARTESIAN_POINT ( 'NONE',  ( -108.4435728141672968, -294.2756057908904381, -293.2524164743741721 ) ) ;
#18904 = CARTESIAN_POINT ( 'NONE',  ( -100.7767048361804427, -298.8309245426736993, -232.1303878486236272 ) ) ;
#18905 = CARTESIAN_POINT ( 'NONE',  ( -110.0127458350879834, -277.4868049966538592, -259.7109375205692459 ) ) ;
#18906 = EDGE_LOOP ( 'NONE', ( #50128, #66337 ) ) ;
#18907 = CARTESIAN_POINT ( 'NONE',  ( -3.417821543773571946, -298.1327279901885277, -193.3841119163431586 ) ) ;
#18908 = CARTESIAN_POINT ( 'NONE',  ( -102.8999741921116424, -291.9994475966411756, -305.7325986753883171 ) ) ;
#18909 = CARTESIAN_POINT ( 'NONE',  ( 37.53530552031899958, -294.9736077720374965, -256.2234221980717166 ) ) ;
#18910 = DIRECTION ( 'NONE',  ( -1.000000000000000000, 0.000000000000000000, 0.000000000000000000 ) ) ;
#18911 = CARTESIAN_POINT ( 'NONE',  ( -96.84916500930633276, -291.7969625586382563, -227.8166296339977350 ) ) ;
#18912 = CYLINDRICAL_SURFACE ( 'NONE', #19457, 5.000000000000004441 ) ;
#18913 = CARTESIAN_POINT ( 'NONE',  ( -113.5019643645738796, -297.3378347527212782, -259.6390841796218751 ) ) ;
#18914 = CARTESIAN_POINT ( 'NONE',  ( -98.05378919152518336, -288.0786964853737686, -315.7074932839720418 ) ) ;
#18915 = CARTESIAN_POINT ( 'NONE',  ( -106.4961856110193850, -297.3197655250767752, -236.5468986506695899 ) ) ;
#18916 = CARTESIAN_POINT ( 'NONE',  ( 197.4878715644970555, 25.93102243561465414, 12.00000000000000000 ) ) ;
#18917 = DIRECTION ( 'NONE',  ( 1.000000000000000000, 0.000000000000000000, 0.000000000000000000 ) ) ;
#18918 = CARTESIAN_POINT ( 'NONE',  ( -29.03325661180904405, -290.4689228954406985, -346.2671623026141674 ) ) ;
#18919 = CARTESIAN_POINT ( 'NONE',  ( 25.18497378105907814, -283.4090924074130839, -220.4570493818173702 ) ) ;
#18920 = CARTESIAN_POINT ( 'NONE',  ( -73.27619907303937907, -287.5746980773051291, -204.7055472661805311 ) ) ;
#18921 = CARTESIAN_POINT ( 'NONE',  ( 35.29463020705783549, -285.8242574056594663, -246.4732252129328458 ) ) ;
#18922 = CARTESIAN_POINT ( 'NONE',  ( -66.50469390704590467, -271.6691758527842353, -201.4441518400082600 ) ) ;
#18923 = CARTESIAN_POINT ( 'NONE',  ( -38.12150358451864918, -275.9624588189304859, -195.9251985070002604 ) ) ;
#18924 = CARTESIAN_POINT ( 'NONE',  ( -102.3699398615240312, -289.1190763813115723, -234.0249009848026276 ) ) ;
#18925 = CARTESIAN_POINT ( 'NONE',  ( -111.5785046087205075, -280.2193230442732101, -285.5645670620446595 ) ) ;
#18926 = ORIENTED_EDGE ( 'NONE', *, *, #77324, .T. ) ;
#18928 = CARTESIAN_POINT ( 'NONE',  ( -6.719158214782700256, -279.8136768529938081, -203.9685962304837119 ) ) ;
#18927 = CARTESIAN_POINT ( 'NONE',  ( -14.30887690687654690, -280.3591643763424486, -201.0365515420852489 ) ) ;
#18929 = CARTESIAN_POINT ( 'NONE',  ( 14.68362212398608868, -277.4199162954646454, -326.7792892441633512 ) ) ;
#18930 = CARTESIAN_POINT ( 'NONE',  ( 25.96119380767855844, -279.7741671649436057, -227.1320995106458156 ) ) ;
#18931 = CARTESIAN_POINT ( 'NONE',  ( 101.5448465039121118, 115.7098217570894860, -280.1310368427940602 ) ) ;
#18932 = CARTESIAN_POINT ( 'NONE',  ( 25.94377920860218723, -275.9179540940089623, -226.8893685182977151 ) ) ;
#18933 = CARTESIAN_POINT ( 'NONE',  ( -97.28058710471766801, -274.7095762327166995, -223.1378442324793241 ) ) ;
#18934 = CARTESIAN_POINT ( 'NONE',  ( -4.829096099716510437, -294.9805209788416391, -202.7746430608542312 ) ) ;
#18935 = EDGE_LOOP ( 'NONE', ( #11356, #72469, #85648, #15340 ) ) ;
#18936 = LINE ( 'NONE', #82845, #65058 ) ;
#18937 = CARTESIAN_POINT ( 'NONE',  ( 13.34338273959105692, -287.8608674766525155, -217.3265000158627629 ) ) ;
#18938 = CARTESIAN_POINT ( 'NONE',  ( 11.77807641742177225, -290.1408466456891801, -328.3371609959373245 ) ) ;
#18939 = CARTESIAN_POINT ( 'NONE',  ( -108.2052430265821812, -290.1379391938208414, -252.3588819823835934 ) ) ;
#18940 = AXIS2_PLACEMENT_3D ( 'NONE', #90959, #40773, #33703 ) ;
#18941 = CARTESIAN_POINT ( 'NONE',  ( -35.14370753370436518, -285.5866794659120842, -193.4409260643512027 ) ) ;
#18942 = DIRECTION ( 'NONE',  ( -0.000000000000000000, -0.000000000000000000, -1.000000000000000000 ) ) ;
#18943 = CARTESIAN_POINT ( 'NONE',  ( -13.28766378687964789, -281.1344694934547306, -340.1852386514914315 ) ) ;
#18944 = CARTESIAN_POINT ( 'NONE',  ( 6.594435684013265409, -290.3085974241698182, -330.2623200973995381 ) ) ;
#18945 = CARTESIAN_POINT ( 'NONE',  ( -51.16677148893051452, -281.7118059978511155, -342.7980960525821388 ) ) ;
#18946 = CARTESIAN_POINT ( 'NONE',  ( -72.37946481064477666, -280.8933190962096660, -205.7577239161643945 ) ) ;
#18947 = CARTESIAN_POINT ( 'NONE',  ( 18.35939138315959340, -276.7161881296901242, -317.6408900450365422 ) ) ;
#18948 = CARTESIAN_POINT ( 'NONE',  ( -97.14390731579817384, -289.9916753979920259, -222.4893649737437329 ) ) ;
#18949 = CIRCLE ( 'NONE', #15914, 0.4999999999999922839 ) ;
#18950 = CARTESIAN_POINT ( 'NONE',  ( -100.8687674336618016, -285.9272585173221159, -227.0413013179723976 ) ) ;
#18951 = CARTESIAN_POINT ( 'NONE',  ( 12.03328035965071408, -287.2095133635745015, -211.2861942985843768 ) ) ;
#18952 = CARTESIAN_POINT ( 'NONE',  ( 33.45506089537422412, -281.4833226953147118, -252.5109377799178390 ) ) ;
#18953 = ORIENTED_EDGE ( 'NONE', *, *, #91976, .T. ) ;
#18954 = CARTESIAN_POINT ( 'NONE',  ( 157.7238125175271648, 18.72892514816273746, -11.10081581328746658 ) ) ;
#18955 = CARTESIAN_POINT ( 'NONE',  ( -105.3934700524614101, -291.9765227537372994, -303.7858825478775771 ) ) ;
#18956 = CARTESIAN_POINT ( 'NONE',  ( -69.40113288861358853, -290.3239040214406259, -200.8811149789876254 ) ) ;
#18957 = CARTESIAN_POINT ( 'NONE',  ( 22.47993516742575792, -274.0228657482211361, -228.0927434532131031 ) ) ;
#18958 = EDGE_CURVE ( 'NONE', #17649, #1470, #47369, .T. ) ;
#18959 = CARTESIAN_POINT ( 'NONE',  ( -108.2842166799565859, -295.5212885965420355, -300.1717196851911922 ) ) ;
#18960 = CARTESIAN_POINT ( 'NONE',  ( -63.02439339721960465, -290.1913948194979298, -201.2879175443906945 ) ) ;
#18961 = CARTESIAN_POINT ( 'NONE',  ( -71.41701075110785268, -293.7483828484737387, -336.0780167449001965 ) ) ;
#18962 = CARTESIAN_POINT ( 'NONE',  ( -45.39083524964373595, -290.3614852083207438, -343.3155004987569896 ) ) ;
#18963 = CARTESIAN_POINT ( 'NONE',  ( 2.197429475817664013, -229.5268262511776527, 22.47499999999998721 ) ) ;
#18964 = CARTESIAN_POINT ( 'NONE',  ( -108.8665964327379214, -292.2592061424039684, -293.0958316240797217 ) ) ;
#18965 = CARTESIAN_POINT ( 'NONE',  ( -19.78954960283480347, -290.2769892493946031, -197.2189484650397162 ) ) ;
#18966 = CARTESIAN_POINT ( 'NONE',  ( -25.79620902928468951, -296.9053838787326072, -344.5188280773609222 ) ) ;
#18967 = CARTESIAN_POINT ( 'NONE',  ( -4.499756205447580371, -287.4372382847431595, -204.9026183951946223 ) ) ;
#18968 = CARTESIAN_POINT ( 'NONE',  ( 32.75132232384592612, -295.9046202709194517, -297.5087997985771153 ) ) ;
#18969 = CARTESIAN_POINT ( 'NONE',  ( 36.86781725228782847, -277.3638169147595249, -257.1972860349069379 ) ) ;
#18970 = CARTESIAN_POINT ( 'NONE',  ( 14.60259654582348965, -275.1355370406461702, -326.7342650939074247 ) ) ;
#18971 = CARTESIAN_POINT ( 'NONE',  ( -73.19615735195343120, -296.7866442821683108, -202.3419951379497377 ) ) ;
#18972 = CARTESIAN_POINT ( 'NONE',  ( -32.37463725636051493, -275.2286638592689201, -344.2582562883887931 ) ) ;
#18973 = CARTESIAN_POINT ( 'NONE',  ( -67.87501289718414910, -277.7280919754755928, -202.4574011820792521 ) ) ;
#18974 = CARTESIAN_POINT ( 'NONE',  ( -101.0701116958632610, -274.2546520269584107, -233.8470664991680508 ) ) ;
#18975 = CARTESIAN_POINT ( 'NONE',  ( 0.9162446341252652449, -273.1268516302044986, -204.2026493507246414 ) ) ;
#18976 = EDGE_CURVE ( 'NONE', #9610, #66586, #59424, .T. ) ;
#18977 = CARTESIAN_POINT ( 'NONE',  ( -108.0303867941109388, -298.2458317151121037, -249.9042243939786658 ) ) ;
#18978 = CARTESIAN_POINT ( 'NONE',  ( 200.2296996224750103, 68.12454877777268791, 0.000000000000000000 ) ) ;
#18979 = CARTESIAN_POINT ( 'NONE',  ( -65.64460335955025982, -298.4751056735780139, -202.8959610797571713 ) ) ;
#18980 = LINE ( 'NONE', #83344, #11141 ) ;
#18982 = CARTESIAN_POINT ( 'NONE',  ( -35.38819928235388090, -273.9106354040160909, -197.3747554587496040 ) ) ;
#18981 = CARTESIAN_POINT ( 'NONE',  ( -8.878288440441002294, -286.7018021541762209, -340.1478584483220402 ) ) ;
#18983 = CARTESIAN_POINT ( 'NONE',  ( 19.62424641933716529, -288.2564058222681638, -322.1869436561482871 ) ) ;
#18984 = CARTESIAN_POINT ( 'NONE',  ( -17.73380864816265401, -288.4726624259701566, -344.8008579280377717 ) ) ;
#18985 = CARTESIAN_POINT ( 'NONE',  ( -62.32403971814561316, -299.7086724253267676, -199.2675914818975116 ) ) ;
#18986 = CARTESIAN_POINT ( 'NONE',  ( 32.28213816380046097, -291.9115183161393361, -297.9354097082195381 ) ) ;
#18987 = CARTESIAN_POINT ( 'NONE',  ( 30.58386087180263502, -280.2832315887928871, -234.3272300470326002 ) ) ;
#18988 = CARTESIAN_POINT ( 'NONE',  ( 152.8344704311132602, 129.4968913933752503, -12.52864452723162003 ) ) ;
#18989 = CARTESIAN_POINT ( 'NONE',  ( -51.23241710295501861, -277.8745459040279115, -196.6064122313974281 ) ) ;
#18990 = CARTESIAN_POINT ( 'NONE',  ( 197.2116943569230330, 275.5000000000000568, -12.92446933126074882 ) ) ;
#18991 = CARTESIAN_POINT ( 'NONE',  ( 10.36175281717805419, -287.1717352319661245, -326.2092279194358184 ) ) ;
#18992 = DIRECTION ( 'NONE',  ( -1.000000000000000000, 0.000000000000000000, 0.000000000000000000 ) ) ;
#18993 = CARTESIAN_POINT ( 'NONE',  ( -91.23628028588400696, -289.2856518755919524, -218.2039048864972415 ) ) ;
#18994 = CARTESIAN_POINT ( 'NONE',  ( -99.87899047268398078, -274.6052608698339554, -231.3765688876021045 ) ) ;
#18995 = CARTESIAN_POINT ( 'NONE',  ( 36.75539332297754669, -282.7421326655936582, -251.7002756421616425 ) ) ;
#18997 = CARTESIAN_POINT ( 'NONE',  ( -66.55957287216529039, -283.4457935327254745, -337.2724910204852904 ) ) ;
#18996 = CARTESIAN_POINT ( 'NONE',  ( -81.97561402377259299, -295.4677244935770091, -209.5820480055150767 ) ) ;
#18998 = CARTESIAN_POINT ( 'NONE',  ( -8.758589379694553756, -275.8587566877072845, -202.4954172976708264 ) ) ;
#18999 = CARTESIAN_POINT ( 'NONE',  ( 35.51574385217134733, -276.4426902996534068, -277.0240440181192980 ) ) ;
#19000 = CARTESIAN_POINT ( 'NONE',  ( -14.01905113807645442, -284.7497394030690430, -341.6426351596688846 ) ) ;
#19001 = CARTESIAN_POINT ( 'NONE',  ( -59.55627744073690621, -272.6780597559308603, -200.4456928389735708 ) ) ;
#19002 = ORIENTED_EDGE ( 'NONE', *, *, #73107, .F. ) ;
#19003 = DIRECTION ( 'NONE',  ( 0.000000000000000000, 0.000000000000000000, -1.000000000000000000 ) ) ;
#19004 = CARTESIAN_POINT ( 'NONE',  ( -11.05920414355691683, -294.5523030373764186, -342.7933069836394111 ) ) ;
#19005 = CARTESIAN_POINT ( 'NONE',  ( -108.0993679551943956, -286.8427680437682170, -246.4251853724435648 ) ) ;
#19006 = DIRECTION ( 'NONE',  ( -1.000000000000000000, 0.000000000000000000, 0.000000000000000000 ) ) ;
#19007 = CARTESIAN_POINT ( 'NONE',  ( 25.18497378105905682, -273.6952119285918457, -320.2651865833026363 ) ) ;
#19008 = CARTESIAN_POINT ( 'NONE',  ( -68.95829563863719613, -276.6545694870480361, -340.4079838042694632 ) ) ;
#19009 = CARTESIAN_POINT ( 'NONE',  ( -110.8555608138664752, -289.2064009549977754, -250.2579103794683135 ) ) ;
#19010 = CARTESIAN_POINT ( 'NONE',  ( -74.12624196631004736, -285.0702095508625575, -334.2753906971367996 ) ) ;
#19011 = VECTOR ( 'NONE', #52807, 1000.000000000000000 ) ;
#19012 = CARTESIAN_POINT ( 'NONE',  ( -8.320972237583498909, -278.4270535124706498, -338.4613497847494159 ) ) ;
#19013 = CARTESIAN_POINT ( 'NONE',  ( -73.97739404131314700, -284.9538915480133596, -337.4755898145663764 ) ) ;
#19014 = CARTESIAN_POINT ( 'NONE',  ( -21.31638399556991459, -281.6370667660092408, -342.0396619241350891 ) ) ;
#19015 = CARTESIAN_POINT ( 'NONE',  ( -2.234859526198311297, -282.5169013349871534, -204.0705372737294567 ) ) ;
#19016 = CARTESIAN_POINT ( 'NONE',  ( 28.50144580648328230, -275.1965741415396565, -230.3382679360367149 ) ) ;
#19017 = CARTESIAN_POINT ( 'NONE',  ( -104.9765986667826070, -277.9092091799133186, -307.1649289828673659 ) ) ;
#19018 = CARTESIAN_POINT ( 'NONE',  ( -36.96416287557057245, -296.9675092877473048, -344.8128343504163240 ) ) ;
#19019 = LINE ( 'NONE', #18535, #8770 ) ;
#19020 = CARTESIAN_POINT ( 'NONE',  ( -109.6285296886695733, -294.4014580894347546, -293.0964298822452747 ) ) ;
#19021 = CARTESIAN_POINT ( 'NONE',  ( 17.47725363303493751, -275.7491181336600334, -318.6797906538209872 ) ) ;
#19022 = CARTESIAN_POINT ( 'NONE',  ( -113.9451976302604379, -273.7928955659290295, -267.5237491005502761 ) ) ;
#19023 = CARTESIAN_POINT ( 'NONE',  ( 36.56304859358461101, -289.2490275679292040, -265.4980928583517539 ) ) ;
#19024 = CARTESIAN_POINT ( 'NONE',  ( -85.93873637189760473, -297.2317184728580060, -329.1916867306165386 ) ) ;
#19025 = CARTESIAN_POINT ( 'NONE',  ( 33.05774922560197382, -295.1453579721232927, -300.6932587163273638 ) ) ;
#19026 = CARTESIAN_POINT ( 'NONE',  ( -103.2459557649118551, -292.0794411352630959, -305.9202800335608003 ) ) ;
#19027 = CARTESIAN_POINT ( 'NONE',  ( -30.05924010357734133, -278.1442228727949555, -195.8313521715718935 ) ) ;
#19028 = CARTESIAN_POINT ( 'NONE',  ( -109.3720579153232961, -280.7161279424268514, -251.5242396855583706 ) ) ;
#19029 = CARTESIAN_POINT ( 'NONE',  ( -111.8253227037627511, -294.6177698717550015, -271.4604521233549121 ) ) ;
#19030 = CARTESIAN_POINT ( 'NONE',  ( -0.9476217701010717365, -284.4347738489031485, -336.8271290643297107 ) ) ;
#19031 = CARTESIAN_POINT ( 'NONE',  ( 35.86220529250802258, -286.4096721109496571, -265.5801862427985043 ) ) ;
#19032 = CARTESIAN_POINT ( 'NONE',  ( 46.88546938567958478, 11.31389355509462291, -331.4406996308803741 ) ) ;
#19033 = VERTEX_POINT ( 'NONE', #11874 ) ;
#19034 = CARTESIAN_POINT ( 'NONE',  ( -57.39611940224994413, -285.4529398884592410, -200.0951886219402525 ) ) ;
#19035 = EDGE_LOOP ( 'NONE', ( #50833, #50359, #8798, #18213 ) ) ;
#19036 = CARTESIAN_POINT ( 'NONE',  ( 17.61440780927308936, -283.3688226009854247, -323.9283089932884536 ) ) ;
#19037 = CARTESIAN_POINT ( 'NONE',  ( -48.88296166321605085, -274.2345039754250706, -198.2066231337833528 ) ) ;
#19038 = CARTESIAN_POINT ( 'NONE',  ( -15.51184499926307581, -285.1233564870236137, -196.8794037206927783 ) ) ;
#19039 = CARTESIAN_POINT ( 'NONE',  ( -38.17939962249425179, -280.9831412569245686, -193.6009820160768982 ) ) ;
#19040 = CARTESIAN_POINT ( 'NONE',  ( 194.7453183674700199, 20.99999999999999645, -15.62499999999999112 ) ) ;
#19041 = CARTESIAN_POINT ( 'NONE',  ( -67.10999394045602173, -281.1890335110183514, -200.1004857822151735 ) ) ;
#19042 = CARTESIAN_POINT ( 'NONE',  ( 29.26616279052587899, -281.3834569720291370, -231.7717815167536912 ) ) ;
#19043 = CARTESIAN_POINT ( 'NONE',  ( 7.399455738971487229, -279.9094976428775681, -326.5171145203363494 ) ) ;
#19044 = CARTESIAN_POINT ( 'NONE',  ( 190.6848901948926027, 270.9012093486809363, -139.6392467641786368 ) ) ;
#19045 = ORIENTED_EDGE ( 'NONE', *, *, #7154, .F. ) ;
#19046 = CARTESIAN_POINT ( 'NONE',  ( 22.12322928847072490, -276.9287847433913043, -224.9093112442553490 ) ) ;
#19047 = CARTESIAN_POINT ( 'NONE',  ( 44.58079383892317793, 12.73659974197433620, -331.8102939384928050 ) ) ;
#19048 = CARTESIAN_POINT ( 'NONE',  ( 18.82626069481717224, -280.2583195277787240, -319.5241832013510361 ) ) ;
#19049 = CARTESIAN_POINT ( 'NONE',  ( -36.41356295141496702, -293.8237733903442859, -194.3672561163407693 ) ) ;
#19050 = CARTESIAN_POINT ( 'NONE',  ( -20.83320936382524380, -294.1833337229817289, -341.6267926717862338 ) ) ;
#19051 = CARTESIAN_POINT ( 'NONE',  ( -44.88476794646827983, -291.4668766204152348, -193.7404312595681404 ) ) ;
#19052 = CARTESIAN_POINT ( 'NONE',  ( 200.4644824113734671, 275.5000000000000568, -2.942835885954290021 ) ) ;
#19054 = CARTESIAN_POINT ( 'NONE',  ( 34.16875774102882701, -285.7132766600460059, -252.0701301054242265 ) ) ;
#19053 = CARTESIAN_POINT ( 'NONE',  ( -83.84112659353174024, -294.2509448288038811, -331.0612449030070366 ) ) ;
#19055 = CARTESIAN_POINT ( 'NONE',  ( 29.51715895196011985, -295.8432727049249138, -302.7405321901514412 ) ) ;
#19056 = CARTESIAN_POINT ( 'NONE',  ( 27.45742738705570574, -286.7077717641705021, -305.1438205458529751 ) ) ;
#19057 = CARTESIAN_POINT ( 'NONE',  ( -105.0584267521073087, -286.2496327910332639, -241.6699811892725052 ) ) ;
#19058 = VERTEX_POINT ( 'NONE', #55447 ) ;
#19059 = CARTESIAN_POINT ( 'NONE',  ( -44.88588853948748891, -292.9002446658929557, -193.9152591176198825 ) ) ;
#19060 = CARTESIAN_POINT ( 'NONE',  ( -29.43176443758198246, -283.4417474349663735, -343.0437602525310581 ) ) ;
#19061 = CARTESIAN_POINT ( 'NONE',  ( -113.9407591959636079, -295.3567574941754970, -269.5911391662599499 ) ) ;
#19062 = CARTESIAN_POINT ( 'NONE',  ( -94.59782229122845365, -292.0515202943333293, -219.1176277080542150 ) ) ;
#19063 = CARTESIAN_POINT ( 'NONE',  ( -13.89118181700644428, -292.8406952314584828, -197.0276341407994209 ) ) ;
#19064 = CARTESIAN_POINT ( 'NONE',  ( 32.31425617400080341, -288.0103094660927354, -292.3707967870726065 ) ) ;
#19065 = EDGE_LOOP ( 'NONE', ( #32265, #90845, #27665, #39578 ) ) ;
#19066 = LINE ( 'NONE', #54562, #47269 ) ;
#19067 = CARTESIAN_POINT ( 'NONE',  ( -100.5839457998255995, -297.8538944069742911, -312.1779388397400226 ) ) ;
#19068 = CARTESIAN_POINT ( 'NONE',  ( -20.62698905467090071, -296.9421269185311303, -193.8579100128171149 ) ) ;
#19069 = CARTESIAN_POINT ( 'NONE',  ( -1.841558484049782729, -279.5935557865460055, -206.3052955172217651 ) ) ;
#19070 = ORIENTED_EDGE ( 'NONE', *, *, #85278, .F. ) ;
#19071 = ADVANCED_FACE ( 'NONE', ( #21324 ), #62400, .T. ) ;
#19072 = CARTESIAN_POINT ( 'NONE',  ( 38.86408800217596138, -274.9272246995406590, -259.7684432184076400 ) ) ;
#19073 = CARTESIAN_POINT ( 'NONE',  ( -95.82762422071574804, -295.6570911407147833, -225.5063748874037231 ) ) ;
#19074 = CARTESIAN_POINT ( 'NONE',  ( -74.61328858115132334, -279.4141855127528515, -334.5615399034859365 ) ) ;
#19075 = CARTESIAN_POINT ( 'NONE',  ( 35.84738177226173406, -273.5296548867451634, -257.8667889600991430 ) ) ;
#19076 = CARTESIAN_POINT ( 'NONE',  ( -88.76917945675440080, -296.9986580170072443, -322.7999311888759735 ) ) ;
#19077 = CARTESIAN_POINT ( 'NONE',  ( -107.7601042620882339, -297.9002866353736181, -249.9779280146009626 ) ) ;
#19078 = CARTESIAN_POINT ( 'NONE',  ( 199.5417009657504650, 26.45151344826108897, 10.49999999999999645 ) ) ;
#19079 = CARTESIAN_POINT ( 'NONE',  ( -110.8151805956194806, -297.8965663403694180, -290.5623081628882574 ) ) ;
#19080 = CARTESIAN_POINT ( 'NONE',  ( -51.43137961469841457, -295.8723580471684045, -196.4737386689759546 ) ) ;
#19081 = CARTESIAN_POINT ( 'NONE',  ( -72.68349467631576033, -292.2227669743808747, -206.3132154034420580 ) ) ;
#19082 = CARTESIAN_POINT ( 'NONE',  ( -86.30767457985406566, -289.9318046556179524, -215.3588743740152154 ) ) ;
#19083 = DIRECTION ( 'NONE',  ( -1.000000000000000000, -0.000000000000000000, -0.000000000000000000 ) ) ;
#19084 = CARTESIAN_POINT ( 'NONE',  ( 35.66956938950480804, -275.7368775982211559, -245.9263411066081346 ) ) ;
#19085 = CARTESIAN_POINT ( 'NONE',  ( -71.90960281324012726, -273.7487489490164307, -206.0081361520411747 ) ) ;
#19086 = CARTESIAN_POINT ( 'NONE',  ( -3.159272911374352955, -282.4812220372008937, -203.1904080733705769 ) ) ;
#19087 = AXIS2_PLACEMENT_3D ( 'NONE', #32553, #38696, #32069 ) ;
#19088 = CARTESIAN_POINT ( 'NONE',  ( 21.22165363788893444, -280.9041633259438413, -319.5915137754943203 ) ) ;
#19089 = CARTESIAN_POINT ( 'NONE',  ( -93.26557235102262666, -277.1784327708272144, -323.2185305411105674 ) ) ;
#19090 = CARTESIAN_POINT ( 'NONE',  ( -109.5789386915224526, -283.9029449644849024, -258.6894596859793864 ) ) ;
#19091 = CARTESIAN_POINT ( 'NONE',  ( 3.527015550632476515, -280.5041807362050008, -333.5080933350487271 ) ) ;
#19092 = EDGE_CURVE ( 'NONE', #13829, #67504, #44253, .T. ) ;
#19093 = CARTESIAN_POINT ( 'NONE',  ( -91.54435054112427395, -271.8357250074435569, -220.5685046757476186 ) ) ;
#19094 = CARTESIAN_POINT ( 'NONE',  ( -37.76180476151213128, -279.0575998057332754, -345.3725049901557895 ) ) ;
#19095 = FACE_OUTER_BOUND ( 'NONE', #21021, .T. ) ;
#19096 = DIRECTION ( 'NONE',  ( 0.000000000000000000, 0.000000000000000000, 1.000000000000000000 ) ) ;
#19097 = CARTESIAN_POINT ( 'NONE',  ( -113.5417001291471024, -270.9522813053617369, -270.3407899428912629 ) ) ;
#19098 = CARTESIAN_POINT ( 'NONE',  ( -112.2200814915740068, -280.6438772235991905, -263.2141941308548780 ) ) ;
#19099 = CARTESIAN_POINT ( 'NONE',  ( -40.84350783984969979, -272.0080689485911876, -195.3918459206030604 ) ) ;
#19100 = DIRECTION ( 'NONE',  ( -1.000000000000000000, -0.000000000000000000, -0.000000000000000000 ) ) ;
#19101 = CARTESIAN_POINT ( 'NONE',  ( -107.6968004657215232, -286.8299134348403641, -242.6601490968003816 ) ) ;
#19102 = CARTESIAN_POINT ( 'NONE',  ( -9.696358412319998621, -286.6908782887689995, -340.0937875371106429 ) ) ;
#19103 = CARTESIAN_POINT ( 'NONE',  ( 207.5863589332323329, 29.28491128719180026, 13.57731244650625513 ) ) ;
#19104 = CARTESIAN_POINT ( 'NONE',  ( 33.12712816227236345, -292.6176458556732314, -290.9312367272567030 ) ) ;
#19105 = CARTESIAN_POINT ( 'NONE',  ( 24.57721647626301831, -285.1319718354183692, -229.3178761208892524 ) ) ;
#19106 = CARTESIAN_POINT ( 'NONE',  ( 202.9738562182569694, 296.4636489450776367, -53.99999999999997868 ) ) ;
#19107 = CARTESIAN_POINT ( 'NONE',  ( -111.7929898901849981, -294.4303608837819866, -279.8338554059012608 ) ) ;
#19108 = CARTESIAN_POINT ( 'NONE',  ( -0.03809412471642474596, -285.0190603887202769, -203.7793299268059570 ) ) ;
#19109 = CARTESIAN_POINT ( 'NONE',  ( 34.53495670390901040, -282.9338591087963550, -253.6223420304083334 ) ) ;
#19110 = CARTESIAN_POINT ( 'NONE',  ( 38.62850208667887841, -279.7509763932390570, -267.1232116835210491 ) ) ;
#19111 = CARTESIAN_POINT ( 'NONE',  ( -88.66106809430590374, -289.7972933910598385, -322.2776131603669114 ) ) ;
#19112 = CARTESIAN_POINT ( 'NONE',  ( -107.0083868980533026, -280.2917782631946579, -246.4995038274308286 ) ) ;
#19113 = CARTESIAN_POINT ( 'NONE',  ( -11.69610293760054276, -281.1975261912533597, -201.7881685346277436 ) ) ;
#19114 = CARTESIAN_POINT ( 'NONE',  ( 36.50164532655497851, -289.7239724984143550, -285.3800106942805428 ) ) ;
#19115 = EDGE_LOOP ( 'NONE', ( #13220, #39488, #26158, #13808 ) ) ;
#19116 = CARTESIAN_POINT ( 'NONE',  ( -113.0682893601508709, -272.7301230832840133, -256.1307079426312612 ) ) ;
#19117 = CARTESIAN_POINT ( 'NONE',  ( -111.8898848917655755, -292.5927436484923874, -265.6565254940458658 ) ) ;
#19118 = CARTESIAN_POINT ( 'NONE',  ( 206.8376799756172204, 36.39179024836181497, 13.90950695095621015 ) ) ;
#19119 = CARTESIAN_POINT ( 'NONE',  ( -99.86837403722181250, -292.4090924074130839, -320.2651865833026363 ) ) ;
#19120 = ORIENTED_EDGE ( 'NONE', *, *, #84897, .T. ) ;
#19121 = CARTESIAN_POINT ( 'NONE',  ( 35.51468649724040461, -273.3149533264262345, -251.8685422326711887 ) ) ;
#19122 = DIRECTION ( 'NONE',  ( 1.000000000000000000, 0.000000000000000000, 0.000000000000000000 ) ) ;
#19123 = CARTESIAN_POINT ( 'NONE',  ( -103.9140130235631432, -294.4651158269297184, -307.5441959380592039 ) ) ;
#19124 = CARTESIAN_POINT ( 'NONE',  ( -99.94629275890376618, -296.5787989552235331, -232.5977301564361142 ) ) ;
#19125 = CARTESIAN_POINT ( 'NONE',  ( -7.924091673659301449, -290.1798445040051888, -337.9827716403593172 ) ) ;
#19126 = CARTESIAN_POINT ( 'NONE',  ( -8.073175706643860750, -284.4235629146169231, -338.3414643579641847 ) ) ;
#19127 = CARTESIAN_POINT ( 'NONE',  ( -53.28423573993921281, -293.2769756701276265, -195.5779116826343227 ) ) ;
#19128 = CARTESIAN_POINT ( 'NONE',  ( -65.25141332893073809, -290.7244247455753339, -341.6515393523510511 ) ) ;
#19129 = CARTESIAN_POINT ( 'NONE',  ( -97.38191157747579041, -287.1663516298240211, -225.4147759636723549 ) ) ;
#19130 = CARTESIAN_POINT ( 'NONE',  ( -97.69821886276980649, -279.3586402124670371, -222.5480376512654175 ) ) ;
#19131 = CARTESIAN_POINT ( 'NONE',  ( -101.0881710472737041, -295.1738866049096828, -229.7938695864031899 ) ) ;
#19132 = CARTESIAN_POINT ( 'NONE',  ( 22.52192514762148789, -282.0350669651697331, -318.8106966827294855 ) ) ;
#19133 = CARTESIAN_POINT ( 'NONE',  ( 16.32361754381321717, -276.6842517230317640, -218.9944411785646423 ) ) ;
#19134 = CARTESIAN_POINT ( 'NONE',  ( -82.13390479932378696, -275.9090924074130271, -214.2458315076590907 ) ) ;
#19135 = CARTESIAN_POINT ( 'NONE',  ( -109.4977049187817499, -276.3945724307605474, -293.6346733324220963 ) ) ;
#19136 = DIRECTION ( 'NONE',  ( 0.000000000000000000, 0.000000000000000000, 1.000000000000000000 ) ) ;
#19137 = CARTESIAN_POINT ( 'NONE',  ( 21.38217294224192599, -280.4506154646063578, -226.8717355002970351 ) ) ;
#19138 = CARTESIAN_POINT ( 'NONE',  ( -108.2829020371179212, -279.3882418821172564, -299.2636194198420867 ) ) ;
#19139 = CARTESIAN_POINT ( 'NONE',  ( -35.14292900344018733, -285.1378472560713817, -193.6148041650766345 ) ) ;
#19140 = CARTESIAN_POINT ( 'NONE',  ( -52.60027132107033054, -293.6142978870089451, -197.8850852416966291 ) ) ;
#19141 = CARTESIAN_POINT ( 'NONE',  ( 31.14530127559968165, -277.5870547306427056, -303.8875214355168737 ) ) ;
#19142 = CARTESIAN_POINT ( 'NONE',  ( 26.50970416140871322, -276.3095048748384102, -228.2149859799214369 ) ) ;
#19143 = CARTESIAN_POINT ( 'NONE',  ( 209.5027106082920056, 29.50523358103493621, 14.69807322781335479 ) ) ;
#19144 = CARTESIAN_POINT ( 'NONE',  ( 35.37841573153354346, -275.2939439364304803, -263.4228568230018368 ) ) ;
#19145 = CARTESIAN_POINT ( 'NONE',  ( -110.0750188786464321, -298.3250803534549505, -288.0188526371112516 ) ) ;
#19146 = CARTESIAN_POINT ( 'NONE',  ( -110.9929811818575871, -282.7234030662491477, -257.0408724347454950 ) ) ;
#19147 = CARTESIAN_POINT ( 'NONE',  ( 24.79989469958890780, -292.6155192340553413, -224.9280189923490241 ) ) ;
#19148 = CARTESIAN_POINT ( 'NONE',  ( -40.28721907734122709, -290.6886905126430065, -346.5171157729111542 ) ) ;
#19149 = CARTESIAN_POINT ( 'NONE',  ( -7.130349273065858640, -291.3784279388920595, -203.5666544844541477 ) ) ;
#19150 = ORIENTED_EDGE ( 'NONE', *, *, #47379, .F. ) ;
#19151 = CARTESIAN_POINT ( 'NONE',  ( -2.309683589954180771, -291.0812126288142281, -202.4394264261509591 ) ) ;
#19152 = CARTESIAN_POINT ( 'NONE',  ( -34.85231234756710705, -291.7510008970354534, -197.3824194786699593 ) ) ;
#19153 = ORIENTED_EDGE ( 'NONE', *, *, #23961, .F. ) ;
#19154 = CARTESIAN_POINT ( 'NONE',  ( 37.80815125157658230, -288.8238973310369033, -285.6579264225256338 ) ) ;
#19155 = EDGE_CURVE ( 'NONE', #65802, #26035, #36698, .T. ) ;
#19156 = CARTESIAN_POINT ( 'NONE',  ( -88.40988614964473413, -294.6681969542845536, -327.6471383155461581 ) ) ;
#19157 = CARTESIAN_POINT ( 'NONE',  ( -107.8360113200843671, -285.5972411640034352, -239.5055597734092316 ) ) ;
#19158 = CARTESIAN_POINT ( 'NONE',  ( 32.69102699790111188, -287.4753688959346505, -238.2771976502217228 ) ) ;
#19159 = CARTESIAN_POINT ( 'NONE',  ( -21.37946038499688228, -283.1751761666347988, -341.6682823668233482 ) ) ;
#19160 = CARTESIAN_POINT ( 'NONE',  ( 179.8324430359451469, 254.2804809356018438, -166.6962587909805507 ) ) ;
#19161 = CARTESIAN_POINT ( 'NONE',  ( 195.8903196521388850, 285.0434368066629531, -111.3771662356307246 ) ) ;
#19162 = CARTESIAN_POINT ( 'NONE',  ( 195.5810153702553578, 282.4170139924178784, -110.2874269805470533 ) ) ;
#19163 = CARTESIAN_POINT ( 'NONE',  ( 19.98840512737379171, -274.1089791189192511, -224.8893273668976462 ) ) ;
#19164 = CARTESIAN_POINT ( 'NONE',  ( 16.74998684707813013, -275.1794960946866695, -319.8602924183693403 ) ) ;
#19165 = CARTESIAN_POINT ( 'NONE',  ( -113.3277794448817417, -296.2119018351638147, -258.2094495888708252 ) ) ;
#19166 = CARTESIAN_POINT ( 'NONE',  ( -68.96539051565628142, -196.7406117984471052, -357.3712819849171751 ) ) ;
#19167 = CARTESIAN_POINT ( 'NONE',  ( -1.712334662834919641, -275.2748333539560690, -338.0652285700219863 ) ) ;
#19168 = CARTESIAN_POINT ( 'NONE',  ( -34.44277719179873287, -299.9492309039443967, -196.1249797147749518 ) ) ;
#19169 = CARTESIAN_POINT ( 'NONE',  ( -40.44279298285383817, -298.9554434094916360, -193.6071081001820744 ) ) ;
#19170 = CARTESIAN_POINT ( 'NONE',  ( 28.86307556313219891, -287.6275786598560558, -239.4594009245641644 ) ) ;
#19171 = CARTESIAN_POINT ( 'NONE',  ( -41.92568613099764008, -295.9112267315418308, -347.1150699620685032 ) ) ;
#19172 = CARTESIAN_POINT ( 'NONE',  ( -62.83057623854973173, -298.2213672155115773, -197.7674261231517505 ) ) ;
#19173 = CARTESIAN_POINT ( 'NONE',  ( 24.42838960059447473, -294.2573577986904638, -309.3592381204121011 ) ) ;
#19174 = ORIENTED_EDGE ( 'NONE', *, *, #63351, .T. ) ;
#19175 = CARTESIAN_POINT ( 'NONE',  ( 38.11471748469551812, -277.4104489510829126, -265.5074445544746595 ) ) ;
#19176 = CARTESIAN_POINT ( 'NONE',  ( -67.33268488774348270, -279.1768894789483397, -199.5086816342627003 ) ) ;
#19177 = CARTESIAN_POINT ( 'NONE',  ( -85.25014032811193943, -278.6741182138933368, -325.8195270661732934 ) ) ;
#19178 = CARTESIAN_POINT ( 'NONE',  ( 38.37272345668768025, -277.3937367117095505, -276.7876312898428637 ) ) ;
#19179 = CARTESIAN_POINT ( 'NONE',  ( -59.21224747668785682, -275.3539658206864260, -342.4727395087656419 ) ) ;
#19180 = CARTESIAN_POINT ( 'NONE',  ( -94.53625257169122165, -297.8455756013553923, -224.8344682116025410 ) ) ;
#19181 = CARTESIAN_POINT ( 'NONE',  ( -50.59499754121058857, -293.7994611848385489, -342.7470629117134990 ) ) ;
#19182 = CARTESIAN_POINT ( 'NONE',  ( 209.7513585654922679, 305.7026273589066818, -40.00000000000000711 ) ) ;
#19183 = CARTESIAN_POINT ( 'NONE',  ( -67.34424839344553959, -280.1614247869131873, -199.5135774400097830 ) ) ;
#19184 = CARTESIAN_POINT ( 'NONE',  ( -108.6072184209689055, -278.9281931386223619, -254.4853564134882333 ) ) ;
#19185 = CARTESIAN_POINT ( 'NONE',  ( 36.30511850056931422, -286.4989011540779416, -291.1321638049303147 ) ) ;
#19186 = CARTESIAN_POINT ( 'NONE',  ( -30.71290953486229824, -300.1351034432233860, -195.1921889355453743 ) ) ;
#19187 = CARTESIAN_POINT ( 'NONE',  ( 160.5350683151633291, 275.0000000000000568, 20.22542485937379908 ) ) ;
#19188 = AXIS2_PLACEMENT_3D ( 'NONE', #17976, #54415, #55837 ) ;
#19189 = CARTESIAN_POINT ( 'NONE',  ( -42.68589332596516783, -288.3183194308615498, -343.3778625224693997 ) ) ;
#19190 = CARTESIAN_POINT ( 'NONE',  ( -7.571567205648026544, -278.6876960848901490, -202.5850723548841472 ) ) ;
#19192 = CARTESIAN_POINT ( 'NONE',  ( -32.06760748982689080, -281.0649392113111844, -344.6140515634363055 ) ) ;
#19191 = CARTESIAN_POINT ( 'NONE',  ( -99.95964648073017145, -277.6568281901861610, -231.6068914038433206 ) ) ;
#19193 = CARTESIAN_POINT ( 'NONE',  ( -106.2146468188840487, -286.9421581721882148, -240.5416067929351698 ) ) ;
#19194 = CARTESIAN_POINT ( 'NONE',  ( -97.96820939095927372, -279.1847433690685421, -311.7320846099459004 ) ) ;
#19195 = CARTESIAN_POINT ( 'NONE',  ( 153.8597781956983113, 19.40377396060713266, -11.71176238812795134 ) ) ;
#19196 = CARTESIAN_POINT ( 'NONE',  ( -35.04778466501801404, -294.0810897511464646, -195.3833934152537211 ) ) ;
#19197 = CARTESIAN_POINT ( 'NONE',  ( -77.30133824385073638, -275.8196281508062384, -335.0535451644575460 ) ) ;
#19198 = CARTESIAN_POINT ( 'NONE',  ( -13.74465827841398102, -277.3891975232490950, -339.6030040671423080 ) ) ;
#19199 = CARTESIAN_POINT ( 'NONE',  ( -89.15549691237981733, -285.7786127769256268, -324.8875706930659248 ) ) ;
#19200 = CARTESIAN_POINT ( 'NONE',  ( 140.6539576904058606, 130.0000000000000568, -12.50000000000000000 ) ) ;
#19201 = CARTESIAN_POINT ( 'NONE',  ( -96.15354890874544935, -291.8239821709321404, -317.8207460599227261 ) ) ;
#19202 = CARTESIAN_POINT ( 'NONE',  ( -95.93821868842539402, -293.9081572155508297, -317.1941802727007484 ) ) ;
#19203 = EDGE_CURVE ( 'NONE', #91332, #93704, #7129, .T. ) ;
#19204 = CARTESIAN_POINT ( 'NONE',  ( 31.28218055757993454, -286.3035850472850257, -235.7934767607450226 ) ) ;
#19205 = FACE_OUTER_BOUND ( 'NONE', #69708, .T. ) ;
#19206 = CARTESIAN_POINT ( 'NONE',  ( 5.671946108636324979, -275.1408140073654067, -330.0148047846920463 ) ) ;
#19207 = CARTESIAN_POINT ( 'NONE',  ( 32.69768401439767302, -292.0154469445254222, -295.1187568085193789 ) ) ;
#19208 = CARTESIAN_POINT ( 'NONE',  ( 197.1656530321902494, 41.90019538913895758, 12.64285714285713169 ) ) ;
#19209 = CARTESIAN_POINT ( 'NONE',  ( 197.2304840627181477, 41.97094794048064870, 11.95796701298976572 ) ) ;
#19210 = CARTESIAN_POINT ( 'NONE',  ( -44.80974917579993644, -290.4392675593994113, -194.3683274290261238 ) ) ;
#19211 = CARTESIAN_POINT ( 'NONE',  ( -86.27163083601209337, -286.9602894620695110, -215.0451526915797160 ) ) ;
#19212 = CARTESIAN_POINT ( 'NONE',  ( 35.80281138171877586, -286.0540058276777700, -290.9965100657445305 ) ) ;
#19213 = CARTESIAN_POINT ( 'NONE',  ( -110.8988318193390796, -286.0058719838534103, -268.1878041858792585 ) ) ;
#19214 = EDGE_CURVE ( 'NONE', #6475, #62648, #26070, .T. ) ;
#19215 = CARTESIAN_POINT ( 'NONE',  ( 152.6878565075764413, 20.88255170682893080, -8.268021619243398845 ) ) ;
#19216 = CARTESIAN_POINT ( 'NONE',  ( -73.64462034686829384, -286.3599454160650453, -206.8273026964639598 ) ) ;
#19217 = CARTESIAN_POINT ( 'NONE',  ( 37.58773696906638406, -295.4237301880644395, -261.8853295629847366 ) ) ;
#19218 = CARTESIAN_POINT ( 'NONE',  ( -4.640606255320009588, -274.7046195760476053, -338.4925409304452160 ) ) ;
#19219 = CARTESIAN_POINT ( 'NONE',  ( 14.87195484190964656, -276.6736462525976208, -326.9976038943935350 ) ) ;
#19220 = CARTESIAN_POINT ( 'NONE',  ( -53.06533541039279100, -289.9320876350648746, -196.4017464581970103 ) ) ;
#19221 = CARTESIAN_POINT ( 'NONE',  ( -99.42786816593280719, -279.1572650174151136, -224.7942965060165363 ) ) ;
#19222 = CARTESIAN_POINT ( 'NONE',  ( -71.66517040781522496, -297.4878114800368394, -336.6607546392650647 ) ) ;
#19223 = DIRECTION ( 'NONE',  ( 0.000000000000000000, 0.000000000000000000, 1.000000000000000000 ) ) ;
#19224 = CYLINDRICAL_SURFACE ( 'NONE', #81359, 35.00000000000002842 ) ;
#19225 = CARTESIAN_POINT ( 'NONE',  ( -30.46859702267936143, -284.8255638981279958, -197.1389164006562851 ) ) ;
#19226 = CARTESIAN_POINT ( 'NONE',  ( -97.90694129153108349, -276.1020812294920006, -313.3100845624825297 ) ) ;
#19227 = CARTESIAN_POINT ( 'NONE',  ( 12.33647257618995674, -280.3607973171270373, -326.6181222355833143 ) ) ;
#19228 = CARTESIAN_POINT ( 'NONE',  ( -54.94434090351493438, 0.000000000000000000, 74.50000000000001421 ) ) ;
#19229 = CARTESIAN_POINT ( 'NONE',  ( 35.07813996601782236, -273.7247329064165342, -246.1512484178971647 ) ) ;
#19230 = CARTESIAN_POINT ( 'NONE',  ( -80.88673780970184168, -277.0098056950945988, -329.0784268544667270 ) ) ;
#19231 = CARTESIAN_POINT ( 'NONE',  ( -7.691753305845443478, -296.1764699141970709, -337.8402871408548549 ) ) ;
#19232 = PRODUCT_DEFINITION ( 'UNKNOWN', '', #50708, #7762 ) ;
#19233 = CARTESIAN_POINT ( 'NONE',  ( 38.96906939831934835, -280.5746744134050346, -278.4994459607108865 ) ) ;
#19234 = CARTESIAN_POINT ( 'NONE',  ( -20.78335903422243902, -295.7757426783928167, -341.7522306533316510 ) ) ;
#19235 = CARTESIAN_POINT ( 'NONE',  ( -36.91721156693651551, -299.3725293809989694, -193.8541723928366309 ) ) ;
#19236 = CARTESIAN_POINT ( 'NONE',  ( -110.2095571528937796, -272.2907884077905578, -264.9076476289289985 ) ) ;
#19237 = CARTESIAN_POINT ( 'NONE',  ( -82.96532920742994577, -293.4285347675631215, -210.7682030704291094 ) ) ;
#19238 = CARTESIAN_POINT ( 'NONE',  ( -35.15036386621238051, -286.2456001408052657, -193.3791623395837860 ) ) ;
#19239 = CARTESIAN_POINT ( 'NONE',  ( 37.90785305008348871, -273.8094307723012548, -279.6208324128426170 ) ) ;
#19240 = CARTESIAN_POINT ( 'NONE',  ( 28.90266363740056832, -287.8968621647022701, -309.6126692104884910 ) ) ;
#19241 = CARTESIAN_POINT ( 'NONE',  ( -32.88954751117633180, -282.0884243912386182, -195.8492052368922884 ) ) ;
#19242 = CARTESIAN_POINT ( 'NONE',  ( 34.80128781790409676, -286.4414312600176231, -257.4733000395002023 ) ) ;
#19243 = CARTESIAN_POINT ( 'NONE',  ( -52.94763135209608151, -289.8520940826414858, -196.9496342952077157 ) ) ;
#19244 = ORIENTED_EDGE ( 'NONE', *, *, #27513, .F. ) ;
#19245 = CARTESIAN_POINT ( 'NONE',  ( 164.1991770243031681, 231.0496910105122765, -188.4318802409405009 ) ) ;
#19246 = CARTESIAN_POINT ( 'NONE',  ( 32.73076934925363446, -286.7858086738262386, -249.6327390865224345 ) ) ;
#19247 = FACE_OUTER_BOUND ( 'NONE', #50322, .T. ) ;
#19248 = CARTESIAN_POINT ( 'NONE',  ( 0.7620111289098248086, -283.4981740433552773, -337.0165884279342663 ) ) ;
#19249 = CARTESIAN_POINT ( 'NONE',  ( -111.0029971093512557, -289.8827438656514914, -248.7547869612925240 ) ) ;
#19250 = CARTESIAN_POINT ( 'NONE',  ( 0.9541017032971741418, -282.1539631844422047, -204.4233466335672347 ) ) ;
#19251 = CARTESIAN_POINT ( 'NONE',  ( 32.71461710192765082, -282.4726592047770168, -239.6135865750992195 ) ) ;
#19252 = CARTESIAN_POINT ( 'NONE',  ( 34.70321745139083447, -281.5407355279730268, -282.1309886479731972 ) ) ;
#19253 = CARTESIAN_POINT ( 'NONE',  ( 35.53583224254434469, -277.7804538051685199, -288.1315569825152352 ) ) ;
#19254 = CARTESIAN_POINT ( 'NONE',  ( 13.39582739010140955, -294.3653761964523028, -328.3516132997970089 ) ) ;
#19255 = CARTESIAN_POINT ( 'NONE',  ( -95.55821391285505229, -289.2182366478500626, -223.6216074237341047 ) ) ;
#19256 = CARTESIAN_POINT ( 'NONE',  ( -94.07557479271419254, -272.0033672433459628, -223.7754103272211808 ) ) ;
#19257 = ORIENTED_EDGE ( 'NONE', *, *, #18859, .F. ) ;
#19258 = ORIENTED_EDGE ( 'NONE', *, *, #88840, .T. ) ;
#19259 = CARTESIAN_POINT ( 'NONE',  ( -97.06267273757688940, -285.8610062081989440, -314.7989355585051499 ) ) ;
#19260 = CARTESIAN_POINT ( 'NONE',  ( 37.16300026672992374, -294.8607809645405382, -288.5969262331369691 ) ) ;
#19261 = CARTESIAN_POINT ( 'NONE',  ( 17.68705264205629035, -282.8891997407130248, -318.4831403524349298 ) ) ;
#19262 = CARTESIAN_POINT ( 'NONE',  ( 25.86630329801068129, -275.1888213164584727, -314.0141914818792088 ) ) ;
#19263 = CARTESIAN_POINT ( 'NONE',  ( -110.3367714222608953, -291.5102982578577553, -246.0069840434583455 ) ) ;
#19264 = CARTESIAN_POINT ( 'NONE',  ( -113.0906860500255391, -282.7326402546606232, -267.1428584951389098 ) ) ;
#19265 = CARTESIAN_POINT ( 'NONE',  ( -64.38535207857050580, -292.0421006777201001, -198.2328756303478485 ) ) ;
#19266 = CARTESIAN_POINT ( 'NONE',  ( 33.72264406068770626, -288.1068872051334324, -287.1523797545385719 ) ) ;
#19267 = CARTESIAN_POINT ( 'NONE',  ( 175.2296996224750103, 20.99999999999998934, 0.000000000000000000 ) ) ;
#19268 = CARTESIAN_POINT ( 'NONE',  ( 151.2975037349263800, 130.0000000000000568, 12.50000000000000000 ) ) ;
#19269 = CARTESIAN_POINT ( 'NONE',  ( -76.58874877760752042, -208.1735614672835197, -353.4623537001039040 ) ) ;
#19270 = CARTESIAN_POINT ( 'NONE',  ( -95.72720533505923868, -285.4044566034078798, -319.5121797396082570 ) ) ;
#19271 = CARTESIAN_POINT ( 'NONE',  ( -85.33152481854864391, -281.1952119285918457, -330.4860931364850671 ) ) ;
#19272 = ORIENTED_EDGE ( 'NONE', *, *, #31803, .F. ) ;
#19273 = CARTESIAN_POINT ( 'NONE',  ( 25.81839340915425396, -280.9827083662730161, -307.6773701161826011 ) ) ;
#19274 = CARTESIAN_POINT ( 'NONE',  ( 34.16303839569806655, -275.5822831477111095, -299.0147507613526159 ) ) ;
#19275 = CARTESIAN_POINT ( 'NONE',  ( -68.08211249619313321, -281.6477724909933045, -202.1192003733392824 ) ) ;
#19276 = CARTESIAN_POINT ( 'NONE',  ( 155.4638711370593569, 204.8809718456330415, -215.8888951672738585 ) ) ;
#19277 = CARTESIAN_POINT ( 'NONE',  ( -9.062181949930447900, -278.9895656462564943, -199.3760833295065424 ) ) ;
#19278 = CARTESIAN_POINT ( 'NONE',  ( -97.06717561235315372, -283.1869425323889686, -225.5870810443808523 ) ) ;
#19279 = CARTESIAN_POINT ( 'NONE',  ( -57.14748864760450431, -299.5603315045846102, -196.9464592911140528 ) ) ;
#19280 = CARTESIAN_POINT ( 'NONE',  ( 6.104563476882358231, -294.9371745107561651, -329.1643668735893584 ) ) ;
#19281 = EDGE_LOOP ( 'NONE', ( #22757, #40417, #70408, #8547 ) ) ;
#19282 = CARTESIAN_POINT ( 'NONE',  ( -110.7370991443813892, -289.2982078910837345, -265.6876807222027992 ) ) ;
#19283 = CARTESIAN_POINT ( 'NONE',  ( -56.89009676848863961, -277.9491165894031042, -344.7879520330303080 ) ) ;
#19284 = CARTESIAN_POINT ( 'NONE',  ( -32.69103204684299868, -274.1123625625297109, -197.4968841856502593 ) ) ;
#19285 = CARTESIAN_POINT ( 'NONE',  ( -41.16355307362950100, -272.9255770132322141, -193.7134674802490792 ) ) ;
#19286 = DIRECTION ( 'NONE',  ( 1.000000000000000000, 0.000000000000000000, -0.000000000000000000 ) ) ;
#19287 = CARTESIAN_POINT ( 'NONE',  ( 23.86119083419642095, -272.9626433515699659, -226.9893269079989295 ) ) ;
#19288 = CARTESIAN_POINT ( 'NONE',  ( -43.53335921173260914, -248.9562857179395508, -480.6412943097532207 ) ) ;
#19289 = CARTESIAN_POINT ( 'NONE',  ( 35.99627554596227696, -282.6082011210353357, -268.5623309648966597 ) ) ;
#19290 = CARTESIAN_POINT ( 'NONE',  ( 36.98867910418877614, -283.1115329481219192, -254.5202117064272329 ) ) ;
#19291 = CARTESIAN_POINT ( 'NONE',  ( -88.97215051655771845, -283.1497116781166028, -322.1834016919127066 ) ) ;
#19292 = CARTESIAN_POINT ( 'NONE',  ( 1.045801265805477387, -272.9737015388060968, -207.3306479573419665 ) ) ;
#19293 = CARTESIAN_POINT ( 'NONE',  ( 7.876262782212916314, -282.5373320520805578, -211.4216398369878505 ) ) ;
#19294 = CARTESIAN_POINT ( 'NONE',  ( 1.217866415617300913, -275.0073707914935426, -333.2212889912209448 ) ) ;
#19295 = DIRECTION ( 'NONE',  ( 0.6056179655966478226, -0.7957555401921982963, -0.000000000000000000 ) ) ;
#19296 = CARTESIAN_POINT ( 'NONE',  ( 33.15347234365612650, -276.3648219298077606, -250.0637712767699270 ) ) ;
#19297 = LINE ( 'NONE', #17900, #33505 ) ;
#19298 = CARTESIAN_POINT ( 'NONE',  ( -99.30372800989310633, -279.9599678542490437, -224.8981122928330194 ) ) ;
#19299 = ORIENTED_EDGE ( 'NONE', *, *, #85804, .F. ) ;
#19300 = CARTESIAN_POINT ( 'NONE',  ( 200.3378311594553622, 16.04715669186171922, 10.05743975622762498 ) ) ;
#19301 = CARTESIAN_POINT ( 'NONE',  ( -57.45126543052634105, -287.6558475347466128, -197.2593302120670273 ) ) ;
#19302 = CARTESIAN_POINT ( 'NONE',  ( -94.07423630157281025, -295.0966795284489876, -316.5762764205593953 ) ) ;
#19303 = CARTESIAN_POINT ( 'NONE',  ( -69.32248810350432677, -288.8105656559068848, -340.3079334664897146 ) ) ;
#19304 = CARTESIAN_POINT ( 'NONE',  ( 9.691465384147978313, -284.9497063866011786, -213.2134552761442592 ) ) ;
#19306 = CARTESIAN_POINT ( 'NONE',  ( -100.5657489523968593, -289.3147396615349862, -231.8813354662964912 ) ) ;
#19305 = CARTESIAN_POINT ( 'NONE',  ( 34.57568247128498484, -285.9227753921196609, -254.7641631827181072 ) ) ;
#19307 = CARTESIAN_POINT ( 'NONE',  ( -95.42128366494856095, -285.1285621727255943, -315.2580422649932075 ) ) ;
#19308 = CARTESIAN_POINT ( 'NONE',  ( -2.422104263145531622, -274.5899576302240916, -336.7359812670925976 ) ) ;
#19309 = CARTESIAN_POINT ( 'NONE',  ( 11.57973657644783749, -285.1173745097558481, -211.8702211287368300 ) ) ;
#19310 = CARTESIAN_POINT ( 'NONE',  ( -86.17973997582254242, -299.3754136886805668, -213.3729853843608737 ) ) ;
#19311 = CARTESIAN_POINT ( 'NONE',  ( 36.30676224294442278, -285.7445636035419056, -285.3921665295383150 ) ) ;
#19312 = CARTESIAN_POINT ( 'NONE',  ( 5.049630586105095631, -281.5824673427633229, -210.6419122963373525 ) ) ;
#19313 = CARTESIAN_POINT ( 'NONE',  ( 15.41773474911120623, -290.3092396126820631, -323.9729513598685458 ) ) ;
#19314 = DIRECTION ( 'NONE',  ( 0.000000000000000000, 0.000000000000000000, 1.000000000000000000 ) ) ;
#19315 = CARTESIAN_POINT ( 'NONE',  ( 154.0637704119390037, 19.72112694978656577, -13.30738029212319162 ) ) ;
#19316 = CARTESIAN_POINT ( 'NONE',  ( -93.56345401848219012, -297.7740741019533743, -320.8623505491577816 ) ) ;
#19317 = CARTESIAN_POINT ( 'NONE',  ( -57.63042878020125670, -277.7900246726454725, -198.1574606256745881 ) ) ;
#19318 = CARTESIAN_POINT ( 'NONE',  ( -37.78382080134698384, -291.2439184691713763, -193.5238656197525700 ) ) ;
#19319 = CARTESIAN_POINT ( 'NONE',  ( -109.8276189887545655, -295.1338145041859775, -256.4291338908207649 ) ) ;
#19320 = CARTESIAN_POINT ( 'NONE',  ( 28.22890427824656356, -279.7879969233286488, -237.0557682084490807 ) ) ;
#19321 = CARTESIAN_POINT ( 'NONE',  ( -49.07883902702410239, -271.9814315128986095, -196.8000682633288818 ) ) ;
#19322 = CARTESIAN_POINT ( 'NONE',  ( 15.21654807871645509, -294.1283480494853393, -218.9182737601863664 ) ) ;
#19323 = CARTESIAN_POINT ( 'NONE',  ( -106.6662871844225293, -299.4805209788416391, -237.0123917617630696 ) ) ;
#19324 = CARTESIAN_POINT ( 'NONE',  ( -112.4531982868974751, -295.2018061084520468, -256.9085866942377834 ) ) ;
#19325 = CARTESIAN_POINT ( 'NONE',  ( -6.233322651633932843, -292.8888790201270353, -339.6881896576142594 ) ) ;
#19326 = CARTESIAN_POINT ( 'NONE',  ( -86.33473845658161849, -292.7818904339169990, -215.3829797432403552 ) ) ;
#19327 = DIRECTION ( 'NONE',  ( 0.000000000000000000, 0.000000000000000000, 1.000000000000000000 ) ) ;
#19328 = CARTESIAN_POINT ( 'NONE',  ( -89.93949945674523860, -292.0881928938936767, -219.5076694002517570 ) ) ;
#19329 = DIRECTION ( 'NONE',  ( -0.000000000000000000, -0.000000000000000000, -1.000000000000000000 ) ) ;
#19330 = CARTESIAN_POINT ( 'NONE',  ( -112.1741428937693712, -291.5513785533925670, -286.7353120116117680 ) ) ;
#19332 = CARTESIAN_POINT ( 'NONE',  ( 10.93080629530809667, -292.7419188015177838, -215.5326838798079621 ) ) ;
#19331 = CARTESIAN_POINT ( 'NONE',  ( 10.42998291966162761, -280.4169801292837860, -328.7061751592140695 ) ) ;
#19333 = CARTESIAN_POINT ( 'NONE',  ( 22.87531297833881894, -280.9094443014819831, -222.3514976036543942 ) ) ;
#19334 = CARTESIAN_POINT ( 'NONE',  ( -110.2060370730548726, -283.9059354087220299, -295.1911943630058204 ) ) ;
#19335 = CARTESIAN_POINT ( 'NONE',  ( -98.06071458232067073, -287.9553087247246026, -314.1015993713901935 ) ) ;
#19336 = CARTESIAN_POINT ( 'NONE',  ( -106.3711201022286588, -282.3308680365232135, -297.8105844061078074 ) ) ;
#19337 = CARTESIAN_POINT ( 'NONE',  ( -2.687559918590475050, -278.9817740087083280, -202.3627121064109815 ) ) ;
#19338 = CARTESIAN_POINT ( 'NONE',  ( -3.612852668795328182, -285.4071906515711134, -201.4709808852229855 ) ) ;
#19339 = CARTESIAN_POINT ( 'NONE',  ( 196.9624057960931509, 41.89407144457039323, 12.94963709701906751 ) ) ;
#19340 = CARTESIAN_POINT ( 'NONE',  ( 4.945544221397195628, -294.2339694101602845, -209.8151869044908153 ) ) ;
#19341 = CARTESIAN_POINT ( 'NONE',  ( 14.49686612503592720, -277.7654615448470281, -326.5702062463382163 ) ) ;
#19342 = CARTESIAN_POINT ( 'NONE',  ( -43.21301939045737583, -276.7950518690103081, -343.1458354506034993 ) ) ;
#19343 = CARTESIAN_POINT ( 'NONE',  ( -111.2327617711435721, -290.9904969963481562, -248.7021472365947545 ) ) ;
#19344 = CARTESIAN_POINT ( 'NONE',  ( 16.77749209836053979, -280.3694807798769943, -323.1656105699629506 ) ) ;
#19345 = CARTESIAN_POINT ( 'NONE',  ( 6.827659768009302965, -291.7289121733602428, -211.9447153736229836 ) ) ;
#19346 = CARTESIAN_POINT ( 'NONE',  ( -111.2378981130450910, -294.3836093657660058, -283.4751613437791775 ) ) ;
#19347 = ORIENTED_EDGE ( 'NONE', *, *, #60229, .T. ) ;
#19348 = CARTESIAN_POINT ( 'NONE',  ( 201.2509219215139922, 65.09645894978946501, 0.000000000000000000 ) ) ;
#19349 = CARTESIAN_POINT ( 'NONE',  ( 33.50419931762212400, -293.2952676138845050, -288.2174046506316358 ) ) ;
#19350 = CARTESIAN_POINT ( 'NONE',  ( 120.8395553409046528, -296.8152984961567427, -195.3611179825600175 ) ) ;
#19351 = CARTESIAN_POINT ( 'NONE',  ( -105.5795714935544112, -282.2666405000203440, -254.7536222014695397 ) ) ;
#19352 = CARTESIAN_POINT ( 'NONE',  ( -90.55762577094819221, -294.8423941055107207, -325.7595832190785359 ) ) ;
#19353 = CARTESIAN_POINT ( 'NONE',  ( 38.47453809775845457, -279.6866472146214164, -269.9608258604031334 ) ) ;
#19354 = CARTESIAN_POINT ( 'NONE',  ( -1.217290840402611707, -287.8364056609063937, -202.9198448089321403 ) ) ;
#19355 = CARTESIAN_POINT ( 'NONE',  ( 34.96007745442040715, -287.5195431365880836, -280.5244969956690397 ) ) ;
#19356 = CARTESIAN_POINT ( 'NONE',  ( -62.00378850043031065, -278.8986713685884524, -339.8595075047044247 ) ) ;
#19357 = CARTESIAN_POINT ( 'NONE',  ( -72.93049307174983653, -293.5461813092999819, -335.9903784861277245 ) ) ;
#19358 = CARTESIAN_POINT ( 'NONE',  ( -111.2524442055989340, -298.2616144368424216, -274.2567464536628563 ) ) ;
#19359 = CARTESIAN_POINT ( 'NONE',  ( -108.9910380518414712, -277.5566596118563325, -254.3818652144164787 ) ) ;
#19360 = EDGE_LOOP ( 'NONE', ( #22867, #53348, #37110, #25874 ) ) ;
#19361 = DIRECTION ( 'NONE',  ( 0.000000000000000000, 0.000000000000000000, 1.000000000000000000 ) ) ;
#19362 = CARTESIAN_POINT ( 'NONE',  ( -92.68475354843974401, -295.4856827975393117, -323.8671057746762472 ) ) ;
#19363 = CARTESIAN_POINT ( 'NONE',  ( -42.74448929455780899, -291.0408666532099460, -344.6564001954229752 ) ) ;
#19364 = CARTESIAN_POINT ( 'NONE',  ( 36.32840533430368879, -295.3986030066924400, -289.8330459380111392 ) ) ;
#19365 = CARTESIAN_POINT ( 'NONE',  ( 199.2296996224018812, 66.10105075032893751, -2.340466192624005792 ) ) ;
#19366 = CARTESIAN_POINT ( 'NONE',  ( -43.50953176532448907, -251.5913190049807611, -450.1129310769470067 ) ) ;
#19367 = CARTESIAN_POINT ( 'NONE',  ( 17.64932773812103406, -281.3482250297483347, -323.9983051005348784 ) ) ;
#19368 = CARTESIAN_POINT ( 'NONE',  ( -107.0704490825032593, -296.7880487345041161, -302.7835539724968612 ) ) ;
#19369 = CARTESIAN_POINT ( 'NONE',  ( -113.1325893188627560, -288.7171284882096529, -268.3632572824193403 ) ) ;
#19370 = CARTESIAN_POINT ( 'NONE',  ( -87.45171586596606517, -297.7088026291820029, -211.8551487525683115 ) ) ;
#19371 = CARTESIAN_POINT ( 'NONE',  ( 204.6539576904058606, 291.1800221208779931, -7.500000000000000000 ) ) ;
#19372 = CYLINDRICAL_SURFACE ( 'NONE', #25030, 2.000000000000000000 ) ;
#19373 = CARTESIAN_POINT ( 'NONE',  ( 197.2116943569230045, 249.5000000000000568, -12.42446933126075592 ) ) ;
#19374 = CARTESIAN_POINT ( 'NONE',  ( -34.67152081584604417, -290.5392847426256822, -346.6210543625663831 ) ) ;
#19375 = CARTESIAN_POINT ( 'NONE',  ( -99.90806341382572953, -275.6948066931273047, -220.5068182859052968 ) ) ;
#19376 = ORIENTED_EDGE ( 'NONE', *, *, #83986, .F. ) ;
#19377 = ADVANCED_FACE ( 'NONE', ( #79098 ), #26989, .T. ) ;
#19378 = CARTESIAN_POINT ( 'NONE',  ( -2.428998617669638538, -279.8503422498260989, -201.8306003024534050 ) ) ;
#19379 = CARTESIAN_POINT ( 'NONE',  ( -112.2247868479535242, -286.5447593951460021, -270.9484879699466546 ) ) ;
#19380 = EDGE_CURVE ( 'NONE', #67504, #13829, #71466, .T. ) ;
#19381 = CARTESIAN_POINT ( 'NONE',  ( -26.68518726441089228, -284.7597618869936014, -194.6440001154971924 ) ) ;
#19382 = CARTESIAN_POINT ( 'NONE',  ( 25.34277220506094608, -272.9995144579653470, -229.4870998971572646 ) ) ;
#19383 = CARTESIAN_POINT ( 'NONE',  ( -81.95316389797478962, -275.3594204872909472, -210.7050505781511447 ) ) ;
#19384 = CARTESIAN_POINT ( 'NONE',  ( -85.63751318266520229, -287.8058732304746741, -327.0756974491847018 ) ) ;
#19385 = CARTESIAN_POINT ( 'NONE',  ( -110.6265399009983241, -280.1673916383721803, -289.6379983987773699 ) ) ;
#19386 = ORIENTED_EDGE ( 'NONE', *, *, #80976, .F. ) ;
#19388 = CARTESIAN_POINT ( 'NONE',  ( -14.26884904698354184, -279.7078560988997538, -200.9423640825450548 ) ) ;
#19387 = CARTESIAN_POINT ( 'NONE',  ( -59.73363206496299682, -279.7539979123742455, -200.8268705012600606 ) ) ;
#19389 = CARTESIAN_POINT ( 'NONE',  ( 38.83223831995906039, -276.7490441371188581, -279.6965678161697610 ) ) ;
#19390 = CARTESIAN_POINT ( 'NONE',  ( 38.40446978103273779, -280.1991257847736847, -258.5918179892675539 ) ) ;
#19391 = CARTESIAN_POINT ( 'NONE',  ( 166.0191155783938370, 231.4420791936586852, -190.6152028106120895 ) ) ;
#19392 = CARTESIAN_POINT ( 'NONE',  ( 37.05422437480636688, -276.2558900577091663, -251.4384693542097011 ) ) ;
#19393 = CARTESIAN_POINT ( 'NONE',  ( 30.12263164617074551, -300.3064692177213715, -193.9343428704701182 ) ) ;
#19394 = CARTESIAN_POINT ( 'NONE',  ( 35.77081079830085031, -283.8376638359844719, -253.6410175316879361 ) ) ;
#19395 = VERTEX_POINT ( 'NONE', #49730 ) ;
#19396 = AXIS2_PLACEMENT_3D ( 'NONE', #21830, #50223, #79127 ) ;
#19397 = CARTESIAN_POINT ( 'NONE',  ( 82.64890176555634582, -299.5541904835127980, -195.3611179825600175 ) ) ;
#19398 = CARTESIAN_POINT ( 'NONE',  ( 34.29515255759648795, -288.4273135979447034, -254.7923218847039664 ) ) ;
#19399 = CARTESIAN_POINT ( 'NONE',  ( 34.99012493043350958, -289.6089768121959764, -293.6437530815389323 ) ) ;
#19400 = CARTESIAN_POINT ( 'NONE',  ( -96.64616049843958479, -289.3038380930856874, -313.1030604813448122 ) ) ;
#19401 = CARTESIAN_POINT ( 'NONE',  ( -26.62347082025265976, -285.6925367351441878, -194.1194309527787993 ) ) ;
#19402 = CARTESIAN_POINT ( 'NONE',  ( -46.98879273849259164, -155.5777431771304009, -365.1571803742538691 ) ) ;
#19403 = CARTESIAN_POINT ( 'NONE',  ( -6.942361788622357643, -281.0463124202631775, -337.6231815527979734 ) ) ;
#19404 = CARTESIAN_POINT ( 'NONE',  ( -74.18897684265721182, -287.4173580660720404, -205.9014855633704428 ) ) ;
#19405 = CARTESIAN_POINT ( 'NONE',  ( -38.91914892066086651, -281.5521366313458884, -344.0501781010830200 ) ) ;
#19406 = CARTESIAN_POINT ( 'NONE',  ( -96.01551138448773770, -280.4850423649531308, -226.0838409119601238 ) ) ;
#19407 = CARTESIAN_POINT ( 'NONE',  ( -21.63368471006718252, -277.3377947579107854, -341.7661278118835071 ) ) ;
#19408 = CARTESIAN_POINT ( 'NONE',  ( -93.31321642233871216, -288.6295358201517161, -322.7367040332125612 ) ) ;
#19409 = CARTESIAN_POINT ( 'NONE',  ( -83.18774489038943898, -286.2452576912470477, -208.6319767399097316 ) ) ;
#19410 = CARTESIAN_POINT ( 'NONE',  ( -93.38241247716482007, -284.3242155319110793, -323.0963244491782689 ) ) ;
#19411 = CARTESIAN_POINT ( 'NONE',  ( 17.60625775002468529, -282.4045448989123201, -318.4206844552840039 ) ) ;
#19412 = VERTEX_POINT ( 'NONE', #48154 ) ;
#19413 = FACE_OUTER_BOUND ( 'NONE', #84459, .T. ) ;
#19414 = CARTESIAN_POINT ( 'NONE',  ( -102.1714003406963940, -292.9337910870783617, -231.0500252879517973 ) ) ;
#19415 = CARTESIAN_POINT ( 'NONE',  ( -71.93421273947951988, -290.2893545709914065, -202.1069157976611734 ) ) ;
#19416 = CARTESIAN_POINT ( 'NONE',  ( 20.04734331374150003, -273.9705821302050595, -224.8448262857601492 ) ) ;
#19417 = CARTESIAN_POINT ( 'NONE',  ( -69.49287061192910642, -294.8128637054778665, -340.2297741149855028 ) ) ;
#19418 = CARTESIAN_POINT ( 'NONE',  ( -108.0551838024495623, -289.3044209870867007, -249.5724138148768532 ) ) ;
#19419 = B_SPLINE_CURVE_WITH_KNOTS ( 'NONE', 3,
 ( #40560, #83665, #40102, #55282 ),
 .UNSPECIFIED., .F., .F.,
 ( 4, 4 ),
 ( -4.472146915501929662E-06, 0.0002823611672359634833 ),
 .UNSPECIFIED. ) ;
#19420 = CARTESIAN_POINT ( 'NONE',  ( -91.15926689724861376, -294.0695377649434477, -321.2448282055677851 ) ) ;
#19421 = CARTESIAN_POINT ( 'NONE',  ( -82.78013088581576540, -290.8946686732883222, -328.0020714261202670 ) ) ;
#19422 = CARTESIAN_POINT ( 'NONE',  ( 222.4306832106270804, -135.2391364535880882, -21.50000000000000000 ) ) ;
#19423 = CARTESIAN_POINT ( 'NONE',  ( -112.3687964989947545, -292.5770836642851691, -268.4322422422585532 ) ) ;
#19424 = CARTESIAN_POINT ( 'NONE',  ( 18.08151948523178376, -290.8443932915548089, -219.5842024102376229 ) ) ;
#19425 = CARTESIAN_POINT ( 'NONE',  ( -50.54293921849853177, -297.2207659589902846, -344.2423438634703530 ) ) ;
#19426 = CARTESIAN_POINT ( 'NONE',  ( -77.18710288309884504, -286.4451848430729797, -208.8537922480863358 ) ) ;
#19427 = CARTESIAN_POINT ( 'NONE',  ( -4.018081362540677048, -296.6139714307894906, -337.7516691833790219 ) ) ;
#19428 = CARTESIAN_POINT ( 'NONE',  ( 37.09875191467167355, -277.3813898625871843, -258.5723126336488349 ) ) ;
#19429 = CARTESIAN_POINT ( 'NONE',  ( 19.25122274158002966, -297.9409541251399673, -193.5300614419665806 ) ) ;
#19430 = CARTESIAN_POINT ( 'NONE',  ( -26.90041023837674317, -275.1574151874874019, -343.6342609293431565 ) ) ;
#19431 = CARTESIAN_POINT ( 'NONE',  ( -34.22911269578052185, -278.1714037116320242, -195.9734255393522631 ) ) ;
#19432 = CARTESIAN_POINT ( 'NONE',  ( -105.7920830218455137, -274.1109254191138120, -243.7316835570631213 ) ) ;
#19433 = CARTESIAN_POINT ( 'NONE',  ( -96.87449052283102446, -297.3766075508637527, -313.6402403777127574 ) ) ;
#19434 = CARTESIAN_POINT ( 'NONE',  ( 113.5000000000000568, -190.7866584945343220, -490.8867980474134356 ) ) ;
#19435 = CARTESIAN_POINT ( 'NONE',  ( -109.4367199486425193, -297.5188125419746257, -257.9148396508234669 ) ) ;
#19436 = DIRECTION ( 'NONE',  ( -0.000000000000000000, -0.000000000000000000, -1.000000000000000000 ) ) ;
#19438 = CARTESIAN_POINT ( 'NONE',  ( -68.28064516795458871, -273.4674572970430972, -204.2279701918880335 ) ) ;
#19437 = CARTESIAN_POINT ( 'NONE',  ( -36.13893527901843328, -287.0572881008694139, -345.7195534182802703 ) ) ;
#19439 = CARTESIAN_POINT ( 'NONE',  ( -29.46293762432317820, -286.1493411985822490, -193.7652623413481194 ) ) ;
#19440 = CARTESIAN_POINT ( 'NONE',  ( -51.68552784716350601, -288.8975643572458125, -345.9917923006224214 ) ) ;
#19441 = CARTESIAN_POINT ( 'NONE',  ( -112.6667822721557286, -298.5770718032194964, -266.8378753867763749 ) ) ;
#19442 = CARTESIAN_POINT ( 'NONE',  ( -64.25145865080580165, -293.4037719596401530, -340.2436272045648593 ) ) ;
#19443 = CARTESIAN_POINT ( 'NONE',  ( 35.45280807396443379, -281.0616858521780728, -295.1255584212946133 ) ) ;
#19444 = CARTESIAN_POINT ( 'NONE',  ( -37.30987171927208834, -289.5523547857347353, -195.3611179825600175 ) ) ;
#19445 = CARTESIAN_POINT ( 'NONE',  ( 6.539178240135462339, -278.6479185318422651, -209.4745301464643319 ) ) ;
#19446 = CARTESIAN_POINT ( 'NONE',  ( 203.6821298523975088, 287.7126147091306620, -4.992670775290489971 ) ) ;
#19447 = CARTESIAN_POINT ( 'NONE',  ( 14.35221991852950119, -287.1001778936119422, -322.4655240789244885 ) ) ;
#19448 = CARTESIAN_POINT ( 'NONE',  ( -147.8070425842520308, 32.24468615100210656, 22.50000000000000000 ) ) ;
#19449 = CARTESIAN_POINT ( 'NONE',  ( -37.29156836245572038, -287.0513678757959610, -345.3611055862955936 ) ) ;
#19450 = CARTESIAN_POINT ( 'NONE',  ( -55.51011055269275118, -299.4147173743010626, -198.7795694348580184 ) ) ;
#19451 = CARTESIAN_POINT ( 'NONE',  ( 38.69370955966201819, -283.0792144695341790, -278.4380654923639895 ) ) ;
#19453 = CARTESIAN_POINT ( 'NONE',  ( 34.06519705922689667, -281.3513100447460147, -255.1339928361404645 ) ) ;
#19452 = CARTESIAN_POINT ( 'NONE',  ( -59.63686598167379316, -295.7850441338677001, -198.3253160845473531 ) ) ;
#19454 = CARTESIAN_POINT ( 'NONE',  ( -83.57474877046688277, -274.8286870505082220, -213.1083440004505860 ) ) ;
#19455 = CARTESIAN_POINT ( 'NONE',  ( 38.20092394607508623, -285.6113430087452798, -268.7405800503912019 ) ) ;
#19456 = CARTESIAN_POINT ( 'NONE',  ( 35.72316715421460032, -283.3343134517385238, -253.3777033569439254 ) ) ;
#19458 = CARTESIAN_POINT ( 'NONE',  ( -91.34096052969518098, -272.1812701167718842, -220.7612330509709011 ) ) ;
#19457 = AXIS2_PLACEMENT_3D ( 'NONE', #68636, #47286, #83282 ) ;
#19459 = VERTEX_POINT ( 'NONE', #33490 ) ;
#19460 = CARTESIAN_POINT ( 'NONE',  ( 204.4813248545303281, 292.6428223457351692, -53.99999999999219114 ) ) ;
#19461 = CARTESIAN_POINT ( 'NONE',  ( -110.0211405059826575, -286.3118640372304640, -287.4329256685942369 ) ) ;
#19462 = CARTESIAN_POINT ( 'NONE',  ( 36.60358173371529489, -272.6237833571633473, -234.7871824221999191 ) ) ;
#19463 = CARTESIAN_POINT ( 'NONE',  ( -62.36309235902298553, -276.5665669388928904, -343.0677669624786859 ) ) ;
#19464 = CARTESIAN_POINT ( 'NONE',  ( -112.1357604998202078, -289.1370197828583173, -255.7230979849308028 ) ) ;
#19465 = CARTESIAN_POINT ( 'NONE',  ( -102.3740545431648030, -285.6030531752517732, -305.1323425053922165 ) ) ;
#19466 = CARTESIAN_POINT ( 'NONE',  ( 36.44231860042102511, -277.1322467691106795, -268.8252165147472397 ) ) ;
#19467 = CARTESIAN_POINT ( 'NONE',  ( -66.33572811649945322, -284.8496516571270831, -341.0713932220160132 ) ) ;
#19468 = CARTESIAN_POINT ( 'NONE',  ( -7.103839026762195807, -281.4413011762461565, -337.2539166903729893 ) ) ;
#19469 = CARTESIAN_POINT ( 'NONE',  ( -73.10523034926555397, -281.5781949023370885, -204.4371423984183878 ) ) ;
#19470 = CARTESIAN_POINT ( 'NONE',  ( 2.416184001802894610, -274.7362494710105238, -204.4193963336869047 ) ) ;
#19471 = CARTESIAN_POINT ( 'NONE',  ( -7.886600221975030856, -276.5100736484404251, -341.5188989344426318 ) ) ;
#19472 = CARTESIAN_POINT ( 'NONE',  ( -93.25646696972620475, -297.7843342022456454, -319.5022723105683440 ) ) ;
#19473 = DIRECTION ( 'NONE',  ( 0.000000000000000000, 0.000000000000000000, 1.000000000000000000 ) ) ;
#19474 = CARTESIAN_POINT ( 'NONE',  ( 160.5350683151633291, 215.0000000000000568, 25.22542485937379197 ) ) ;
#19475 = CARTESIAN_POINT ( 'NONE',  ( -111.9910846304421881, -294.5233313311862275, -283.6109018952587348 ) ) ;
#19476 = CARTESIAN_POINT ( 'NONE',  ( 25.42523679733339748, -275.5734822009889626, -307.7549686876437818 ) ) ;
#19477 = CARTESIAN_POINT ( 'NONE',  ( -20.60763997381464918, -299.3367160135730387, -193.6672397974564035 ) ) ;
#19478 = CARTESIAN_POINT ( 'NONE',  ( -22.27515888739961980, -288.0077523746222710, -197.8449204549039280 ) ) ;
#19479 = CARTESIAN_POINT ( 'NONE',  ( 35.61833481942879587, -294.7890707294258164, -248.0107029232511593 ) ) ;
#19480 = CARTESIAN_POINT ( 'NONE',  ( 37.03272232231700656, -294.5265677265944646, -252.0184353741070140 ) ) ;
#19481 = EDGE_CURVE ( 'NONE', #15179, #56456, #30608, .T. ) ;
#19482 = CARTESIAN_POINT ( 'NONE',  ( -94.86504419410113087, -293.2149144735826098, -222.4757380611491158 ) ) ;
#19483 = CARTESIAN_POINT ( 'NONE',  ( -2.267823063134530859, -278.5172269377239331, -204.2417290563731740 ) ) ;
#19484 = CARTESIAN_POINT ( 'NONE',  ( -52.13702688884777814, -281.7815889881048292, -197.3534978758159468 ) ) ;
#19485 = CARTESIAN_POINT ( 'NONE',  ( -72.83224060477833461, -293.6059097861643181, -335.8106439962826926 ) ) ;
#19486 = CARTESIAN_POINT ( 'NONE',  ( 0.2759929415788082152, -284.4171896256192440, -336.1424722854899869 ) ) ;
#19487 = CARTESIAN_POINT ( 'NONE',  ( -108.3245363648242972, -283.7133148990215545, -252.0400090034268885 ) ) ;
#19488 = CARTESIAN_POINT ( 'NONE',  ( -93.21478779330486475, -240.8791580765806088, -341.0619996075755012 ) ) ;
#19489 = ORIENTED_EDGE ( 'NONE', *, *, #5821, .T. ) ;
#19490 = CARTESIAN_POINT ( 'NONE',  ( -74.72729022312158520, -285.2062956943942709, -207.6362812747704538 ) ) ;
#19491 = EDGE_LOOP ( 'NONE', ( #51142, #74444, #26389, #9344 ) ) ;
#19492 = CARTESIAN_POINT ( 'NONE',  ( -4.284572199490292554, -283.7062449515055960, -339.5761198286045897 ) ) ;
#19493 = CARTESIAN_POINT ( 'NONE',  ( -27.29146742889274435, -274.5165431070660702, -197.9839973314861368 ) ) ;
#19494 = CARTESIAN_POINT ( 'NONE',  ( 31.07408505274378996, -285.9014066330980199, -235.9040569418474718 ) ) ;
#19495 = CARTESIAN_POINT ( 'NONE',  ( 26.07943445700025364, -281.9201485474387141, -227.0181869501322467 ) ) ;
#19496 = CARTESIAN_POINT ( 'NONE',  ( -74.97723650541998097, -279.0641608532977784, -336.7408901622046073 ) ) ;
#19497 = CARTESIAN_POINT ( 'NONE',  ( -36.76166467069850086, -280.7106732390200818, -193.4522099878877555 ) ) ;
#19498 = CARTESIAN_POINT ( 'NONE',  ( -67.68488546085839630, -277.1237833571632905, -207.2794874003663779 ) ) ;
#19499 = CARTESIAN_POINT ( 'NONE',  ( 175.0256770085078983, 242.8924757603117541, -179.7605988551675580 ) ) ;
#19500 = VERTEX_POINT ( 'NONE', #48624 ) ;
#19501 = CARTESIAN_POINT ( 'NONE',  ( -5.778309749577410059, -276.4682931798193408, -202.5099513130991511 ) ) ;
#19502 = CARTESIAN_POINT ( 'NONE',  ( 179.5181012596348751, 254.3142353492114296, -166.5901205928782645 ) ) ;
#19503 = CARTESIAN_POINT ( 'NONE',  ( -30.07778042622149073, -278.1644878974050812, -196.0191018990759630 ) ) ;
#19504 = CARTESIAN_POINT ( 'NONE',  ( 22.29859497045398342, -294.6738642988329957, -223.2552068712512323 ) ) ;
#19505 = CARTESIAN_POINT ( 'NONE',  ( -53.17953288726015870, -294.6090767794040062, -341.7788244049817195 ) ) ;
#19506 = CARTESIAN_POINT ( 'NONE',  ( -66.98593661265492472, -291.1815266414670873, -199.3629057052757503 ) ) ;
#19507 = DIRECTION ( 'NONE',  ( 0.000000000000000000, 1.000000000000000000, 0.000000000000000000 ) ) ;
#19509 = CARTESIAN_POINT ( 'NONE',  ( 20.12372798844755906, -286.5996363189235012, -316.6662471702024391 ) ) ;
#19508 = CARTESIAN_POINT ( 'NONE',  ( -101.0483277147252466, -295.6864341085647538, -228.1464024302122198 ) ) ;
#19510 = CARTESIAN_POINT ( 'NONE',  ( 36.87787846106154888, -295.4535302682090787, -273.5182665011015501 ) ) ;
#19511 = CARTESIAN_POINT ( 'NONE',  ( -106.0317635033066210, -286.2138949110586736, -244.2284053279668967 ) ) ;
#19512 = ORIENTED_EDGE ( 'NONE', *, *, #38034, .F. ) ;
#19513 = CARTESIAN_POINT ( 'NONE',  ( -109.2576333635352483, -291.8357203872217269, -243.3596399460035684 ) ) ;
#19514 = CARTESIAN_POINT ( 'NONE',  ( 18.54547584344189204, -282.7126212731938040, -317.4402051643497771 ) ) ;
#19515 = CARTESIAN_POINT ( 'NONE',  ( -112.2202928446892116, -295.1439084619268556, -286.5229580100850626 ) ) ;
#19516 = CARTESIAN_POINT ( 'NONE',  ( -97.15791443741044020, -290.7068416908382460, -318.6123459103395703 ) ) ;
#19517 = CARTESIAN_POINT ( 'NONE',  ( -100.6264103876781206, -290.4661746272823848, -314.1169444588870761 ) ) ;
#19518 = CARTESIAN_POINT ( 'NONE',  ( 35.27417659623907298, -287.6201736092147598, -262.8821840977455508 ) ) ;
#19519 = EDGE_LOOP ( 'NONE', ( #82802, #11595, #56209, #58303 ) ) ;
#19520 = DIRECTION ( 'NONE',  ( 0.9167375550253826777, 5.544037366339495023E-15, 0.3994899938747948354 ) ) ;
#19521 = CARTESIAN_POINT ( 'NONE',  ( -65.12808339599854435, -297.2717749781036787, -340.8607280826007013 ) ) ;
#19522 = CARTESIAN_POINT ( 'NONE',  ( -111.7905790197203828, -295.4588520593165413, -252.7354915619162057 ) ) ;
#19523 = CARTESIAN_POINT ( 'NONE',  ( 19.86730956892184352, -279.9670414364985618, -224.6387202057887009 ) ) ;
#19524 = ORIENTED_EDGE ( 'NONE', *, *, #55430, .T. ) ;
#19525 = CARTESIAN_POINT ( 'NONE',  ( 38.12078599941734325, -275.2475281872420965, -285.3591208794525755 ) ) ;
#19526 = CIRCLE ( 'NONE', #28604, 4.999999999999990230 ) ;
#19527 = CARTESIAN_POINT ( 'NONE',  ( -110.7390068134509562, -295.1254274995856122, -263.2133351378632824 ) ) ;
#19528 = CARTESIAN_POINT ( 'NONE',  ( -37.79390056430135303, -278.9182544319880890, -344.6076084687080652 ) ) ;
#19529 = CARTESIAN_POINT ( 'NONE',  ( 36.61092313206808058, -273.6004808806676465, -263.3268763405372965 ) ) ;
#19530 = CARTESIAN_POINT ( 'NONE',  ( -66.19517610796971496, -296.6435585387627043, -337.8489496966423076 ) ) ;
#19531 = CARTESIAN_POINT ( 'NONE',  ( -106.1005258454177778, -297.9711562326219791, -244.7892399344289345 ) ) ;
#19532 = CYLINDRICAL_SURFACE ( 'NONE', #17252, 2.500000000000002220 ) ;
#19533 = CARTESIAN_POINT ( 'NONE',  ( -92.10772536110540898, -297.4187805553817157, -323.3434064864345601 ) ) ;
#19534 = CARTESIAN_POINT ( 'NONE',  ( -94.75772925859425300, -271.2447616858585207, -221.5375050123102767 ) ) ;
#19535 = CARTESIAN_POINT ( 'NONE',  ( -2.397997746604971780, -293.1788268533762221, -206.1376338038719780 ) ) ;
#19536 = CARTESIAN_POINT ( 'NONE',  ( -77.56214637827635272, -290.0753201204041716, -208.7357123471115870 ) ) ;
#19537 = CARTESIAN_POINT ( 'NONE',  ( 207.9918764980109813, 30.19551755111683633, 15.05517478741770532 ) ) ;
#19538 = CARTESIAN_POINT ( 'NONE',  ( 29.89070456516675378, -275.5579666380244817, -232.8439520388284620 ) ) ;
#19539 = CARTESIAN_POINT ( 'NONE',  ( -107.8571847730526230, -297.1364233326436874, -251.3483811165647239 ) ) ;
#19540 = CARTESIAN_POINT ( 'NONE',  ( 19.80198164101667047, -282.8542852446947791, -221.2191436886357394 ) ) ;
#19541 = CARTESIAN_POINT ( 'NONE',  ( 16.88547115480753291, -279.4893537735560471, -216.3172659066114534 ) ) ;
#19542 = CARTESIAN_POINT ( 'NONE',  ( -96.98060673086467887, -277.2482760934615840, -318.9256753709169629 ) ) ;
#19543 = CARTESIAN_POINT ( 'NONE',  ( 35.41795174450378880, -279.6646591839970597, -247.7232409878020576 ) ) ;
#19544 = CARTESIAN_POINT ( 'NONE',  ( 25.69297347687545141, -281.2595026035443766, -307.5992111682854215 ) ) ;
#19545 = CARTESIAN_POINT ( 'NONE',  ( 34.43286967942899679, -279.2646916444378462, -248.0353580658202475 ) ) ;
#19546 = CARTESIAN_POINT ( 'NONE',  ( 13.92001354922727963, -273.3634149119303629, -217.5632806479824239 ) ) ;
#19547 = CARTESIAN_POINT ( 'NONE',  ( -106.8067075046749466, -280.9225857543624443, -241.9483524703122441 ) ) ;
#19548 = DIRECTION ( 'NONE',  ( -0.2456588035076310295, 0.9693563597868428694, 0.000000000000000000 ) ) ;
#19549 = CYLINDRICAL_SURFACE ( 'NONE', #47351, 1.999999999999996003 ) ;
#19550 = CARTESIAN_POINT ( 'NONE',  ( -80.03688364510111342, -295.7232943209882023, -207.4401271544244594 ) ) ;
#19551 = CARTESIAN_POINT ( 'NONE',  ( -53.38931786843857452, -291.8519327235883338, -194.9974311095321582 ) ) ;
#19552 = CARTESIAN_POINT ( 'NONE',  ( 26.11511654838982111, -278.0943193263464082, -310.7476310939799760 ) ) ;
#19553 = CARTESIAN_POINT ( 'NONE',  ( -79.97149403564445436, -271.4756853547752939, -208.5914724473852289 ) ) ;
#19554 = CARTESIAN_POINT ( 'NONE',  ( 193.6552470326849402, 250.5000000000000568, 16.89672165344822119 ) ) ;
#19555 = CARTESIAN_POINT ( 'NONE',  ( -94.23407710033788476, -285.7869239796958141, -320.0860779359610433 ) ) ;
#19556 = CARTESIAN_POINT ( 'NONE',  ( 208.3418117619747818, 38.42745601219717599, 11.99999999999999822 ) ) ;
#19557 = CARTESIAN_POINT ( 'NONE',  ( 37.64557036340986684, -285.5121675678184374, -267.2598578389902286 ) ) ;
#19558 = CARTESIAN_POINT ( 'NONE',  ( 194.5881128153457098, -26.00396092263537540, -47.19625681453479871 ) ) ;
#19559 = CARTESIAN_POINT ( 'NONE',  ( 33.49591756564610989, -292.6000761556006751, -289.6224664639239563 ) ) ;
#19560 = CARTESIAN_POINT ( 'NONE',  ( 26.01708183997713419, -285.1676366962180964, -231.6761050384101566 ) ) ;
#19561 = CARTESIAN_POINT ( 'NONE',  ( -75.31871349344845612, -193.4224457575235192, -358.3059354159982490 ) ) ;
#19562 = CARTESIAN_POINT ( 'NONE',  ( -79.08344145442049467, -293.6145419377324401, -332.7345953412741437 ) ) ;
#19563 = CARTESIAN_POINT ( 'NONE',  ( -82.84675689506562435, -283.9226769932094498, -209.0416881251521488 ) ) ;
#19564 = CARTESIAN_POINT ( 'NONE',  ( -70.11369419273363235, -281.2131257202270262, -204.2227143297434395 ) ) ;
#19565 = CARTESIAN_POINT ( 'NONE',  ( 1.308016098052928067, -287.7614439222979854, -204.2080636061183156 ) ) ;
#19566 = CARTESIAN_POINT ( 'NONE',  ( 3.299190660261174024, -278.8297374877788570, -206.0938766645446663 ) ) ;
#19567 = CARTESIAN_POINT ( 'NONE',  ( -106.0325700772870476, -290.2230626197979291, -295.0707190643522040 ) ) ;
#19568 = CARTESIAN_POINT ( 'NONE',  ( -59.93163074521979183, -281.1790406629697827, -200.2711736610520461 ) ) ;
#19569 = CARTESIAN_POINT ( 'NONE',  ( -16.88634231863705182, -281.1260295508619151, -200.1173989507307169 ) ) ;
#19570 = CARTESIAN_POINT ( 'NONE',  ( -26.87505113223141251, -288.1643779550932436, -195.6839948042730555 ) ) ;
#19571 = VERTEX_POINT ( 'NONE', #61921 ) ;
#19572 = CARTESIAN_POINT ( 'NONE',  ( -26.99651961282917867, -274.1800832024772490, -194.0058057105406988 ) ) ;
#19573 = CARTESIAN_POINT ( 'NONE',  ( -103.0800100968285875, -292.0591761065450669, -305.8305225488045380 ) ) ;
#19574 = FACE_OUTER_BOUND ( 'NONE', #37045, .T. ) ;
#19575 = CARTESIAN_POINT ( 'NONE',  ( 44.71564893372296723, -296.0519495502701943, -270.3284710469131937 ) ) ;
#19576 = ORIENTED_EDGE ( 'NONE', *, *, #5059, .T. ) ;
#19577 = CARTESIAN_POINT ( 'NONE',  ( -38.30767883862273493, -272.0399123529101075, -195.2006542008588212 ) ) ;
#19578 = DIRECTION ( 'NONE',  ( 0.000000000000000000, 0.000000000000000000, 1.000000000000000000 ) ) ;
#19579 = CARTESIAN_POINT ( 'NONE',  ( 0.1291653543521297798, -292.9618621637017100, -336.7265308687156562 ) ) ;
#19580 = CARTESIAN_POINT ( 'NONE',  ( -108.0365170528754959, -272.1483792230273480, -251.5623744590946274 ) ) ;
#19581 = CARTESIAN_POINT ( 'NONE',  ( -61.46386170854030695, -290.8913998111416959, -339.9946520913386507 ) ) ;
#19582 = CARTESIAN_POINT ( 'NONE',  ( -29.31275414760042608, -284.7093371208448502, -343.9888821885774632 ) ) ;
#19583 = CARTESIAN_POINT ( 'NONE',  ( -41.70860172938049715, -290.5313889818283428, -346.6601254359052859 ) ) ;
#19584 = CARTESIAN_POINT ( 'NONE',  ( -43.12818387945036136, -290.4389445989027649, -346.6488291725361250 ) ) ;
#19585 = CARTESIAN_POINT ( 'NONE',  ( 8.119539619085845317, -288.6734769072125459, -210.6442281288526317 ) ) ;
#19586 = CARTESIAN_POINT ( 'NONE',  ( -14.22978131563478854, -280.5103562792286311, -196.8556491659560095 ) ) ;
#19587 = CARTESIAN_POINT ( 'NONE',  ( -105.8708425130099187, -294.2168953295993674, -302.1898917438289800 ) ) ;
#19588 = CARTESIAN_POINT ( 'NONE',  ( -86.10400932912597227, -283.5404450889965915, -329.9533759181841788 ) ) ;
#19589 = CARTESIAN_POINT ( 'NONE',  ( -4.787412233589957822, -276.3459418369423020, -203.6306191924289521 ) ) ;
#19590 = EDGE_CURVE ( 'NONE', #78809, #200, #42457, .T. ) ;
#19591 = CARTESIAN_POINT ( 'NONE',  ( 27.36219212280431989, -278.4805209788416391, -301.4846348637938149 ) ) ;
#19592 = CARTESIAN_POINT ( 'NONE',  ( 38.54379683051755023, -273.7307461590430648, -265.5268812043017306 ) ) ;
#19593 = DIRECTION ( 'NONE',  ( -1.000000000000000000, 0.000000000000000000, 0.000000000000000000 ) ) ;
#19594 = CARTESIAN_POINT ( 'NONE',  ( 35.58166762261365079, -281.0006054385590915, -265.8699179869444720 ) ) ;
#19595 = CARTESIAN_POINT ( 'NONE',  ( -51.22551418447954319, -278.4309355136653608, -345.6953626843069856 ) ) ;
#19596 = AXIS2_PLACEMENT_3D ( 'NONE', #2561, #53195, #87774 ) ;
#19597 = CARTESIAN_POINT ( 'NONE',  ( -105.2184239451338925, -284.0765554432099975, -234.3924822740572438 ) ) ;
#19598 = CARTESIAN_POINT ( 'NONE',  ( -4.401955851565386268, -294.2524402574632632, -204.0676892681283618 ) ) ;
#19599 = CARTESIAN_POINT ( 'NONE',  ( -38.36729687786588272, -275.6396185786705360, -194.1680174449055869 ) ) ;
#19600 = CARTESIAN_POINT ( 'NONE',  ( -92.82613347742224619, -274.5919936852125716, -217.6658532834244681 ) ) ;
#19601 = PLANE ( 'NONE',  #64162 ) ;
#19602 = CARTESIAN_POINT ( 'NONE',  ( -11.25602427284302109, -276.5358373546932853, -338.5413021982215014 ) ) ;
#19603 = CARTESIAN_POINT ( 'NONE',  ( -58.91296420194156980, -297.3320423923565841, -342.0180017439558924 ) ) ;
#19604 = CARTESIAN_POINT ( 'NONE',  ( -70.77931714641178473, -283.6099794526190294, -203.3994268745634884 ) ) ;
#19605 = CARTESIAN_POINT ( 'NONE',  ( 8.841633256664769291, -292.3325536065581218, -208.7085176790063485 ) ) ;
#19606 = CARTESIAN_POINT ( 'NONE',  ( 30.59323416358538594, -273.1629794480649593, -239.3055581775890062 ) ) ;
#19607 = CARTESIAN_POINT ( 'NONE',  ( 29.66898077533889477, -289.6277234983708695, -306.7483626064407076 ) ) ;
#19608 = CARTESIAN_POINT ( 'NONE',  ( 35.95039856128092737, -292.5139160932710638, -273.5159278391927842 ) ) ;
#19609 = ORIENTED_EDGE ( 'NONE', *, *, #77208, .T. ) ;
#19610 = CARTESIAN_POINT ( 'NONE',  ( -40.58907249422940566, -290.5868279356390076, -194.0062991542219493 ) ) ;
#19611 = CARTESIAN_POINT ( 'NONE',  ( -94.12340507806628409, -289.5696727001651425, -316.2732674622867535 ) ) ;
#19612 = EDGE_LOOP ( 'NONE', ( #67245, #6383, #77532, #48990 ) ) ;
#19613 = CARTESIAN_POINT ( 'NONE',  ( 37.20719950797992226, -288.8584859785029266, -288.4153615057131219 ) ) ;
#19614 = CARTESIAN_POINT ( 'NONE',  ( -99.19074347219216747, -278.3484204529441399, -309.2728663125286630 ) ) ;
#19615 = EDGE_CURVE ( 'NONE', #17985, #89903, #91071, .T. ) ;
#19616 = CARTESIAN_POINT ( 'NONE',  ( 6.426266550188667104, -293.3934825830512523, -333.4008727872264899 ) ) ;
#19617 = CARTESIAN_POINT ( 'NONE',  ( -65.84729576893857939, -286.3403113424697608, -198.9274896755308077 ) ) ;
#19618 = CARTESIAN_POINT ( 'NONE',  ( -93.90708481666278828, -285.5971835479311949, -218.0709097067394282 ) ) ;
#19619 = CARTESIAN_POINT ( 'NONE',  ( 34.72511216175007576, -282.0406160159020033, -282.1281079625403549 ) ) ;
#19620 = CARTESIAN_POINT ( 'NONE',  ( 185.4827870066121420, 263.6036262534566958, -153.3731815501813287 ) ) ;
#19621 = CARTESIAN_POINT ( 'NONE',  ( 43.70754100293377320, 12.83641530529500230, -330.7637548252565693 ) ) ;
#19622 = CARTESIAN_POINT ( 'NONE',  ( 101.8919747252719503, 115.3001919161196298, -279.7615209532445419 ) ) ;
#19623 = CARTESIAN_POINT ( 'NONE',  ( 26.78297338306001407, -274.2680019390987241, -235.0329552948199137 ) ) ;
#19624 = CARTESIAN_POINT ( 'NONE',  ( 19.41220318830806590, -275.1269586707234112, -316.7837016143473079 ) ) ;
#19625 = CARTESIAN_POINT ( 'NONE',  ( -97.29444852694773260, -296.7065741132399808, -222.1408435847179419 ) ) ;
#19626 = CARTESIAN_POINT ( 'NONE',  ( -104.5998066112789644, -261.3044276662151333, -315.9010574050290643 ) ) ;
#19627 = CARTESIAN_POINT ( 'NONE',  ( 30.10038376170000518, -274.7081494616471105, -306.5958297535347583 ) ) ;
#19628 = CARTESIAN_POINT ( 'NONE',  ( -59.80422781972996660, -275.5174150529499002, -199.7850559432307591 ) ) ;
#19629 = EDGE_LOOP ( 'NONE', ( #76225, #76329, #50740, #51309, #86118, #58445, #72981, #2536 ) ) ;
#19630 = CARTESIAN_POINT ( 'NONE',  ( -99.73731463604903524, -298.0877647455494071, -225.6441468924830644 ) ) ;
#19631 = CARTESIAN_POINT ( 'NONE',  ( 34.34575610701025994, -288.2312402561335034, -284.5289057701014599 ) ) ;
#19632 = CARTESIAN_POINT ( 'NONE',  ( -94.52455482727145863, -296.6569330555036572, -321.7059550712958753 ) ) ;
#19633 = CARTESIAN_POINT ( 'NONE',  ( -106.4607857110296152, -297.4788059414447048, -236.5664599545320641 ) ) ;
#19634 = CARTESIAN_POINT ( 'NONE',  ( 34.32478059344524723, -293.9020571189629436, -284.2505220560532848 ) ) ;
#19635 = ORIENTED_EDGE ( 'NONE', *, *, #4911, .F. ) ;
#19636 = CARTESIAN_POINT ( 'NONE',  ( 27.25848415957279869, -276.9497656794484897, -231.0676451195035099 ) ) ;
#19637 = ORIENTED_EDGE ( 'NONE', *, *, #84489, .F. ) ;
#19638 = CARTESIAN_POINT ( 'NONE',  ( -19.76418420593281766, -279.7798115852958745, -195.4027331056911123 ) ) ;
#19639 = CARTESIAN_POINT ( 'NONE',  ( -32.39272349485402458, -277.9296210395533535, -343.4791318620034986 ) ) ;
#19640 = CARTESIAN_POINT ( 'NONE',  ( -32.76631449444165156, -275.8691727412134469, -194.4993442762985012 ) ) ;
#19641 = CARTESIAN_POINT ( 'NONE',  ( -74.54654198849124214, -275.5647117204638334, -335.8913136616171187 ) ) ;
#19642 = CARTESIAN_POINT ( 'NONE',  ( -92.82718225066639661, -297.8803225160447710, -222.7471772407489823 ) ) ;
#19643 = CARTESIAN_POINT ( 'NONE',  ( -94.41092623939734096, -294.4743406805955033, -316.8403549952678873 ) ) ;
#19644 = DIRECTION ( 'NONE',  ( 0.000000000000000000, 0.000000000000000000, 1.000000000000000000 ) ) ;
#19645 = CARTESIAN_POINT ( 'NONE',  ( 12.94721008102246174, -281.2250624549287181, -212.1326677795434250 ) ) ;
#19646 = CARTESIAN_POINT ( 'NONE',  ( 3.135869998262936331, -276.6581652179443722, -331.1111494324139812 ) ) ;
#19647 = CARTESIAN_POINT ( 'NONE',  ( 38.86506681061069202, -286.1445945879853525, -263.0213388523831668 ) ) ;
#19648 = CARTESIAN_POINT ( 'NONE',  ( -108.2203180557378772, -274.8696739446943411, -245.8412858368496927 ) ) ;
#19649 = CARTESIAN_POINT ( 'NONE',  ( 82.68073018288104947, -297.0543924324409204, -195.4120394483015559 ) ) ;
#19650 = CARTESIAN_POINT ( 'NONE',  ( 14.18988546296487741, -287.5023562168280478, -322.2947045452755219 ) ) ;
#19651 = CARTESIAN_POINT ( 'NONE',  ( 22.15676834298203701, -279.1830263801064120, -226.3181223125586428 ) ) ;
#19653 = CARTESIAN_POINT ( 'NONE',  ( -89.92853646524764599, -281.8811752907210462, -323.1206733906225850 ) ) ;
#19652 = CARTESIAN_POINT ( 'NONE',  ( -36.98741841384914864, -278.6314003859331478, -196.7727397997874448 ) ) ;
#19654 = CARTESIAN_POINT ( 'NONE',  ( -14.24238930478394849, -288.3517357250240138, -198.9533476307918249 ) ) ;
#19655 = CARTESIAN_POINT ( 'NONE',  ( -108.1996132146635432, -279.5057944259626765, -289.4997349308646903 ) ) ;
#19656 = FACE_OUTER_BOUND ( 'NONE', #47790, .T. ) ;
#19657 = CARTESIAN_POINT ( 'NONE',  ( -72.51880510702238780, -293.5867174665395964, -204.1078535119520438 ) ) ;
#19658 = CARTESIAN_POINT ( 'NONE',  ( -92.61253242368304939, -276.0698836054360186, -322.5817248135517730 ) ) ;
#19659 = VECTOR ( 'NONE', #27927, 1000.000000000000000 ) ;
#19660 = CARTESIAN_POINT ( 'NONE',  ( -5.013548982505705354, -277.2663799546780297, -335.9401358482916748 ) ) ;
#19661 = CARTESIAN_POINT ( 'NONE',  ( 18.44050481977730982, -284.2537714581124533, -320.8195784446700145 ) ) ;
#19662 = CARTESIAN_POINT ( 'NONE',  ( 196.3789471156757713, 71.92880008233049693, 11.42127566691390683 ) ) ;
#19663 = CARTESIAN_POINT ( 'NONE',  ( -111.2369507814203757, -292.6740740063152657, -254.5263891447043818 ) ) ;
#19664 = CARTESIAN_POINT ( 'NONE',  ( -103.6660590602784850, -295.0174025927381081, -235.2361043553986804 ) ) ;
#19665 = CARTESIAN_POINT ( 'NONE',  ( -100.8572357993364363, -284.3218524460170897, -227.0243940207085700 ) ) ;
#19666 = CARTESIAN_POINT ( 'NONE',  ( 198.1329898669366969, 69.92583464099143953, 8.330337636095686449 ) ) ;
#19667 = CARTESIAN_POINT ( 'NONE',  ( -81.35302854835673259, -272.1246130319072449, -211.4394216006893430 ) ) ;
#19668 = CARTESIAN_POINT ( 'NONE',  ( -36.16315086508631538, -290.2066310600814063, -196.1225827854780732 ) ) ;
#19669 = CARTESIAN_POINT ( 'NONE',  ( 195.4781563537916043, 39.36132622696000283, 15.00000000000000000 ) ) ;
#19670 = CARTESIAN_POINT ( 'NONE',  ( 208.4306832106270804, -198.2391364535880598, 0.000000000000000000 ) ) ;
#19671 = CARTESIAN_POINT ( 'NONE',  ( -66.73036770220565472, -290.1539178826674288, -199.9408512141963001 ) ) ;
#19672 = CARTESIAN_POINT ( 'NONE',  ( 38.33619385700066573, -285.8787378740418035, -277.2043901635170755 ) ) ;
#19673 = EDGE_CURVE ( 'NONE', #4825, #65856, #7967, .T. ) ;
#19674 = CARTESIAN_POINT ( 'NONE',  ( -110.9799068465407856, -285.9699637215548478, -270.9318380093532710 ) ) ;
#19675 = CARTESIAN_POINT ( 'NONE',  ( -71.26214713705579129, -286.3950412505004124, -205.5382439172087743 ) ) ;
#19676 = CARTESIAN_POINT ( 'NONE',  ( -22.54204002674223162, -294.2204577724324395, -196.4203591817009169 ) ) ;
#19677 = CARTESIAN_POINT ( 'NONE',  ( -7.172545680384787126, -274.7393621255194489, -339.6509040317794756 ) ) ;
#19678 = CARTESIAN_POINT ( 'NONE',  ( 36.56436033103000227, -275.6132200038420024, -248.6426118559175507 ) ) ;
#19679 = CARTESIAN_POINT ( 'NONE',  ( -25.22775416250377134, -290.2852867372482137, -195.7785026567699447 ) ) ;
#19680 = CARTESIAN_POINT ( 'NONE',  ( -107.4191222988419696, -278.9614488591267332, -238.3242045949060923 ) ) ;
#19681 = CARTESIAN_POINT ( 'NONE',  ( -104.2311226638829709, -298.0914451866808577, -303.6086752717274067 ) ) ;
#19682 = CARTESIAN_POINT ( 'NONE',  ( -43.53082020000776708, -249.2392102346787510, -481.7612224915185948 ) ) ;
#19683 = LINE ( 'NONE', #42386, #5754 ) ;
#19684 = CARTESIAN_POINT ( 'NONE',  ( -94.49505170464325943, -283.8862425032945680, -224.1379548612009671 ) ) ;
#19685 = CARTESIAN_POINT ( 'NONE',  ( -7.015099983241920079, -278.4498802124176109, -201.7520392936258702 ) ) ;
#19686 = CARTESIAN_POINT ( 'NONE',  ( 200.4738562182569694, 293.9636489450776367, -44.00000000000000000 ) ) ;
#19687 = CARTESIAN_POINT ( 'NONE',  ( -21.47985050700745546, -272.7318698313854952, -195.7212527797362611 ) ) ;
#19688 = CARTESIAN_POINT ( 'NONE',  ( -85.17820155550340644, -277.0817093105747517, -325.7053148123472965 ) ) ;
#19689 = CARTESIAN_POINT ( 'NONE',  ( 8.676076768217118484, -295.9287765001250250, -327.9860053392569625 ) ) ;
#19690 = CARTESIAN_POINT ( 'NONE',  ( 37.95382898646369085, -280.2896231767836639, -255.7982952493898949 ) ) ;
#19691 = CARTESIAN_POINT ( 'NONE',  ( 18.15855984532634793, -295.1718741233734136, -318.1623481909813336 ) ) ;
#19692 = CARTESIAN_POINT ( 'NONE',  ( -88.26462543217742507, -297.0626568651287016, -327.5299037707362118 ) ) ;
#19693 = CARTESIAN_POINT ( 'NONE',  ( -35.14562830694016071, -297.9137171610188943, -197.3611822273222458 ) ) ;
#19694 = CARTESIAN_POINT ( 'NONE',  ( -112.2446338966031192, -292.6130086750177952, -265.6342764491004118 ) ) ;
#19695 = CARTESIAN_POINT ( 'NONE',  ( -4.775876822855616766, -286.6360087948301612, -200.5867161077590026 ) ) ;
#19696 = CARTESIAN_POINT ( 'NONE',  ( 32.58286245647676083, -273.3131932041474670, -241.0559906015652700 ) ) ;
#19697 = CARTESIAN_POINT ( 'NONE',  ( -36.08897095696743662, -288.8702068675487453, -347.3640372530098261 ) ) ;
#19698 = CARTESIAN_POINT ( 'NONE',  ( -24.62031947533433396, -282.1951881461678795, -196.8083255521464423 ) ) ;
#19699 = EDGE_CURVE ( 'NONE', #33474, #34201, #91715, .T. ) ;
#19700 = CARTESIAN_POINT ( 'NONE',  ( -30.49739542974624129, -285.1994256252635296, -197.3953836105832806 ) ) ;
#19701 = CARTESIAN_POINT ( 'NONE',  ( -83.02736304058474559, -289.4271986102591541, -210.8160960141771909 ) ) ;
#19702 = CARTESIAN_POINT ( 'NONE',  ( 198.7213489544213303, 274.9184959104715631, -125.0903475807052416 ) ) ;
#19703 = CARTESIAN_POINT ( 'NONE',  ( -10.72171321864602156, -285.9165616421683467, -202.3081449986320024 ) ) ;
#19704 = DIRECTION ( 'NONE',  ( -1.000000000000000000, 0.000000000000000000, 0.000000000000000000 ) ) ;
#19705 = CARTESIAN_POINT ( 'NONE',  ( 37.63830155107445563, -282.7006045018844702, -286.8784615048901969 ) ) ;
#19706 = CARTESIAN_POINT ( 'NONE',  ( -114.0168623531891967, -289.5644021979895228, -274.0678294754696935 ) ) ;
#19707 = CARTESIAN_POINT ( 'NONE',  ( -42.39753414699718093, -281.5895124599226733, -194.3290263488046321 ) ) ;
#19708 = CARTESIAN_POINT ( 'NONE',  ( -99.85575994222260476, -280.4546632004311846, -226.2556693533755094 ) ) ;
#19709 = CARTESIAN_POINT ( 'NONE',  ( 34.06564199394210846, -281.1846570255385132, -255.1360791399640675 ) ) ;
#19710 = CARTESIAN_POINT ( 'NONE',  ( 23.07765528434189051, -276.9462939751554131, -225.9257475807246465 ) ) ;
#19711 = CARTESIAN_POINT ( 'NONE',  ( -41.94556103032653027, -295.1085237700092421, -347.2757548767604590 ) ) ;
#19712 = CARTESIAN_POINT ( 'NONE',  ( -82.70917201603603530, -289.4491225278515003, -211.0197694380165387 ) ) ;
#19713 = CARTESIAN_POINT ( 'NONE',  ( -71.79818029325973328, -296.5058242797296089, -205.6400064961015630 ) ) ;
#19714 = VERTEX_POINT ( 'NONE', #26868 ) ;
#19715 = VERTEX_POINT ( 'NONE', #49112 ) ;
#19716 = CARTESIAN_POINT ( 'NONE',  ( -79.16589712348211094, -285.5414983966610976, -331.9407472564299155 ) ) ;
#19717 = CARTESIAN_POINT ( 'NONE',  ( -110.1206748168517606, -296.1326706596463509, -276.8973139176134168 ) ) ;
#19718 = CARTESIAN_POINT ( 'NONE',  ( 30.61860236383399680, -294.1701763916955201, -234.7096720974109871 ) ) ;
#19719 = CARTESIAN_POINT ( 'NONE',  ( -78.42707957339293046, -284.2729618792450310, -330.8250267528971449 ) ) ;
#19720 = ADVANCED_FACE ( 'NONE', ( #20703 ), #78009, .T. ) ;
#19721 = CARTESIAN_POINT ( 'NONE',  ( 21.67766519286977811, -273.9486810173527260, -221.2741061470665329 ) ) ;
#19722 = CARTESIAN_POINT ( 'NONE',  ( -72.13357699223674047, -292.2556236867211510, -201.7692956589353912 ) ) ;
#19723 = CARTESIAN_POINT ( 'NONE',  ( -112.9178208589332115, -282.7684858132503791, -264.3227084533477296 ) ) ;
#19724 = AXIS2_PLACEMENT_3D ( 'NONE', #25062, #24581, #53469 ) ;
#19725 = CARTESIAN_POINT ( 'NONE',  ( -39.21543250222599397, -292.3625520495683645, -193.3920377942747280 ) ) ;
#19726 = CARTESIAN_POINT ( 'NONE',  ( 33.10343484458137198, -288.1415686587847063, -289.7730104989897200 ) ) ;
#19727 = DIRECTION ( 'NONE',  ( -0.000000000000000000, -0.000000000000000000, -1.000000000000000000 ) ) ;
#19728 = CARTESIAN_POINT ( 'NONE',  ( 144.2857639756989272, -299.5541904835127980, -195.3611179825600175 ) ) ;
#19729 = CARTESIAN_POINT ( 'NONE',  ( 138.7881348363077052, 178.2172623047512161, -238.2660695523903485 ) ) ;
#19730 = AXIS2_PLACEMENT_3D ( 'NONE', #46573, #17255, #75017 ) ;
#19731 = CARTESIAN_POINT ( 'NONE',  ( 21.09167699642706140, -283.7390007671057788, -319.4350233954951364 ) ) ;
#19732 = CARTESIAN_POINT ( 'NONE',  ( 31.95455697924147032, -285.4809262143061801, -303.7686719486574702 ) ) ;
#19733 = VERTEX_POINT ( 'NONE', #71368 ) ;
#19734 = CARTESIAN_POINT ( 'NONE',  ( 23.94849149654265119, -279.9161214585595872, -230.0484276068459621 ) ) ;
#19735 = CARTESIAN_POINT ( 'NONE',  ( -59.66293500783951487, -277.0003116746102592, -344.0327323594311224 ) ) ;
#19736 = CARTESIAN_POINT ( 'NONE',  ( -97.09054081448391571, -281.1699180687517696, -225.2831583572297234 ) ) ;
#19737 = CARTESIAN_POINT ( 'NONE',  ( -45.92068160576775426, -156.1269989744705526, -363.0336626541780447 ) ) ;
#19738 = CARTESIAN_POINT ( 'NONE',  ( 37.84251794672265845, -280.2996511457330939, -284.0696689086099127 ) ) ;
#19739 = CARTESIAN_POINT ( 'NONE',  ( -107.0931480392117976, -282.9193594679904891, -243.7795018716523430 ) ) ;
#19740 = CARTESIAN_POINT ( 'NONE',  ( -92.93686599548415472, -299.0284833316845834, -218.4851962741639113 ) ) ;
#19741 = CARTESIAN_POINT ( 'NONE',  ( 29.90993719255589767, -293.6599345157313223, -241.6799036520421566 ) ) ;
#19742 = VERTEX_POINT ( 'NONE', #33977 ) ;
#19743 = CARTESIAN_POINT ( 'NONE',  ( -97.15301100410968616, -289.8306929644076604, -227.5684999561558470 ) ) ;
#19744 = CARTESIAN_POINT ( 'NONE',  ( -38.53504745781614815, -277.7181572635600446, -347.2499254203794408 ) ) ;
#19745 = CARTESIAN_POINT ( 'NONE',  ( -110.3417001280813707, -272.5521521680024648, -270.3611179825603585 ) ) ;
#19746 = ORIENTED_EDGE ( 'NONE', *, *, #67912, .F. ) ;
#19747 = CARTESIAN_POINT ( 'NONE',  ( -60.76358233746753257, -272.6756696795112020, -197.2789531441635802 ) ) ;
#19748 = CARTESIAN_POINT ( 'NONE',  ( 152.4536156746142410, 0.000000000000000000, -12.50000000000000000 ) ) ;
#19749 = LINE ( 'NONE', #49566, #47581 ) ;
#19750 = EDGE_CURVE ( 'NONE', #30016, #53974, #10520, .T. ) ;
#19751 = CARTESIAN_POINT ( 'NONE',  ( 129.4467878515196162, -299.5541904835127980, -198.3997165823495550 ) ) ;
#19752 = CARTESIAN_POINT ( 'NONE',  ( -10.85129343070491892, -283.7782516955888354, -338.7705037227991056 ) ) ;
#19753 = CARTESIAN_POINT ( 'NONE',  ( 25.43068128015184470, -282.7389056369913760, -227.4487645885667746 ) ) ;
#19754 = CARTESIAN_POINT ( 'NONE',  ( -108.3242324399501229, -283.3737599452003906, -288.3857831769414020 ) ) ;
#19755 = CARTESIAN_POINT ( 'NONE',  ( -32.91259614913970211, -281.9689674292251880, -196.2581590718765767 ) ) ;
#19756 = CARTESIAN_POINT ( 'NONE',  ( 17.02974745033863968, -274.7391166311875850, -320.1238118355374809 ) ) ;
#19757 = CARTESIAN_POINT ( 'NONE',  ( 175.2296996224750103, 142.2541816238762920, -24.00000000000001066 ) ) ;
#19758 = CARTESIAN_POINT ( 'NONE',  ( 36.00835036207486439, -276.6477944451348776, -271.5764282949344306 ) ) ;
#19759 = CARTESIAN_POINT ( 'NONE',  ( 194.3811518219889649, 40.34787838408796290, 14.46471776229852679 ) ) ;
#19760 = CARTESIAN_POINT ( 'NONE',  ( -99.51307849737928279, -278.7543702694639478, -315.5374298997721780 ) ) ;
#19761 = EDGE_LOOP ( 'NONE', ( #31495, #72178, #26521, #82940 ) ) ;
#19762 = ORIENTED_EDGE ( 'NONE', *, *, #42341, .T. ) ;
#19763 = DIRECTION ( 'NONE',  ( -1.000000000000000000, 0.000000000000000000, 0.000000000000000000 ) ) ;
#19764 = CARTESIAN_POINT ( 'NONE',  ( -68.02263366361404451, -287.5140618410572415, -201.0722573994112281 ) ) ;
#19765 = CARTESIAN_POINT ( 'NONE',  ( 12.45731938454958332, -293.5344078923220650, -324.0277401862096553 ) ) ;
#19766 = CARTESIAN_POINT ( 'NONE',  ( -6.967832638906750198, -288.0125230783871757, -341.0205149338335104 ) ) ;
#19767 = CARTESIAN_POINT ( 'NONE',  ( -90.37349702975336641, -283.5291129654755196, -218.6581220524021205 ) ) ;
#19769 = CARTESIAN_POINT ( 'NONE',  ( -18.23320475851627620, -287.0425047312920128, -341.9185511184355164 ) ) ;
#19768 = CARTESIAN_POINT ( 'NONE',  ( -106.7353939726693426, -282.8017453815176623, -295.0056244869351758 ) ) ;
#19770 = CARTESIAN_POINT ( 'NONE',  ( -89.16383424396659052, -285.0059014523712904, -322.4093275085817822 ) ) ;
#19771 = CARTESIAN_POINT ( 'NONE',  ( 37.70584845660003737, -273.5624502577534827, -271.1760116059775214 ) ) ;
#19772 = CARTESIAN_POINT ( 'NONE',  ( 35.09498239607010817, -285.6494295133321089, -246.5412806311888403 ) ) ;
#19773 = CARTESIAN_POINT ( 'NONE',  ( -10.04654659474507916, -300.3939934521641248, -195.3518037847966866 ) ) ;
#19774 = CARTESIAN_POINT ( 'NONE',  ( -46.26204850434202598, -283.9390585778286322, -195.7256317173185778 ) ) ;
#19775 = CARTESIAN_POINT ( 'NONE',  ( -11.67186913108536217, -281.3359232788729400, -201.7183662783044724 ) ) ;
#19776 = CARTESIAN_POINT ( 'NONE',  ( 27.33943558787691686, -290.0633536414809441, -308.6544477817870415 ) ) ;
#19777 = FACE_OUTER_BOUND ( 'NONE', #4816, .T. ) ;
#19778 = CARTESIAN_POINT ( 'NONE',  ( 195.9119638496091227, 40.72287714413864990, 13.40410220951428855 ) ) ;
#19779 = CARTESIAN_POINT ( 'NONE',  ( -44.63188582019119366, -297.0637387576827564, -345.6210205169334131 ) ) ;
#19780 =( BOUNDED_SURFACE ( )  B_SPLINE_SURFACE ( 3, 2, ( 
 ( #46821, #83280, #48699 ),
 ( #70517, #76201, #18424 ),
 ( #5644, #40640, #54407 ),
 ( #12754, #27412, #61540 ),
 ( #63426, #19365, #25528 ),
 ( #92255, #75723, #82817 ) ),
 .UNSPECIFIED., .F., .F., .F. ) 
 B_SPLINE_SURFACE_WITH_KNOTS ( ( 4, 2, 4 ),
 ( 3, 3 ),
 ( 5.756444938927698374, 6.019815123053642303, 6.283185307179586232 ),
 ( 0.000000000000000000, 1.000000000000000000 ),
 .UNSPECIFIED. ) 
 GEOMETRIC_REPRESENTATION_ITEM ( )  RATIONAL_B_SPLINE_SURFACE ( (
 ( 1.000000000000000000, 0.9186651033962672797, 1.000000000000000000),
 ( 1.000000000000000000, 0.9282241625911038518, 1.000000000000000000),
 ( 1.000000000000000000, 0.9354614375524440417, 1.000000000000000000),
 ( 1.000000000000000000, 0.9451322790882566993, 1.000000000000000000),
 ( 1.000000000000000000, 0.9475658968924186576, 1.000000000000000000),
 ( 1.000000000000000000, 0.9475641245298915827, 1.000000000000000000) ) ) 
 REPRESENTATION_ITEM ( '' )  SURFACE ( )  );
#19781 = CARTESIAN_POINT ( 'NONE',  ( -88.88717499401114708, -277.3284010007266716, -215.8094222756787985 ) ) ;
#19782 = CARTESIAN_POINT ( 'NONE',  ( -84.15985010224790130, -290.6243338587401013, -209.3660776980017886 ) ) ;
#19783 = CARTESIAN_POINT ( 'NONE',  ( 12.88457774571210557, -292.7372404654198590, -324.5029587064720999 ) ) ;
#19784 = CARTESIAN_POINT ( 'NONE',  ( -93.45596567768583895, -277.9071474005312439, -222.8819648695211129 ) ) ;
#19785 = CARTESIAN_POINT ( 'NONE',  ( -36.44134323252146856, -296.2031237266695598, -196.1261993992958423 ) ) ;
#19786 = CARTESIAN_POINT ( 'NONE',  ( 27.60164628934830944, -295.3341227589655205, -304.8734753598757266 ) ) ;
#19787 = CARTESIAN_POINT ( 'NONE',  ( 21.31550574532285580, -296.6948066931273615, -317.0979686699210447 ) ) ;
#19788 = CARTESIAN_POINT ( 'NONE',  ( -109.1914579710964688, -295.3593595955787805, -244.6644246220234891 ) ) ;
#19790 = CARTESIAN_POINT ( 'NONE',  ( 18.68388157314336340, -291.0843738005387422, -219.0278129147083916 ) ) ;
#19789 =( BOUNDED_CURVE ( )  B_SPLINE_CURVE ( 3, ( #1518, #2467, #23301, #67336 ),
 .UNSPECIFIED., .F., .F. ) 
 B_SPLINE_CURVE_WITH_KNOTS ( ( 4, 4 ),
 ( 0.000000000000000000, 0.2609887789853130857 ),
 .UNSPECIFIED. ) 
 CURVE ( )  GEOMETRIC_REPRESENTATION_ITEM ( )  RATIONAL_B_SPLINE_CURVE ( ( 1.000000000000000000, 0.9943317885200935180, 0.9943317885200935180, 1.000000000000000000 ) ) 
 REPRESENTATION_ITEM ( '' )  );
#19791 = EDGE_CURVE ( 'NONE', #81769, #68679, #18579, .T. ) ;
#19792 = CARTESIAN_POINT ( 'NONE',  ( -82.10171122319502501, -292.8537390999568402, -211.8850126452549603 ) ) ;
#19793 = CARTESIAN_POINT ( 'NONE',  ( 159.4851178187871312, 15.00000000000000000, 9.000000000000000000 ) ) ;
#19794 = CARTESIAN_POINT ( 'NONE',  ( -99.85487640567964718, -291.8773005092447761, -232.3518491338498109 ) ) ;
#19795 = CARTESIAN_POINT ( 'NONE',  ( 133.0872704186301405, -299.5541904835127980, -201.5153591320744226 ) ) ;
#19796 = CARTESIAN_POINT ( 'NONE',  ( -92.53669015439579937, -292.4888117153999474, -217.1676380539473143 ) ) ;
#19798 = CARTESIAN_POINT ( 'NONE',  ( 32.62907988878000509, -293.2746562634193310, -249.3761161526255705 ) ) ;
#19797 = CARTESIAN_POINT ( 'NONE',  ( 22.08979908418054805, -280.2049567537261510, -316.7101787175686809 ) ) ;
#19799 = CARTESIAN_POINT ( 'NONE',  ( 38.25468745361011713, -281.3691200323804651, -255.7260168691857700 ) ) ;
#19800 = CIRCLE ( 'NONE', #62184, 25.00000000000000355 ) ;
#19801 = CARTESIAN_POINT ( 'NONE',  ( -74.26957379479510735, -283.1956220999660445, -337.9637400062198367 ) ) ;
#19802 = CARTESIAN_POINT ( 'NONE',  ( -45.58917951545137015, -287.1567656722282322, -344.7385843906310470 ) ) ;
#19803 = CARTESIAN_POINT ( 'NONE',  ( -21.14134750837864374, -280.9818320128409255, -342.8599463161110066 ) ) ;
#19804 = CARTESIAN_POINT ( 'NONE',  ( -22.68025812134403196, -278.7162612770173951, -195.4224380181877052 ) ) ;
#19805 = CARTESIAN_POINT ( 'NONE',  ( -1.103432937216531462, -285.4419472342749486, -202.7720619055572229 ) ) ;
#19806 = CARTESIAN_POINT ( 'NONE',  ( 196.5083371989332761, 41.97678070738544420, 13.12846593433875775 ) ) ;
#19807 = CARTESIAN_POINT ( 'NONE',  ( 31.56818299172082476, -294.8032841239700019, -243.9439186182547417 ) ) ;
#19808 = CARTESIAN_POINT ( 'NONE',  ( 22.28705372150622566, -276.3322010358536431, -222.5594381705689955 ) ) ;
#19809 = CARTESIAN_POINT ( 'NONE',  ( -78.64745811923552310, -277.2919877065582455, -330.6383188499635821 ) ) ;
#19810 = CARTESIAN_POINT ( 'NONE',  ( -109.8648345067316967, -290.3904830862032895, -296.3918474323584178 ) ) ;
#19811 = CARTESIAN_POINT ( 'NONE',  ( -85.20936181462374748, -281.7872532658637965, -328.8247918306738597 ) ) ;
#19812 = EDGE_CURVE ( 'NONE', #89567, #46866, #18839, .T. ) ;
#19813 = CARTESIAN_POINT ( 'NONE',  ( 20.70238336388817402, -293.2376174111251999, -315.0391521586855106 ) ) ;
#19814 = CARTESIAN_POINT ( 'NONE',  ( -99.86788536775441116, -295.1116386565533389, -228.9194289742398212 ) ) ;
#19815 = EDGE_LOOP ( 'NONE', ( #91912, #51590, #66215, #10760 ) ) ;
#19816 = DIRECTION ( 'NONE',  ( -0.4999999999999952260, -0.8660254037844413721, 0.000000000000000000 ) ) ;
#19817 = CARTESIAN_POINT ( 'NONE',  ( -44.29982926479985395, -291.4695650077200071, -197.5808075477365833 ) ) ;
#19818 = DIRECTION ( 'NONE',  ( 0.000000000000000000, 0.000000000000000000, -1.000000000000000000 ) ) ;
#19819 = CARTESIAN_POINT ( 'NONE',  ( -67.74223827176246004, -280.9809262143061233, -333.4151289067050357 ) ) ;
#19820 = CARTESIAN_POINT ( 'NONE',  ( -112.9741625675555809, -295.4423467957212210, -283.7976215715974604 ) ) ;
#19821 = CARTESIAN_POINT ( 'NONE',  ( 38.29441365000484154, -279.7583168382161602, -275.5994865863074779 ) ) ;
#19822 = CARTESIAN_POINT ( 'NONE',  ( 11.74824306526563511, -288.0322077725974736, -211.6108641715086378 ) ) ;
#19823 = CARTESIAN_POINT ( 'NONE',  ( 30.97534841185867549, -287.0404763278103246, -244.4933101193268499 ) ) ;
#19824 = CARTESIAN_POINT ( 'NONE',  ( -35.07711795261460708, -278.5433253358024217, -344.0196505608382722 ) ) ;
#19825 = CARTESIAN_POINT ( 'NONE',  ( -110.0741409595411255, -294.7888458145322943, -253.5730609785514105 ) ) ;
#19826 = CARTESIAN_POINT ( 'NONE',  ( -106.9324130441769398, -297.9793987867762439, -295.7130125659959958 ) ) ;
#19827 = CARTESIAN_POINT ( 'NONE',  ( -109.5198074835607258, -277.5218494093459753, -257.0400322831028461 ) ) ;
#19828 = ORIENTED_EDGE ( 'NONE', *, *, #17386, .F. ) ;
#19829 = LINE ( 'NONE', #49645, #69747 ) ;
#19830 = CARTESIAN_POINT ( 'NONE',  ( -113.6322613052279706, -296.0854973759957147, -281.0227273243137347 ) ) ;
#19831 = CARTESIAN_POINT ( 'NONE',  ( -100.0417524746999050, -291.9279981651594085, -310.4861430031413647 ) ) ;
#19832 = CARTESIAN_POINT ( 'NONE',  ( 202.7117753844581500, 291.9766168559941661, -53.99999999997706368 ) ) ;
#19833 = CARTESIAN_POINT ( 'NONE',  ( -21.09863385626011123, -289.4896033134440927, -341.6356258090864912 ) ) ;
#19834 = VERTEX_POINT ( 'NONE', #19757 ) ;
#19835 = CARTESIAN_POINT ( 'NONE',  ( 21.79712709136077109, -279.9509789798811994, -221.4180967335175865 ) ) ;
#19836 = CARTESIAN_POINT ( 'NONE',  ( -97.32270926352100560, -296.5577274728772750, -318.5025463817614764 ) ) ;
#19837 = CARTESIAN_POINT ( 'NONE',  ( -87.80879734104286172, -289.4951983790995200, -213.8511403055622395 ) ) ;
#19838 = CARTESIAN_POINT ( 'NONE',  ( -97.33253926625397412, -297.5320688180210027, -222.1237516451573129 ) ) ;
#19839 = CARTESIAN_POINT ( 'NONE',  ( 33.32759624862482895, -293.6428072252660968, -251.9780269348134709 ) ) ;
#19840 = SURFACE_STYLE_USAGE ( .BOTH. , #26949 ) ;
#19841 = DIRECTION ( 'NONE',  ( -0.000000000000000000, 0.000000000000000000, -1.000000000000000000 ) ) ;
#19842 = CARTESIAN_POINT ( 'NONE',  ( 20.97180904886876718, -289.7413038712097091, -319.5773998617260077 ) ) ;
#19843 = CARTESIAN_POINT ( 'NONE',  ( -2.602324593224680793, -279.1233781216987495, -342.4248175857292154 ) ) ;
#19844 = VERTEX_POINT ( 'NONE', #69486 ) ;
#19845 = CARTESIAN_POINT ( 'NONE',  ( 37.23443169202002423, -280.6657830660437867, -251.6070957540618735 ) ) ;
#19846 = CARTESIAN_POINT ( 'NONE',  ( -111.2354060202307977, -286.7054854840063172, -258.4582456560783044 ) ) ;
#19847 = CARTESIAN_POINT ( 'NONE',  ( 38.09030551851898849, -286.2845723372089424, -282.8732652393977673 ) ) ;
#19848 = CARTESIAN_POINT ( 'NONE',  ( -75.17890104189361011, -271.5469468727137610, -205.7381509177145915 ) ) ;
#19849 = CARTESIAN_POINT ( 'NONE',  ( -72.61116682373119602, -275.5019396621260626, -204.7492781176285348 ) ) ;
#19850 = CARTESIAN_POINT ( 'NONE',  ( -96.23902366933627661, -289.2605802766945544, -224.8372837746817083 ) ) ;
#19851 = CARTESIAN_POINT ( 'NONE',  ( -112.9791290467273654, -280.4683850981388673, -265.9696689317390792 ) ) ;
#19852 = ORIENTED_EDGE ( 'NONE', *, *, #89992, .T. ) ;
#19854 = CARTESIAN_POINT ( 'NONE',  ( 19.76083203576745362, -280.2568332731972305, -224.7191034666850271 ) ) ;
#19853 = CARTESIAN_POINT ( 'NONE',  ( 17.96452820155933594, -280.8733720385426977, -222.6950921471296283 ) ) ;
#19855 = CARTESIAN_POINT ( 'NONE',  ( -22.98323590571796160, -277.9524078404988927, -345.7498532214596025 ) ) ;
#19856 = CARTESIAN_POINT ( 'NONE',  ( -113.9878542064895584, -277.3316714146322397, -271.5866485534946264 ) ) ;
#19857 = CARTESIAN_POINT ( 'NONE',  ( -14.28501004054799317, -91.24624836385295623, -357.5043840972602425 ) ) ;
#19858 = CARTESIAN_POINT ( 'NONE',  ( -113.6301709903047339, -273.6005026173463648, -261.8235875350928268 ) ) ;
#19859 = ADVANCED_FACE ( 'NONE', ( #34904 ), #20075, .T. ) ;
#19860 = CARTESIAN_POINT ( 'NONE',  ( -113.4905809247468369, -274.1437518858514295, -264.6971630283529180 ) ) ;
#19861 = CARTESIAN_POINT ( 'NONE',  ( -20.25526795762937127, -282.7662352645560304, -195.3538533559490702 ) ) ;
#19862 = CARTESIAN_POINT ( 'NONE',  ( 82.63534306898570492, -300.6190880219792234, -193.0924700335917237 ) ) ;
#19863 = AXIS2_PLACEMENT_3D ( 'NONE', #10737, #39137, #25417 ) ;
#19864 = CARTESIAN_POINT ( 'NONE',  ( 29.08426838874779108, -288.2148083501572273, -239.3479469218989664 ) ) ;
#19865 = CARTESIAN_POINT ( 'NONE',  ( 25.03291158125579585, -289.8944386141885161, -313.8494441673540791 ) ) ;
#19866 = CARTESIAN_POINT ( 'NONE',  ( -110.3469302561202454, -289.9618618412728779, -265.7208929794977053 ) ) ;
#19867 = CARTESIAN_POINT ( 'NONE',  ( -79.13156295577935850, -283.1074802814790701, -334.9609188179333614 ) ) ;
#19868 = CARTESIAN_POINT ( 'NONE',  ( 34.23643778570506413, -279.7168000767629792, -252.3372213726389077 ) ) ;
#19869 = CARTESIAN_POINT ( 'NONE',  ( 20.46231358632398312, -288.7647177333050763, -223.7624331235648754 ) ) ;
#19870 = CARTESIAN_POINT ( 'NONE',  ( 32.64108156036306241, -279.7265045949353066, -247.1108045521797578 ) ) ;
#19871 = CARTESIAN_POINT ( 'NONE',  ( -85.82196974150400592, -280.6790745625722252, -215.1261025035766465 ) ) ;
#19872 = CARTESIAN_POINT ( 'NONE',  ( -64.35006221551422811, -277.9065828417870421, -338.3010481819119946 ) ) ;
#19873 = CARTESIAN_POINT ( 'NONE',  ( -45.99623230670244567, -287.9543732541552572, -346.5264392340654354 ) ) ;
#19874 = CARTESIAN_POINT ( 'NONE',  ( -2.955911128589296499, -283.4122504978410575, -339.0909240032391949 ) ) ;
#19875 = CARTESIAN_POINT ( 'NONE',  ( -112.3011926466277828, -285.2615055784484639, -253.0232581102962968 ) ) ;
#19876 = CARTESIAN_POINT ( 'NONE',  ( -4.825256163146140587, -282.7781737388872330, -335.7192152346252669 ) ) ;
#19877 = ORIENTED_EDGE ( 'NONE', *, *, #47034, .T. ) ;
#19878 = CARTESIAN_POINT ( 'NONE',  ( 193.9646936176702070, 20.00000000000000000, -15.00000000000000000 ) ) ;
#19879 = CARTESIAN_POINT ( 'NONE',  ( -109.2659381197514961, -292.7191060495488273, -246.3806185591135431 ) ) ;
#19880 = CARTESIAN_POINT ( 'NONE',  ( -74.42510646798821483, -290.2543600667134456, -203.4423668922552793 ) ) ;
#19881 = CARTESIAN_POINT ( 'NONE',  ( 26.84851775130295692, -274.1296048084064978, -234.9988425568830905 ) ) ;
#19882 = CARTESIAN_POINT ( 'NONE',  ( -0.7619821634719919912, -293.9279871557318415, -338.0164812317882479 ) ) ;
#19883 = CARTESIAN_POINT ( 'NONE',  ( -99.43629866134806150, -288.4882768012640213, -310.0469918551870023 ) ) ;
#19884 = CARTESIAN_POINT ( 'NONE',  ( 30.40877048175368103, -292.1873985034024486, -300.1578920226834271 ) ) ;
#19885 = CARTESIAN_POINT ( 'NONE',  ( -108.1045342987575850, -291.4989204700930259, -290.0354864268057895 ) ) ;
#19886 = DIRECTION ( 'NONE',  ( 0.000000000000000000, 0.000000000000000000, -1.000000000000000000 ) ) ;
#19887 = CARTESIAN_POINT ( 'NONE',  ( -100.6003028256002665, -292.0089555232320322, -310.7474559801054284 ) ) ;
#19888 = CARTESIAN_POINT ( 'NONE',  ( -11.75283257161107109, -290.3842436657230337, -199.6294066718878639 ) ) ;
#19889 = CARTESIAN_POINT ( 'NONE',  ( -43.67058894805948199, -297.1322664049901050, -345.1064105123521131 ) ) ;
#19890 = CARTESIAN_POINT ( 'NONE',  ( -14.50397283338986121, -287.2967096829185039, -200.7245528512789292 ) ) ;
#19891 = CARTESIAN_POINT ( 'NONE',  ( 33.76072934726541064, -295.8689257727005497, -294.9025961025897118 ) ) ;
#19892 = CARTESIAN_POINT ( 'NONE',  ( 23.14423652758372540, -276.9213866659573569, -225.4182846009512957 ) ) ;
#19893 = CARTESIAN_POINT ( 'NONE',  ( -113.4421986318000535, -272.0436218923558158, -258.9516208099599908 ) ) ;
#19894 = CARTESIAN_POINT ( 'NONE',  ( 16.31731558162838169, -274.5168461903443244, -321.3384075001269480 ) ) ;
#19895 = CARTESIAN_POINT ( 'NONE',  ( -2.452958930701184315, -278.5972204303146782, -204.5888456860378426 ) ) ;
#19896 = CARTESIAN_POINT ( 'NONE',  ( -85.58263452931861082, -274.5725946120732033, -214.9766168087108156 ) ) ;
#19897 = CARTESIAN_POINT ( 'NONE',  ( 4.555368497081262014, -273.1799583960502673, -206.3980818031283775 ) ) ;
#19898 = CARTESIAN_POINT ( 'NONE',  ( -108.4093961080431683, -298.2282379495194959, -251.2138890455044020 ) ) ;
#19899 = CARTESIAN_POINT ( 'NONE',  ( 197.5277731217616122, 69.98851376390391010, 11.59179972292087513 ) ) ;
#19900 = CARTESIAN_POINT ( 'NONE',  ( -110.5360380290351685, -297.3763345195026773, -268.7394961063603773 ) ) ;
#19901 = CYLINDRICAL_SURFACE ( 'NONE', #3577, 7.500000000000013323 ) ;
#19903 = CARTESIAN_POINT ( 'NONE',  ( -36.48340605792428448, -298.0631913788034240, -197.3611179848009272 ) ) ;
#19902 = CARTESIAN_POINT ( 'NONE',  ( 36.67934959249920723, -285.3918560906939206, -256.2440714191681082 ) ) ;
#19904 = CARTESIAN_POINT ( 'NONE',  ( -64.54719059175596385, -285.7066592465739063, -198.3131993125137740 ) ) ;
#19905 = CARTESIAN_POINT ( 'NONE',  ( -40.34218509302081657, -288.7555934237355473, -347.2945534490193609 ) ) ;
#19906 = CARTESIAN_POINT ( 'NONE',  ( -112.4828589344016621, -298.6129001573509640, -264.0342027524442869 ) ) ;
#19907 = CARTESIAN_POINT ( 'NONE',  ( 11.46853091089890953, -292.3731666252827495, -327.0849204777914565 ) ) ;
#19908 = EDGE_CURVE ( 'NONE', #6488, #5433, #49573, .T. ) ;
#19909 = CARTESIAN_POINT ( 'NONE',  ( 20.95029152622550939, -280.0720102686328232, -220.2791208003248471 ) ) ;
#19910 = EDGE_CURVE ( 'NONE', #610, #39726, #77526, .T. ) ;
#19911 = CARTESIAN_POINT ( 'NONE',  ( -4.829096099716524648, -286.1237833571632905, -337.9475929042657754 ) ) ;
#19912 = CARTESIAN_POINT ( 'NONE',  ( -56.64738604829841506, -277.8032505011321405, -197.8352665249953759 ) ) ;
#19913 = CARTESIAN_POINT ( 'NONE',  ( 1.508823052283176480, -287.3150962168544993, -332.6328399207702660 ) ) ;
#19914 = LINE ( 'NONE', #63510, #41124 ) ;
#19915 = CARTESIAN_POINT ( 'NONE',  ( -7.444013132586889014, -286.6601309731845504, -339.1998302859839214 ) ) ;
#19916 = CARTESIAN_POINT ( 'NONE',  ( -103.8389552304829806, -274.4977754644102674, -238.5991467853361314 ) ) ;
#19918 = CARTESIAN_POINT ( 'NONE',  ( 34.23067989249568654, -281.7424991422525977, -284.7904588454235864 ) ) ;
#19917 = CARTESIAN_POINT ( 'NONE',  ( -111.0333716389159520, -270.8448262217655724, -253.6622631491634081 ) ) ;
#19919 = CARTESIAN_POINT ( 'NONE',  ( -98.23527737376741698, -297.3482087257295348, -223.2126454528674060 ) ) ;
#19920 = CARTESIAN_POINT ( 'NONE',  ( 21.13882259146600973, -276.3539895397269675, -225.6704442333011116 ) ) ;
#19921 = CARTESIAN_POINT ( 'NONE',  ( 37.55129286434630842, -285.5043265248769444, -260.3434436863306587 ) ) ;
#19922 = CARTESIAN_POINT ( 'NONE',  ( 0.3463326565518302647, -282.5539307346783175, -205.4590133269092007 ) ) ;
#19923 = CARTESIAN_POINT ( 'NONE',  ( -34.45629250580390135, -297.1478904710399433, -197.1262973527614122 ) ) ;
#19924 = VECTOR ( 'NONE', #78469, 1000.000000000000000 ) ;
#19925 = EDGE_LOOP ( 'NONE', ( #47310, #79631, #38502, #77134 ) ) ;
#19926 = CARTESIAN_POINT ( 'NONE',  ( 60.83509176750334291, -250.0104861964972258, 22.50000000000000000 ) ) ;
#19928 = CARTESIAN_POINT ( 'NONE',  ( -111.9541447851175917, -286.5604026035442757, -268.1634141801937403 ) ) ;
#19927 = AXIS2_PLACEMENT_3D ( 'NONE', #3842, #32724, #45979 ) ;
#19929 = CARTESIAN_POINT ( 'NONE',  ( 61.37083282337847123, -250.8548725835408391, 21.50000000000000000 ) ) ;
#19930 = CARTESIAN_POINT ( 'NONE',  ( -72.02372285203398405, -277.1237833571632905, -198.2697987213421698 ) ) ;
#19931 = CARTESIAN_POINT ( 'NONE',  ( 36.72722915942244981, -275.0065250947175741, -290.8540413367579163 ) ) ;
#19932 = VECTOR ( 'NONE', #4534, 999.9999999999998863 ) ;
#19933 = CARTESIAN_POINT ( 'NONE',  ( -95.65329390752376071, -285.4435574264955449, -315.4424003221237740 ) ) ;
#19934 = CARTESIAN_POINT ( 'NONE',  ( 12.30073783424776401, -277.9478274967066795, -325.0388014569549000 ) ) ;
#19935 = CARTESIAN_POINT ( 'NONE',  ( -97.56870268527291046, -285.3442247216904093, -317.3857334328633328 ) ) ;
#19936 = CARTESIAN_POINT ( 'NONE',  ( -93.73696302578666462, -282.6841478574131656, -317.3366949206035770 ) ) ;
#19937 = CARTESIAN_POINT ( 'NONE',  ( -5.955068411925046767, -282.4648207036316876, -202.2304355248318188 ) ) ;
#19938 = CARTESIAN_POINT ( 'NONE',  ( -67.53759791116084443, -273.8334939040555014, -199.5288671246859735 ) ) ;
#19939 = CARTESIAN_POINT ( 'NONE',  ( 23.63414251517103537, -274.7577112414791145, -223.3189515870644186 ) ) ;
#19940 = CARTESIAN_POINT ( 'NONE',  ( -107.3329321399949379, -298.1393858440949316, -295.8609516453394690 ) ) ;
#19941 = DIRECTION ( 'NONE',  ( -0.000000000000000000, -1.000000000000000000, -0.000000000000000000 ) ) ;
#19942 = CARTESIAN_POINT ( 'NONE',  ( 140.6539576904058606, 132.0000000000000568, 12.50000000000000000 ) ) ;
#19943 = CARTESIAN_POINT ( 'NONE',  ( -112.4317632126142428, -294.5586089432812855, -280.8352438237027400 ) ) ;
#19944 = EDGE_CURVE ( 'NONE', #37793, #58642, #24591, .T. ) ;
#19945 = CARTESIAN_POINT ( 'NONE',  ( 11.78444874418207355, -275.8556887629201810, -324.5094260177707497 ) ) ;
#19946 = CARTESIAN_POINT ( 'NONE',  ( -65.49921320297718808, -287.4391688771809754, -201.8585564823362972 ) ) ;
#19947 = CARTESIAN_POINT ( 'NONE',  ( 21.76201296504892468, -295.7261785416021098, -318.6461051238221671 ) ) ;
#19948 = CARTESIAN_POINT ( 'NONE',  ( 37.68481274290093097, -294.9515811969549759, -285.8217481897000880 ) ) ;
#19949 = CARTESIAN_POINT ( 'NONE',  ( -108.7586984996972888, -292.8417942537846557, -247.9652572111156985 ) ) ;
#19950 = CARTESIAN_POINT ( 'NONE',  ( -105.9624606558039943, -276.1589251778424341, -300.3443685384220316 ) ) ;
#19951 = CARTESIAN_POINT ( 'NONE',  ( -70.40140500038901905, -281.5330995528415770, -203.6508939139774270 ) ) ;
#19952 = CARTESIAN_POINT ( 'NONE',  ( -35.64177008129143331, -293.1105389541633599, -344.7944523728916124 ) ) ;
#19953 = CARTESIAN_POINT ( 'NONE',  ( -101.8537276316863540, -285.8847908249632610, -310.0915066855704936 ) ) ;
#19954 = CARTESIAN_POINT ( 'NONE',  ( -104.8769846099606582, -283.8551728052002545, -241.7138367005689190 ) ) ;
#19955 = CARTESIAN_POINT ( 'NONE',  ( 191.3713445966495499, 269.3054100996118336, -138.9528838864912075 ) ) ;
#19956 = ORIENTED_EDGE ( 'NONE', *, *, #18018, .F. ) ;
#19957 = CARTESIAN_POINT ( 'NONE',  ( -107.0073016536492503, -283.9289337795021311, -292.2424216654995348 ) ) ;
#19958 = ORIENTED_EDGE ( 'NONE', *, *, #81715, .T. ) ;
#19959 = CARTESIAN_POINT ( 'NONE',  ( 25.68417001321747506, -283.2116068919356735, -314.0789815084744987 ) ) ;
#19960 = CARTESIAN_POINT ( 'NONE',  ( -100.6595828943831492, -283.9196741993933983, -227.1530082133320434 ) ) ;
#19961 = CARTESIAN_POINT ( 'NONE',  ( -61.98348121027238022, -280.6808443343365980, -197.6029025719920753 ) ) ;
#19962 = CARTESIAN_POINT ( 'NONE',  ( -106.9357426684950241, -279.6674795972777474, -301.7846174024846277 ) ) ;
#19963 = CARTESIAN_POINT ( 'NONE',  ( -73.72474628654926221, -280.2335615410636365, -202.5996975595941478 ) ) ;
#19964 = CARTESIAN_POINT ( 'NONE',  ( -53.28691492658257545, -271.3380690714491266, -200.3538533559491555 ) ) ;
#19965 = CARTESIAN_POINT ( 'NONE',  ( 198.6655289599987384, 284.5870187839926757, -111.8036103090564382 ) ) ;
#19966 = CARTESIAN_POINT ( 'NONE',  ( -40.88665857834944717, -276.0077436703259082, -195.5608444318603745 ) ) ;
#19967 = CARTESIAN_POINT ( 'NONE',  ( 160.4760655529063911, 220.5667256801315261, -205.0173812340459563 ) ) ;
#19968 = CARTESIAN_POINT ( 'NONE',  ( -97.72166288328035932, -277.1729728092930714, -226.4736835347069643 ) ) ;
#19969 = CARTESIAN_POINT ( 'NONE',  ( -5.055330749482738639, -294.2315037087241762, -201.5747503673869119 ) ) ;
#19970 = CARTESIAN_POINT ( 'NONE',  ( -9.199295319417219119, -294.0228281539394857, -337.8424952510208641 ) ) ;
#19971 = CARTESIAN_POINT ( 'NONE',  ( -111.4843484015535324, -289.8021139158824440, -290.9133589880916588 ) ) ;
#19972 = DIRECTION ( 'NONE',  ( 0.5068419345592570791, -2.990798612913347986E-15, 0.8620390091940327570 ) ) ;
#19974 = CARTESIAN_POINT ( 'NONE',  ( -27.71220996078968568, -284.5763507776962911, -197.1920443709530275 ) ) ;
#19973 = CARTESIAN_POINT ( 'NONE',  ( -88.22667549685542099, -294.3226516898990326, -327.4349416818520808 ) ) ;
#19975 = CARTESIAN_POINT ( 'NONE',  ( -0.6667090460061715351, -294.4052438684481103, -205.8033098007449269 ) ) ;
#19976 = CARTESIAN_POINT ( 'NONE',  ( -14.33130992332623421, -284.8357321918245475, -200.2988074116600501 ) ) ;
#19977 = CARTESIAN_POINT ( 'NONE',  ( -110.8027547118739449, -285.8957914225510990, -268.1892671417301699 ) ) ;
#19978 = ORIENTED_EDGE ( 'NONE', *, *, #133, .T. ) ;
#19979 = CARTESIAN_POINT ( 'NONE',  ( -88.50161931618738720, -292.2964152334592427, -213.1292834756512775 ) ) ;
#19980 = CARTESIAN_POINT ( 'NONE',  ( -61.54920342400573219, -283.8675183020607165, -339.3490416550471878 ) ) ;
#19981 = CARTESIAN_POINT ( 'NONE',  ( -53.22199430612302251, -294.0462103635840094, -345.3541904683731332 ) ) ;
#19982 = CARTESIAN_POINT ( 'NONE',  ( -107.1180926905573756, -291.7688997321332636, -238.0564648206466245 ) ) ;
#19983 = CARTESIAN_POINT ( 'NONE',  ( -103.7421441121441603, -290.5370580429944880, -309.3317350788577187 ) ) ;
#19984 = CARTESIAN_POINT ( 'NONE',  ( 34.52206291861869403, -287.8880770959629558, -283.1907541928001137 ) ) ;
#19985 = EDGE_LOOP ( 'NONE', ( #73401, #27034, #84613, #64021, #93116, #2375 ) ) ;
#19986 = CYLINDRICAL_SURFACE ( 'NONE', #4993, 0.5000000000000004441 ) ;
#19987 = CARTESIAN_POINT ( 'NONE',  ( -111.9827764451988799, -298.2435621634423342, -283.6576445192034726 ) ) ;
#19988 = CARTESIAN_POINT ( 'NONE',  ( -98.68692294464464965, -295.8492338798204173, -224.6220641093916868 ) ) ;
#19989 = CARTESIAN_POINT ( 'NONE',  ( 22.31209271670305938, -280.0193616749232888, -227.8777865722506135 ) ) ;
#19990 = CARTESIAN_POINT ( 'NONE',  ( 37.84419997751617615, -275.2649468118802361, -286.7507640890440257 ) ) ;
#19991 = CARTESIAN_POINT ( 'NONE',  ( -103.1427785231897616, -295.4794976754084814, -237.0673529196825484 ) ) ;
#19992 = CARTESIAN_POINT ( 'NONE',  ( -97.87948571183410706, -279.8223121641687499, -313.3487764013228798 ) ) ;
#19993 = CARTESIAN_POINT ( 'NONE',  ( -4.744646648621247742, -272.6257127552618158, -203.6514982731144698 ) ) ;
#19994 = AXIS2_PLACEMENT_3D ( 'NONE', #58455, #65112, #57988 ) ;
#19995 = CARTESIAN_POINT ( 'NONE',  ( -31.55582687073997405, -296.1827040247025593, -343.5801729685740042 ) ) ;
#19996 = CARTESIAN_POINT ( 'NONE',  ( -108.8905680528670246, -297.4220659071904151, -286.3293856841414708 ) ) ;
#19997 = CARTESIAN_POINT ( 'NONE',  ( 200.4644824113734387, 215.0000000000000568, -2.942835885954282471 ) ) ;
#19998 = CARTESIAN_POINT ( 'NONE',  ( -32.04753574849496545, -296.5865674671629222, -346.3901031670015414 ) ) ;
#19999 = AXIS2_PLACEMENT_3D ( 'NONE', #20747, #57216, #49618 ) ;
#20000 = CARTESIAN_POINT ( 'NONE',  ( -72.40225788177887978, -295.5895106912616939, -203.8146963531014251 ) ) ;
#20001 = CARTESIAN_POINT ( 'NONE',  ( -6.005447940128382456, -293.1266639701533450, -204.3023939260049247 ) ) ;
#20002 = CARTESIAN_POINT ( 'NONE',  ( -55.30580511946723021, -274.6295514870644183, -195.6520171189104360 ) ) ;
#20003 = CARTESIAN_POINT ( 'NONE',  ( -106.5931539357383855, -288.7980200035270286, -295.2531058900292464 ) ) ;
#20004 = CARTESIAN_POINT ( 'NONE',  ( 215.9306832106271088, -142.7221692137691775, 9.184850993605173582E-16 ) ) ;
#20005 = CARTESIAN_POINT ( 'NONE',  ( -104.1791820075805504, -273.5410518952702432, -232.1454206897277288 ) ) ;
#20007 = CARTESIAN_POINT ( 'NONE',  ( -75.22524286702045515, -297.8657468433290205, -207.8771396955177693 ) ) ;
#20006 = AXIS2_PLACEMENT_3D ( 'NONE', #87884, #37701, #16408 ) ;
#20008 = AXIS2_PLACEMENT_3D ( 'NONE', #59763, #68243, #10459 ) ;
#20009 = CARTESIAN_POINT ( 'NONE',  ( -14.74552191971798010, -282.3232764346112162, -198.4188702412958776 ) ) ;
#20010 = CARTESIAN_POINT ( 'NONE',  ( 37.65877536361002598, -280.4271376863619594, -285.4683000579449867 ) ) ;
#20011 = CARTESIAN_POINT ( 'NONE',  ( -31.46634335474100652, -276.3285291766658247, -347.0869588441506721 ) ) ;
#20012 = CARTESIAN_POINT ( 'NONE',  ( 19.54517269016981729, -279.2573273944075822, -219.6431280061817972 ) ) ;
#20013 = CARTESIAN_POINT ( 'NONE',  ( 29.11317099448432444, -279.0860963724547901, -235.1248985799621778 ) ) ;
#20014 = CARTESIAN_POINT ( 'NONE',  ( -57.00171108673121267, -272.3684171248539201, -199.3935320658721650 ) ) ;
#20015 = CARTESIAN_POINT ( 'NONE',  ( -97.20430083200136551, -281.1703169608771304, -225.1575159393051138 ) ) ;
#20016 = DIRECTION ( 'NONE',  ( 0.000000000000000000, 0.000000000000000000, 1.000000000000000000 ) ) ;
#20017 = DIRECTION ( 'NONE',  ( 0.000000000000000000, -1.000000000000000000, 0.000000000000000000 ) ) ;
#20018 = CARTESIAN_POINT ( 'NONE',  ( -92.90624787607011115, -295.5087688527922865, -218.4524048373820335 ) ) ;
#20019 = CARTESIAN_POINT ( 'NONE',  ( -4.604144321097812131, -292.4716473784062032, -200.6671265644712037 ) ) ;
#20020 = CARTESIAN_POINT ( 'NONE',  ( 35.12510414080808374, -277.8090652632523074, -290.3739080526739826 ) ) ;
#20021 = CARTESIAN_POINT ( 'NONE',  ( -33.92475487546162327, -272.0949882399519879, -195.4389908371266245 ) ) ;
#20022 = ADVANCED_FACE ( 'NONE', ( #85085 ), #36662, .T. ) ;
#20023 = DIRECTION ( 'NONE',  ( -0.8457827187922972723, -0.5335274993777825436, -0.000000000000000000 ) ) ;
#20024 = CARTESIAN_POINT ( 'NONE',  ( 22.28199568906610395, -284.1043718082944451, -316.7967854410098312 ) ) ;
#20025 = DIRECTION ( 'NONE',  ( -1.000000000000000000, 0.000000000000000000, 0.000000000000000000 ) ) ;
#20026 = CARTESIAN_POINT ( 'NONE',  ( 0.8551782934694188709, -284.5611025376319958, -205.7571982348605673 ) ) ;
#20027 = FACE_OUTER_BOUND ( 'NONE', #63093, .T. ) ;
#20028 = CARTESIAN_POINT ( 'NONE',  ( 20.82856513173618040, -292.9738363566014527, -315.1404969690702274 ) ) ;
#20029 = CARTESIAN_POINT ( 'NONE',  ( 35.21295173079262497, -285.8962048697335376, -286.1269500914702348 ) ) ;
#20030 = CARTESIAN_POINT ( 'NONE',  ( 159.3464669004307268, 16.14910309755065398, -9.103988188768896705 ) ) ;
#20031 = CARTESIAN_POINT ( 'NONE',  ( 17.60757943251340762, -292.2661600556220378, -321.4059739920773495 ) ) ;
#20032 = CARTESIAN_POINT ( 'NONE',  ( -68.20244818725494440, -284.1340704704256268, -200.5591808367052806 ) ) ;
#20033 = CARTESIAN_POINT ( 'NONE',  ( -111.0786297607549642, -280.1124829652855510, -273.4116296694433004 ) ) ;
#20034 = CARTESIAN_POINT ( 'NONE',  ( 38.28548676386245830, -288.9144956966022733, -282.8715916027106232 ) ) ;
#20035 = CARTESIAN_POINT ( 'NONE',  ( 36.99803877511962469, -279.5918201155166116, -254.5641974274557811 ) ) ;
#20036 = CARTESIAN_POINT ( 'NONE',  ( 34.01067763643982289, -287.7563193171338298, -285.8417480492505547 ) ) ;
#20037 = CARTESIAN_POINT ( 'NONE',  ( -54.64883464035107608, -281.2507713869273971, -198.7834094798326134 ) ) ;
#20038 = CARTESIAN_POINT ( 'NONE',  ( -64.88637029251910349, -280.4857530425537107, -202.5828554443387759 ) ) ;
#20039 = CARTESIAN_POINT ( 'NONE',  ( -62.67277580053323760, -287.7039761364958395, -199.3911003191245186 ) ) ;
#20040 = ORIENTED_EDGE ( 'NONE', *, *, #79416, .T. ) ;
#20041 = CARTESIAN_POINT ( 'NONE',  ( -93.66130201641277608, -297.1019729443513029, -217.7752289675644874 ) ) ;
#20042 = CARTESIAN_POINT ( 'NONE',  ( -75.53633936148847283, -291.5441692366258053, -334.5089353002856569 ) ) ;
#20043 = CARTESIAN_POINT ( 'NONE',  ( 207.2445280759194475, 36.58490166922437226, 13.79342392267524708 ) ) ;
#20044 = CARTESIAN_POINT ( 'NONE',  ( -19.11405058567862625, -294.7662352645559736, -190.3538533559490702 ) ) ;
#20045 = ORIENTED_EDGE ( 'NONE', *, *, #16723, .T. ) ;
#20046 = CARTESIAN_POINT ( 'NONE',  ( -32.76808252924960385, -272.1094782166812251, -195.3208826116317880 ) ) ;
#20047 = DIRECTION ( 'NONE',  ( -0.5877852522924802425, 0.000000000000000000, -0.8090169943749422332 ) ) ;
#20048 = CARTESIAN_POINT ( 'NONE',  ( -92.13604411657455273, -294.2190398984069475, -323.3141186699876357 ) ) ;
#20049 = CARTESIAN_POINT ( 'NONE',  ( -47.27491394963309546, -297.4303200076844291, -197.9267195464555016 ) ) ;
#20050 = CARTESIAN_POINT ( 'NONE',  ( 1.695109183097748051, -290.0398546098388692, -332.8657999730142478 ) ) ;
#20051 = CARTESIAN_POINT ( 'NONE',  ( 25.99195518158492035, -282.7911378813158763, -231.9627339860960547 ) ) ;
#20052 = CARTESIAN_POINT ( 'NONE',  ( -37.48375456549062079, -290.3690268334146936, -346.8808256503987195 ) ) ;
#20053 = CARTESIAN_POINT ( 'NONE',  ( -73.35618142252829443, -287.5746980787349685, -204.5592937361379597 ) ) ;
#20054 = CARTESIAN_POINT ( 'NONE',  ( -94.96319964996769158, -279.4108287468890239, -219.2850688267585895 ) ) ;
#20055 = CARTESIAN_POINT ( 'NONE',  ( -32.13658348927195618, -293.0668532447227790, -345.7546324691795121 ) ) ;
#20056 = CARTESIAN_POINT ( 'NONE',  ( 27.85248385341587252, -280.8478708096207583, -229.2890245579890802 ) ) ;
#20057 = CARTESIAN_POINT ( 'NONE',  ( 34.04130678602621174, -277.1454403860069533, -249.7979589964799061 ) ) ;
#20058 = CARTESIAN_POINT ( 'NONE',  ( 27.33386217378599881, -277.6233781216988064, -239.1787733560258573 ) ) ;
#20059 = CARTESIAN_POINT ( 'NONE',  ( 38.12837484848169822, -273.9096893195509779, -279.6466119788075275 ) ) ;
#20061 = AXIS2_PLACEMENT_3D ( 'NONE', #49937, #79764, #93493 ) ;
#20060 = DIRECTION ( 'NONE',  ( -0.6056179655966478226, 0.7957555401921982963, 0.000000000000000000 ) ) ;
#20062 = CARTESIAN_POINT ( 'NONE',  ( 32.79542189131238672, -280.7893188386312886, -249.8971849152191851 ) ) ;
#20063 = AXIS2_PLACEMENT_3D ( 'NONE', #71362, #56703, #5566 ) ;
#20064 = CARTESIAN_POINT ( 'NONE',  ( -68.83801591382037088, -278.6621530774514213, -340.2037419698561393 ) ) ;
#20065 = CARTESIAN_POINT ( 'NONE',  ( -64.76827231773779658, -275.0015256347070931, -202.1637746357501726 ) ) ;
#20066 = CARTESIAN_POINT ( 'NONE',  ( -113.5845479338653519, -283.7229996255427409, -261.4253264038227940 ) ) ;
#20067 = CARTESIAN_POINT ( 'NONE',  ( -95.09552022463829246, -292.9576642491689427, -224.0541454722773267 ) ) ;
#20068 = CARTESIAN_POINT ( 'NONE',  ( -93.56886751066616625, -274.8592502623891392, -218.9128074112863658 ) ) ;
#20069 = VECTOR ( 'NONE', #53406, 1000.000000000000000 ) ;
#20070 = CARTESIAN_POINT ( 'NONE',  ( -36.95912481475801314, -275.3720476784394009, -193.8422551742366693 ) ) ;
#20071 = CARTESIAN_POINT ( 'NONE',  ( 152.4536156746142410, 275.5000000000000568, -11.99999999999999289 ) ) ;
#20072 = CARTESIAN_POINT ( 'NONE',  ( -21.65509044688186435, -276.6788735553477636, -341.7077821993584053 ) ) ;
#20073 = CARTESIAN_POINT ( 'NONE',  ( -91.72241644707095531, -297.8292329130355256, -321.8435559369090129 ) ) ;
#20074 = CARTESIAN_POINT ( 'NONE',  ( -82.56679668817990603, -283.4324854685679611, -210.7396531851886152 ) ) ;
#20075 = TOROIDAL_SURFACE ( 'NONE', #88109, 203.9779373800640485, 1.000000000000000000 ) ;
#20076 = CARTESIAN_POINT ( 'NONE',  ( -36.37436963039452564, -291.7306902225533918, -193.3753110228519461 ) ) ;
#20077 = CARTESIAN_POINT ( 'NONE',  ( 29.49220761520184553, -274.0144666445947905, -303.7202385540210798 ) ) ;
#20078 = CARTESIAN_POINT ( 'NONE',  ( -5.937388334416650260, -290.2463030297726050, -339.7888474456598260 ) ) ;
#20079 = CARTESIAN_POINT ( 'NONE',  ( -110.6462937780810307, -289.4617814156164286, -271.1751342254810879 ) ) ;
#20080 = ORIENTED_EDGE ( 'NONE', *, *, #8048, .T. ) ;
#20081 = CARTESIAN_POINT ( 'NONE',  ( -33.55030903467089587, -290.6737327303923166, -194.0444641822093388 ) ) ;
#20082 = CARTESIAN_POINT ( 'NONE',  ( -86.74680755776698504, -289.4284379574972945, -324.1998089338482032 ) ) ;
#20083 = VERTEX_POINT ( 'NONE', #50967 ) ;
#20084 = CARTESIAN_POINT ( 'NONE',  ( 20.04626073632925198, -287.9391673013628861, -219.4092285710269152 ) ) ;
#20085 = CARTESIAN_POINT ( 'NONE',  ( -108.9088177157139796, -279.0774796836156497, -255.7988221804640148 ) ) ;
#20086 = CARTESIAN_POINT ( 'NONE',  ( -98.03827912585100535, -294.8442727680667304, -317.2377412505912275 ) ) ;
#20087 = CARTESIAN_POINT ( 'NONE',  ( -97.50584265687383834, -285.8455798200195090, -222.4696913907785074 ) ) ;
#20088 = CARTESIAN_POINT ( 'NONE',  ( -100.9814059380279474, -285.4577828819154206, -226.9572253947787033 ) ) ;
#20089 = CARTESIAN_POINT ( 'NONE',  ( 33.34504874474222902, -282.1277551011364153, -288.7268030233975082 ) ) ;
#20090 = CARTESIAN_POINT ( 'NONE',  ( 185.2826429462496947, 263.6716433825772583, -153.3442153897663616 ) ) ;
#20091 = CARTESIAN_POINT ( 'NONE',  ( 159.7575371838252920, 220.4114972407526523, -204.4531022271711720 ) ) ;
#20092 = CARTESIAN_POINT ( 'NONE',  ( 152.4322389789791998, 205.2264399568286706, -214.4046794774016576 ) ) ;
#20093 = CARTESIAN_POINT ( 'NONE',  ( 9.596493148575063969, -273.9141057013902127, -214.1751838174417628 ) ) ;
#20094 = CARTESIAN_POINT ( 'NONE',  ( -21.85538011468237229, -273.1756386990497276, -198.7063905385278133 ) ) ;
#20095 = CARTESIAN_POINT ( 'NONE',  ( -110.2893569753809402, -295.7515852926684374, -294.8185557810772934 ) ) ;
#20096 = CARTESIAN_POINT ( 'NONE',  ( 139.6181910892751716, 178.0063059127244856, -238.5957382375125064 ) ) ;
#20097 = CARTESIAN_POINT ( 'NONE',  ( 37.15855946076516148, -274.0172280141567853, -252.8969037922039149 ) ) ;
#20098 = CARTESIAN_POINT ( 'NONE',  ( -63.53714435172094710, -299.5676532963165073, -200.8469228458471605 ) ) ;
#20099 = CARTESIAN_POINT ( 'NONE',  ( -17.36149982982482953, -293.3956680683000400, -199.7745010282513647 ) ) ;
#20100 = ORIENTED_EDGE ( 'NONE', *, *, #27543, .T. ) ;
#20101 = CARTESIAN_POINT ( 'NONE',  ( -110.5922287740041554, -297.7847741135059323, -247.2244140488346602 ) ) ;
#20102 = CARTESIAN_POINT ( 'NONE',  ( -8.188177821665913569, -289.1522358358262750, -337.4081945741010600 ) ) ;
#20103 = AXIS2_PLACEMENT_3D ( 'NONE', #3381, #32269, #61175 ) ;
#20104 = CARTESIAN_POINT ( 'NONE',  ( -113.2316824492032765, -297.5068725265143144, -258.2415258761737391 ) ) ;
#20105 = CARTESIAN_POINT ( 'NONE',  ( -56.04924808363270472, -295.7792095461983308, -344.9905662757627169 ) ) ;
#20106 = CARTESIAN_POINT ( 'NONE',  ( -22.74270262261855180, -292.4109186769933331, -198.8358128359274133 ) ) ;
#20107 = ORIENTED_EDGE ( 'NONE', *, *, #20400, .T. ) ;
#20108 = EDGE_CURVE ( 'NONE', #3537, #46977, #43397, .T. ) ;
#20109 = CARTESIAN_POINT ( 'NONE',  ( 36.77474715412966333, -277.6596393236907829, -285.0603167087974725 ) ) ;
#20110 = VERTEX_POINT ( 'NONE', #35838 ) ;
#20111 = CARTESIAN_POINT ( 'NONE',  ( 10.78940024551518562, -280.2047063490701362, -210.2684645879271841 ) ) ;
#20112 = CARTESIAN_POINT ( 'NONE',  ( 15.77676739851996501, -277.2178036085222743, -320.7777507121354006 ) ) ;
#20113 = CARTESIAN_POINT ( 'NONE',  ( 33.76550065166610892, -276.9688174047132634, -243.5704477892614648 ) ) ;
#20114 = CARTESIAN_POINT ( 'NONE',  ( -37.15686973064618570, -275.0699269267319664, -345.7288748229163957 ) ) ;
#20115 = CARTESIAN_POINT ( 'NONE',  ( -37.83151420578207791, -298.6972715054471337, -197.2608255704180920 ) ) ;
#20116 = CARTESIAN_POINT ( 'NONE',  ( -109.3519788511818263, -295.3260676909511062, -255.1383242376388694 ) ) ;
#20117 = CARTESIAN_POINT ( 'NONE',  ( -100.4114633486748858, -278.4615197745321211, -314.4262047359401890 ) ) ;
#20118 = CARTESIAN_POINT ( 'NONE',  ( -29.71131375633569505, -277.1196749686742464, -343.0121425007147309 ) ) ;
#20119 = CARTESIAN_POINT ( 'NONE',  ( 1.287239695076142443, -285.2416008112440977, -204.3072262123218366 ) ) ;
#20120 = CARTESIAN_POINT ( 'NONE',  ( -112.3426463542470799, -274.5878523713495838, -267.5935413054058927 ) ) ;
#20121 = CARTESIAN_POINT ( 'NONE',  ( 82.61849213892784860, -301.9425569738761510, -196.1180017367229880 ) ) ;
#20122 = AXIS2_PLACEMENT_3D ( 'NONE', #33052, #11740, #12700 ) ;
#20123 = CARTESIAN_POINT ( 'NONE',  ( 25.83032970961048846, -287.2559421351874676, -307.3651295578798113 ) ) ;
#20124 = ADVANCED_FACE ( 'NONE', ( #50508 ), #58096, .F. ) ;
#20125 = CARTESIAN_POINT ( 'NONE',  ( -27.40037784261229703, -278.4198998218683982, -196.9665660256600006 ) ) ;
#20127 = CARTESIAN_POINT ( 'NONE',  ( -101.6573424560296957, -282.1275674972855541, -307.8419443853190955 ) ) ;
#20126 = CARTESIAN_POINT ( 'NONE',  ( -54.61361778231162845, -278.4006854406470666, -198.7749040549008441 ) ) ;
#20128 = CARTESIAN_POINT ( 'NONE',  ( -38.77567384759880298, -288.0343566558874500, -195.3621995646847154 ) ) ;
#20129 = CARTESIAN_POINT ( 'NONE',  ( 24.32629861042931552, -277.3063535309164536, -310.2567247996188939 ) ) ;
#20130 = DIRECTION ( 'NONE',  ( 0.000000000000000000, 0.000000000000000000, 1.000000000000000000 ) ) ;
#20131 = AXIS2_PLACEMENT_3D ( 'NONE', #56969, #79998, #20016 ) ;
#20132 = CARTESIAN_POINT ( 'NONE',  ( -93.23819352308036912, -293.2486548172820449, -220.3552915587440566 ) ) ;
#20133 = CARTESIAN_POINT ( 'NONE',  ( -28.73832709560946697, -275.1844852894727183, -345.9120399221340563 ) ) ;
#20134 = VECTOR ( 'NONE', #69604, 1000.000000000000000 ) ;
#20135 = CARTESIAN_POINT ( 'NONE',  ( 15.67751261981096000, -276.9280115873633576, -320.6886029962282123 ) ) ;
#20136 = CARTESIAN_POINT ( 'NONE',  ( 35.42360950894337179, -283.7939573953727859, -289.2088802653337325 ) ) ;
#20137 = AXIS2_PLACEMENT_3D ( 'NONE', #72293, #42937, #64756 ) ;
#20138 = DIRECTION ( 'NONE',  ( 0.000000000000000000, 0.000000000000000000, 1.000000000000000000 ) ) ;
#20139 = CARTESIAN_POINT ( 'NONE',  ( -20.78761857074142938, -290.7615670060641264, -344.1390953996880739 ) ) ;
#20140 = AXIS2_PLACEMENT_3D ( 'NONE', #65711, #24433, #67079 ) ;
#20141 = CARTESIAN_POINT ( 'NONE',  ( -17.69740863898349303, -292.7987519615044789, -342.7959879880374388 ) ) ;
#20142 = CARTESIAN_POINT ( 'NONE',  ( 209.6287663260175975, 29.00782453271232697, 15.00000000000000000 ) ) ;
#20143 = CARTESIAN_POINT ( 'NONE',  ( 25.70745865827042920, -273.7198733116884455, -232.4994721079409317 ) ) ;
#20144 = CARTESIAN_POINT ( 'NONE',  ( 17.66919031077154045, -290.9887443108297020, -220.4392572792103806 ) ) ;
#20145 = CARTESIAN_POINT ( 'NONE',  ( 196.1720347589760252, 41.44788071521509210, 14.04783121195910844 ) ) ;
#20146 = LINE ( 'NONE', #6889, #54936 ) ;
#20147 = CARTESIAN_POINT ( 'NONE',  ( -40.58341442781975417, -290.4919935937610376, -194.1102747254016094 ) ) ;
#20148 = CARTESIAN_POINT ( 'NONE',  ( 36.83084173599346656, -286.0019373028050040, -286.9252314698308055 ) ) ;
#20149 = CIRCLE ( 'NONE', #50573, 0.5000000000000004441 ) ;
#20150 = EDGE_CURVE ( 'NONE', #62642, #36954, #86465, .T. ) ;
#20151 = CARTESIAN_POINT ( 'NONE',  ( -104.6449366095063027, -285.5801239586100451, -300.1209781073677050 ) ) ;
#20152 = CARTESIAN_POINT ( 'NONE',  ( -85.84082221598471563, -286.1631219849281820, -215.5171537372244472 ) ) ;
#20153 = CARTESIAN_POINT ( 'NONE',  ( -47.54616045868586838, -293.9030850245948159, -195.6473976999308206 ) ) ;
#20154 = CARTESIAN_POINT ( 'NONE',  ( 33.83608930054545993, -273.9599221947258911, -295.8733605699800364 ) ) ;
#20155 = CARTESIAN_POINT ( 'NONE',  ( 31.22953744634706652, -275.4347737680809018, -235.3792702762425506 ) ) ;
#20156 = AXIS2_PLACEMENT_3D ( 'NONE', #72886, #24078, #45847 ) ;
#20157 = CARTESIAN_POINT ( 'NONE',  ( -111.2266390754934946, -288.8343882334787054, -254.4783484646853537 ) ) ;
#20158 = CARTESIAN_POINT ( 'NONE',  ( -7.884636678422499045, -276.6767267706535449, -341.5180861090478857 ) ) ;
#20159 = CARTESIAN_POINT ( 'NONE',  ( -105.4267562159298137, -298.1274605023674553, -301.0859327147970816 ) ) ;
#20160 = LINE ( 'NONE', #40960, #69616 ) ;
#20161 = CARTESIAN_POINT ( 'NONE',  ( 208.3427284608899868, 37.37804188714573428, 12.00000001296747598 ) ) ;
#20162 = CARTESIAN_POINT ( 'NONE',  ( -110.5886280708645160, -283.1582098256154154, -276.3720267395096357 ) ) ;
#20163 = CARTESIAN_POINT ( 'NONE',  ( -53.30917782360364043, -277.8473460191802360, -197.0274110760031760 ) ) ;
#20164 = CARTESIAN_POINT ( 'NONE',  ( -2.853431178006288871, -272.9794744330255867, -202.2784400007492422 ) ) ;
#20165 = CARTESIAN_POINT ( 'NONE',  ( -109.3879580793719413, -277.7366946234744205, -282.8137408938397357 ) ) ;
#20166 = CARTESIAN_POINT ( 'NONE',  ( -26.08256051640834983, -296.4263249035763579, -343.1892686268481043 ) ) ;
#20167 = VECTOR ( 'NONE', #30776, 1000.000000000000000 ) ;
#20168 = CARTESIAN_POINT ( 'NONE',  ( -40.97992034744468981, -278.9277414701869588, -193.7434333128720993 ) ) ;
#20169 = CARTESIAN_POINT ( 'NONE',  ( -55.85123976163615822, -296.2374980330741323, -341.2713093379865654 ) ) ;
#20170 = CARTESIAN_POINT ( 'NONE',  ( -0.9260546494287595909, -295.8942566626101325, -337.6603729592434888 ) ) ;
#20171 = CARTESIAN_POINT ( 'NONE',  ( -102.0472147585561515, -272.6806025721981541, -236.4095710574711404 ) ) ;
#20172 = CARTESIAN_POINT ( 'NONE',  ( -38.96574107484891414, -294.0319303747026538, -195.3786990875417189 ) ) ;
#20173 = CARTESIAN_POINT ( 'NONE',  ( -37.98457500666072661, -286.2109853173925558, -193.3638016889015887 ) ) ;
#20174 = CARTESIAN_POINT ( 'NONE',  ( 24.33538729457488614, -273.0991493527042167, -226.3361606592911812 ) ) ;
#20175 = CARTESIAN_POINT ( 'NONE',  ( -48.87109260429120638, -289.0283139329745268, -346.5470079670103019 ) ) ;
#20176 = CARTESIAN_POINT ( 'NONE',  ( -54.90369035024288991, -281.8053020300051230, -197.7582857938907352 ) ) ;
#20177 = CARTESIAN_POINT ( 'NONE',  ( 7.079127850946671963, -285.7325377364758197, -212.0716252673045119 ) ) ;
#20178 = CARTESIAN_POINT ( 'NONE',  ( -93.96551828184074395, -287.8695570610788081, -319.5418445805968872 ) ) ;
#20179 = CARTESIAN_POINT ( 'NONE',  ( 139.3989977797154154, 177.7276089766264704, -238.0725708408485843 ) ) ;
#20180 = CARTESIAN_POINT ( 'NONE',  ( 32.33416872850242640, -286.7681413187816020, -248.3360072627604325 ) ) ;
#20181 = CARTESIAN_POINT ( 'NONE',  ( 180.2288731078812702, 275.0000000000000568, -24.90909090909093848 ) ) ;
#20182 = CARTESIAN_POINT ( 'NONE',  ( 38.64008698756167348, -282.6305856204697875, -281.2967587790881794 ) ) ;
#20183 = CARTESIAN_POINT ( 'NONE',  ( -112.4073492084067851, -289.8131316561925246, -254.2377481203194520 ) ) ;
#20184 = CARTESIAN_POINT ( 'NONE',  ( -107.9078311530945058, -279.7832309258712371, -299.1163186579315720 ) ) ;
#20185 = CARTESIAN_POINT ( 'NONE',  ( -64.58250098870418299, -281.0191529625151361, -198.8123268789160534 ) ) ;
#20186 = CARTESIAN_POINT ( 'NONE',  ( 27.78235261977501835, -280.9363061009318017, -237.2663388890804015 ) ) ;
#20187 = CARTESIAN_POINT ( 'NONE',  ( 35.44414798062614835, -277.3199673566674619, -252.2718679261091665 ) ) ;
#20188 = CARTESIAN_POINT ( 'NONE',  ( -47.63157325885072879, -295.1795367299789632, -346.6704785548560608 ) ) ;
#20189 = CARTESIAN_POINT ( 'NONE',  ( -103.1038996189127346, -288.1000290318023076, -305.7862101314099732 ) ) ;
#20190 = CARTESIAN_POINT ( 'NONE',  ( -103.0513045628199649, -295.0323738833450307, -302.9793209375142169 ) ) ;
#20191 = VERTEX_POINT ( 'NONE', #22545 ) ;
#20192 = ORIENTED_EDGE ( 'NONE', *, *, #76386, .T. ) ;
#20193 = CARTESIAN_POINT ( 'NONE',  ( 25.35625050481410625, -284.0177780539782475, -310.5842330859917411 ) ) ;
#20194 = CARTESIAN_POINT ( 'NONE',  ( -97.20314257997455343, -295.6359571892910481, -312.1785209911674883 ) ) ;
#20195 = AXIS2_PLACEMENT_3D ( 'NONE', #84515, #77431, #69860 ) ;
#20196 = CARTESIAN_POINT ( 'NONE',  ( 23.72073476802203018, -294.0107570384902829, -223.9404656963076548 ) ) ;
#20197 = CARTESIAN_POINT ( 'NONE',  ( -53.70442692472617807, -283.9190000381987034, -341.6604057112347732 ) ) ;
#20198 = CARTESIAN_POINT ( 'NONE',  ( -41.16900876815732602, -273.0639740661492283, -193.6397803870029577 ) ) ;
#20199 = CARTESIAN_POINT ( 'NONE',  ( -66.98382599163394957, -292.3251023065710115, -199.4057999223121271 ) ) ;
#20200 = CARTESIAN_POINT ( 'NONE',  ( -30.96383551090100639, -284.2714936815391980, -194.8521535206214139 ) ) ;
#20201 = CARTESIAN_POINT ( 'NONE',  ( -82.83673185939223060, -289.9889221217006252, -332.4573850137394970 ) ) ;
#20203 = CARTESIAN_POINT ( 'NONE',  ( 3.629980534029428441, -288.8176293778209924, -330.8655263877317907 ) ) ;
#20202 = AXIS2_PLACEMENT_3D ( 'NONE', #23635, #2336, #17471 ) ;
#20204 = CARTESIAN_POINT ( 'NONE',  ( 208.4306832106270804, -198.2391364535880598, 0.000000000000000000 ) ) ;
#20205 = VECTOR ( 'NONE', #63356, 1000.000000000000000 ) ;
#20206 = DIRECTION ( 'NONE',  ( -0.000000000000000000, 1.000000000000000000, -0.000000000000000000 ) ) ;
#20207 = CARTESIAN_POINT ( 'NONE',  ( -55.21708144420773579, -169.6647128743276198, -360.6205609466671262 ) ) ;
#20208 = CARTESIAN_POINT ( 'NONE',  ( -41.51171161027219370, -284.6237506083643893, -346.6056163753486885 ) ) ;
#20209 = CARTESIAN_POINT ( 'NONE',  ( 39.58706461736021254, -291.0523547857346784, -270.3937649182068981 ) ) ;
#20210 = EDGE_LOOP ( 'NONE', ( #40575, #9184, #70666, #77033, #40304, #39033 ) ) ;
#20211 = CARTESIAN_POINT ( 'NONE',  ( 33.41553229368502542, -280.2196921497937296, -251.1391125658965962 ) ) ;
#20212 = CARTESIAN_POINT ( 'NONE',  ( 21.71167546289456141, -275.8835959873263732, -319.7417125813740881 ) ) ;
#20213 = CARTESIAN_POINT ( 'NONE',  ( -73.71128243261479440, -279.5362303201901568, -335.7767905355797780 ) ) ;
#20214 = CARTESIAN_POINT ( 'NONE',  ( -20.14603930832873502, -109.6676116220293835, -360.2926962469870773 ) ) ;
#20215 = CARTESIAN_POINT ( 'NONE',  ( 39.12091579616689074, -280.1217208419323583, -269.9516809897648955 ) ) ;
#20217 = CIRCLE ( 'NONE', #12655, 7.500000000000012434 ) ;
#20216 = CARTESIAN_POINT ( 'NONE',  ( -55.12427778965803782, -283.8425770811846292, -197.8119445251706168 ) ) ;
#20218 = CARTESIAN_POINT ( 'NONE',  ( -101.4733360123586294, -298.8535885687790028, -229.6044339707148652 ) ) ;
#20219 = CARTESIAN_POINT ( 'NONE',  ( 35.48627625942331321, -294.1214413835087953, -276.1984373020115413 ) ) ;
#20220 = ORIENTED_EDGE ( 'NONE', *, *, #32641, .T. ) ;
#20221 = CARTESIAN_POINT ( 'NONE',  ( -95.49440411143764607, -289.8654624382443785, -225.4221983369952511 ) ) ;
#20222 = CARTESIAN_POINT ( 'NONE',  ( 38.11712176391364437, -276.0181213643333535, -255.5530463461401780 ) ) ;
#20223 = CARTESIAN_POINT ( 'NONE',  ( -67.05750530498295348, -273.6514624167348870, -203.6693107640952860 ) ) ;
#20224 = ORIENTED_EDGE ( 'NONE', *, *, #62141, .F. ) ;
#20225 = LINE ( 'NONE', #78001, #61348 ) ;
#20226 = CARTESIAN_POINT ( 'NONE',  ( 180.6209651459523968, 249.5000000000000568, -24.41176470588237635 ) ) ;
#20227 = AXIS2_PLACEMENT_3D ( 'NONE', #53558, #45971, #74877 ) ;
#20228 = CYLINDRICAL_SURFACE ( 'NONE', #63967, 9.103929867429224387 ) ;
#20229 = AXIS2_PLACEMENT_3D ( 'NONE', #63371, #71865, #28759 ) ;
#20230 = CARTESIAN_POINT ( 'NONE',  ( -21.30727050855444915, -283.9214463001050603, -341.9474228160043481 ) ) ;
#20231 = CARTESIAN_POINT ( 'NONE',  ( -96.04903109183956644, -280.9691240146350424, -222.0975020886282891 ) ) ;
#20232 = CARTESIAN_POINT ( 'NONE',  ( -110.1079542799334661, -283.4963208918729833, -279.0744888805806454 ) ) ;
#20233 = CARTESIAN_POINT ( 'NONE',  ( -39.76489218590018027, -281.8818463398827134, -196.1527423568188340 ) ) ;
#20234 = CARTESIAN_POINT ( 'NONE',  ( 22.85829715218401503, -273.4440892567648689, -227.8343478696969555 ) ) ;
#20235 = DIRECTION ( 'NONE',  ( 0.000000000000000000, 0.000000000000000000, 1.000000000000000000 ) ) ;
#20236 = CYLINDRICAL_SURFACE ( 'NONE', #50205, 9.550761578869391144 ) ;
#20237 = CARTESIAN_POINT ( 'NONE',  ( -45.62203281981695113, -277.9572555538766210, -346.8051306091561514 ) ) ;
#20238 = ORIENTED_EDGE ( 'NONE', *, *, #18555, .T. ) ;
#20239 = ORIENTED_EDGE ( 'NONE', *, *, #12108, .F. ) ;
#20240 = DIRECTION ( 'NONE',  ( 0.000000000000000000, 1.000000000000000000, -0.000000000000000000 ) ) ;
#20241 = CARTESIAN_POINT ( 'NONE',  ( -92.21611822576460327, -285.8115205227973661, -322.0250182851863769 ) ) ;
#20242 = CARTESIAN_POINT ( 'NONE',  ( 24.55843368802369397, -293.2880014324734361, -309.4559428039779618 ) ) ;
#20243 = CARTESIAN_POINT ( 'NONE',  ( -46.02251494838112222, -288.5079465466793636, -346.8206942528800596 ) ) ;
#20244 = EDGE_CURVE ( 'NONE', #11198, #46065, #82036, .T. ) ;
#20245 = CARTESIAN_POINT ( 'NONE',  ( -70.41540975968770510, -283.8499598856743091, -204.1344171334308442 ) ) ;
#20246 = B_SPLINE_CURVE_WITH_KNOTS ( 'NONE', 3,
 ( #72341, #57671, #14588, #36808, #86990, #22590, #50555, #15036, #363, #8389, #87903, #15973, #43896, #7460, #80354, #15495, #44366, #37268, #16428, #29249, #73729, #81282, #65728, #73277 ),
 .UNSPECIFIED., .F., .F.,
 ( 4, 2, 2, 2, 2, 2, 2, 2, 2, 2, 2, 4 ),
 ( 5.000000000000000311E-10, 0.06250000043739493971, 0.1250000003747898936, 0.2500000002495797458, 0.3750000001243696812, 0.4999999999991595057, 0.6249999998739494966, 0.7499999997487395431, 0.8124999996861346219, 0.8749999996235297006, 0.9374999995609246684, 0.9999999994983197471 ),
 .UNSPECIFIED. ) ;
#20248 = CARTESIAN_POINT ( 'NONE',  ( 14.78133465449043804, -286.5452018655301458, -322.9078900774871386 ) ) ;
#20247 = CARTESIAN_POINT ( 'NONE',  ( -101.4961819897355326, -283.6174466731628172, -234.2070815833755830 ) ) ;
#20249 = CARTESIAN_POINT ( 'NONE',  ( -29.38644591958286867, -284.1543610972602210, -343.3765760133306912 ) ) ;
#20250 = CARTESIAN_POINT ( 'NONE',  ( -4.884051664691080319, -274.6246261236256032, -337.9881186185056663 ) ) ;
#20251 = CARTESIAN_POINT ( 'NONE',  ( 9.336930237074478001, -285.0815183135947564, -210.1320064114818820 ) ) ;
#20252 = CARTESIAN_POINT ( 'NONE',  ( -36.24728794247184283, -300.0660086204491108, -195.3607361450893904 ) ) ;
#20253 = CARTESIAN_POINT ( 'NONE',  ( -100.9530954106502918, -283.0891964050535421, -230.3159083355264158 ) ) ;
#20254 = CARTESIAN_POINT ( 'NONE',  ( 21.51093134818863462, -281.8839828914335612, -226.7535934818088492 ) ) ;
#20255 = CARTESIAN_POINT ( 'NONE',  ( 24.03308083390703231, -288.9637462017158214, -226.9434909888439904 ) ) ;
#20256 = DIRECTION ( 'NONE',  ( 0.3024135303179589229, 0.9531768234071938961, 0.000000000000000000 ) ) ;
#20257 = CYLINDRICAL_SURFACE ( 'NONE', #76085, 2.999999999999993783 ) ;
#20258 = CARTESIAN_POINT ( 'NONE',  ( 3.470481103912061105, -296.4285759718682698, -334.0126682316591769 ) ) ;
#20259 = CARTESIAN_POINT ( 'NONE',  ( -69.35447072460878815, -277.6307593900839947, -202.5364678026601268 ) ) ;
#20260 = CARTESIAN_POINT ( 'NONE',  ( -98.90590571253842711, -289.1361088475414931, -316.3612160950274870 ) ) ;
#20261 = CARTESIAN_POINT ( 'NONE',  ( -42.46538574669811794, -293.5177172726479284, -343.9830458395301775 ) ) ;
#20262 = CARTESIAN_POINT ( 'NONE',  ( -1.712431984400921925, -279.2196941532208712, -206.0820488370908663 ) ) ;
#20263 = CARTESIAN_POINT ( 'NONE',  ( -101.9557794382960054, -271.1299254082481411, -233.2935517564702081 ) ) ;
#20264 = CARTESIAN_POINT ( 'NONE',  ( 6.960275742959275647, -293.9849750373294341, -211.7217249899602223 ) ) ;
#20265 = CARTESIAN_POINT ( 'NONE',  ( -106.6379572354042153, -292.6233781216987495, -303.7686719486574134 ) ) ;
#20266 = CARTESIAN_POINT ( 'NONE',  ( -67.88201864047690037, -296.1385260511578394, -200.3763282158968195 ) ) ;
#20267 = CARTESIAN_POINT ( 'NONE',  ( 10.65080245116904756, -289.9764879404780800, -326.4925973908365222 ) ) ;
#20268 = CARTESIAN_POINT ( 'NONE',  ( 37.07415536079328433, -291.5964136802967346, -254.9266840776168692 ) ) ;
#20269 = ADVANCED_FACE ( 'NONE', ( #36757 ), #80551, .T. ) ;
#20270 = CARTESIAN_POINT ( 'NONE',  ( -97.82291620412300404, -291.3977410869941309, -312.3045731723368021 ) ) ;
#20271 = EDGE_CURVE ( 'NONE', #29017, #74706, #6501, .T. ) ;
#20272 = DIRECTION ( 'NONE',  ( 0.000000000000000000, 0.000000000000000000, -1.000000000000000000 ) ) ;
#20273 = CARTESIAN_POINT ( 'NONE',  ( -60.31935898979723731, -292.5494406911891474, -200.8484088883652419 ) ) ;
#20274 = CARTESIAN_POINT ( 'NONE',  ( 194.5881128153457098, 0.000000000000000000, 10.00000000000000178 ) ) ;
#20275 = CARTESIAN_POINT ( 'NONE',  ( -96.28323037451396260, -292.4187085568170232, -221.4132961256111685 ) ) ;
#20277 = CARTESIAN_POINT ( 'NONE',  ( 34.48317378039007508, -293.3791421944624744, -257.2460165173690712 ) ) ;
#20276 = CARTESIAN_POINT ( 'NONE',  ( 37.17225381297330244, -279.4244343820826657, -258.7935268516100678 ) ) ;
#20278 = CIRCLE ( 'NONE', #3637, 4.000000000000003553 ) ;
#20279 = CARTESIAN_POINT ( 'NONE',  ( 12.99217136191258959, -280.7327945145713102, -212.0901871436865633 ) ) ;
#20280 = CARTESIAN_POINT ( 'NONE',  ( -44.42149925063706917, -282.8059782237352806, -347.0670586021096824 ) ) ;
#20281 = CARTESIAN_POINT ( 'NONE',  ( -83.70149274560351671, -287.6899482708562914, -329.1046116803624386 ) ) ;
#20282 = CARTESIAN_POINT ( 'NONE',  ( 24.72811970642363377, -279.1355028338772968, -229.5473350224219473 ) ) ;
#20283 = CARTESIAN_POINT ( 'NONE',  ( -99.32875553787344813, -283.1247177520060063, -228.0485062650273562 ) ) ;
#20284 = APPLICATION_CONTEXT ( 'automotive_design' ) ;
#20285 = CARTESIAN_POINT ( 'NONE',  ( 82.64890176555634582, -299.5541904835127980, -197.2582414438974183 ) ) ;
#20286 = CARTESIAN_POINT ( 'NONE',  ( 34.67978178036037207, -279.7093679855465211, -244.9918006069261480 ) ) ;
#20287 = CIRCLE ( 'NONE', #86766, 2.046895004029262832 ) ;
#20288 = CARTESIAN_POINT ( 'NONE',  ( 37.08020550198332188, -286.2398930654125024, -251.8443020218966808 ) ) ;
#20289 = CARTESIAN_POINT ( 'NONE',  ( 196.2170728810764615, 41.80684193227733658, 13.58578709450668320 ) ) ;
#20290 = CARTESIAN_POINT ( 'NONE',  ( 32.55218939409179058, -294.8390308304022369, -246.5107223462067907 ) ) ;
#20291 = CARTESIAN_POINT ( 'NONE',  ( -1.593354834055566771, -275.9418614453367695, -202.8284436475601922 ) ) ;
#20292 = CARTESIAN_POINT ( 'NONE',  ( -96.90540231159040729, -277.6289693470893667, -312.6232530551527589 ) ) ;
#20293 = CARTESIAN_POINT ( 'NONE',  ( -50.56844179464368239, -292.0543754327635497, -194.5056415199272521 ) ) ;
#20294 = AXIS2_PLACEMENT_3D ( 'NONE', #83714, #26903, #69995 ) ;
#20295 = CARTESIAN_POINT ( 'NONE',  ( -98.63499239916552597, -282.0339844744931952, -314.6350897270917812 ) ) ;
#20296 = AXIS2_PLACEMENT_3D ( 'NONE', #30105, #72724, #45209 ) ;
#20297 = CARTESIAN_POINT ( 'NONE',  ( -94.46693240886691001, -290.2567086306071928, -224.5141684049796709 ) ) ;
#20298 = CARTESIAN_POINT ( 'NONE',  ( 27.82397031902284112, -292.0482342373182405, -307.5932637264006644 ) ) ;
#20299 = ORIENTED_EDGE ( 'NONE', *, *, #63681, .F. ) ;
#20300 = CARTESIAN_POINT ( 'NONE',  ( 151.7270317713838210, 20.05858947365256739, 8.551724154028896407 ) ) ;
#20301 = CARTESIAN_POINT ( 'NONE',  ( -46.99639627251990248, -291.4338592455980006, -197.9402971924112933 ) ) ;
#20302 = CARTESIAN_POINT ( 'NONE',  ( 208.3233536746733989, 28.67700077860474295, 12.92477606492824904 ) ) ;
#20303 = CARTESIAN_POINT ( 'NONE',  ( 34.45848030099739390, -279.0523547857346784, -270.3937649182068412 ) ) ;
#20304 = CARTESIAN_POINT ( 'NONE',  ( -112.6554975795644822, -295.7980956059822688, -255.4392073734181281 ) ) ;
#20305 = CARTESIAN_POINT ( 'NONE',  ( 24.09162375906011988, -280.2895622214054470, -314.7255741764288359 ) ) ;
#20306 = CARTESIAN_POINT ( 'NONE',  ( -103.9791965945457264, -285.3752146068695765, -308.0548433018115588 ) ) ;
#20307 = CARTESIAN_POINT ( 'NONE',  ( 34.01022539348792151, -287.5896662920519020, -285.8438323092013889 ) ) ;
#20308 = CARTESIAN_POINT ( 'NONE',  ( 30.92757452963751064, -277.4420827589030409, -298.2461111548918780 ) ) ;
#20309 = CARTESIAN_POINT ( 'NONE',  ( -100.1302118997567305, -294.0248495407202540, -310.8222952834495914 ) ) ;
#20310 = CARTESIAN_POINT ( 'NONE',  ( -96.39954614722465465, -297.6939223965513861, -314.9930276175385870 ) ) ;
#20311 = AXIS2_PLACEMENT_3D ( 'NONE', #80602, #29513, #50811 ) ;
#20312 = CARTESIAN_POINT ( 'NONE',  ( -36.47681003665820754, -275.8360326052328446, -343.7656315442935693 ) ) ;
#20313 = ORIENTED_EDGE ( 'NONE', *, *, #45978, .T. ) ;
#20314 = CARTESIAN_POINT ( 'NONE',  ( 194.7788884907710099, 40.12874951497173015, 13.93756309559030981 ) ) ;
#20315 = CARTESIAN_POINT ( 'NONE',  ( -86.38511144096445094, -295.3786136268852829, -329.6948191837436752 ) ) ;
#20316 = CARTESIAN_POINT ( 'NONE',  ( -18.07772876651895899, -290.7222077603793196, -342.3189431944356897 ) ) ;
#20317 = CARTESIAN_POINT ( 'NONE',  ( 180.6209651459523968, 214.5000000000000568, -24.41176470588237635 ) ) ;
#20318 = CARTESIAN_POINT ( 'NONE',  ( 35.06248585260316020, -288.3375044101859430, -280.5283673644694318 ) ) ;
#20319 = ORIENTED_EDGE ( 'NONE', *, *, #48884, .T. ) ;
#20320 = CARTESIAN_POINT ( 'NONE',  ( -2.486235461489079590, -279.5605503510006429, -201.9511362877977376 ) ) ;
#20321 = CARTESIAN_POINT ( 'NONE',  ( -90.63544387885218612, -296.4348027574329763, -325.8698757792051310 ) ) ;
#20322 = CARTESIAN_POINT ( 'NONE',  ( -111.3637151172544861, -288.4863830695507545, -286.5180601888026217 ) ) ;
#20323 = CARTESIAN_POINT ( 'NONE',  ( -86.37858375892867002, -296.0450687006342037, -329.7002141604654071 ) ) ;
#20324 = CARTESIAN_POINT ( 'NONE',  ( 34.34594285037675121, -294.0686313189999055, -284.2524581280596863 ) ) ;
#20325 = DIRECTION ( 'NONE',  ( 0.000000000000000000, 0.000000000000000000, 1.000000000000000000 ) ) ;
#20326 = CARTESIAN_POINT ( 'NONE',  ( 196.0143093133015384, 73.40565171261609123, -11.99999999999998046 ) ) ;
#20327 = DIRECTION ( 'NONE',  ( -0.9565177946839406031, 0.000000000000000000, 0.2916739763039735700 ) ) ;
#20328 = CARTESIAN_POINT ( 'NONE',  ( 20.06419942736765805, -289.7587214170598031, -320.6527736922806753 ) ) ;
#20329 = CARTESIAN_POINT ( 'NONE',  ( -111.2586520408596868, -280.6233781216988064, -305.9938812882205070 ) ) ;
#20330 = CARTESIAN_POINT ( 'NONE',  ( 35.50984106711873522, -281.2130808109043869, -295.1429158361315785 ) ) ;
#20331 = CARTESIAN_POINT ( 'NONE',  ( -0.3234896261980607091, -284.5588246227664513, -335.3971120059162558 ) ) ;
#20332 = CARTESIAN_POINT ( 'NONE',  ( 32.18349895377764369, -285.7170984082435439, -238.5342635943641767 ) ) ;
#20333 = CARTESIAN_POINT ( 'NONE',  ( -101.5583311862220199, -288.1238534277226790, -308.1129103196010419 ) ) ;
#20334 = CARTESIAN_POINT ( 'NONE',  ( 2.866396278645666484, -278.3795293334136431, -334.6382620907512546 ) ) ;
#20335 = EDGE_LOOP ( 'NONE', ( #35505, #7301 ) ) ;
#20337 = CARTESIAN_POINT ( 'NONE',  ( -3.094003029295910867, -279.8657562179079150, -205.7637337317640345 ) ) ;
#20336 = CARTESIAN_POINT ( 'NONE',  ( -105.2677981959970737, -278.1945495722657142, -297.1014470992312795 ) ) ;
#20338 = CARTESIAN_POINT ( 'NONE',  ( -39.93865872692391150, -278.1636973334351524, -347.0210386357355787 ) ) ;
#20339 = CARTESIAN_POINT ( 'NONE',  ( -99.09860598740684168, -277.9523840343671282, -225.0168795927410486 ) ) ;
#20340 = CARTESIAN_POINT ( 'NONE',  ( -90.56249836145711640, -228.8796048916817938, -345.2664085948654247 ) ) ;
#20341 = CARTESIAN_POINT ( 'NONE',  ( -46.86372918164011736, -274.8752907586663241, -194.1892650757026502 ) ) ;
#20342 = EDGE_CURVE ( 'NONE', #10872, #68845, #23103, .T. ) ;
#20343 = CARTESIAN_POINT ( 'NONE',  ( -112.8610223001902426, -274.2148066845750236, -259.0666763222170630 ) ) ;
#20344 = CARTESIAN_POINT ( 'NONE',  ( -4.829096099716510437, -282.9805209788416391, -202.7746430608542312 ) ) ;
#20345 = CARTESIAN_POINT ( 'NONE',  ( 82.61707336526248469, -302.0539871969763226, -195.3101965168185075 ) ) ;
#20346 = CARTESIAN_POINT ( 'NONE',  ( 22.23478622320949682, -288.0362202097271620, -227.5570762895314658 ) ) ;
#20347 = CARTESIAN_POINT ( 'NONE',  ( -101.6726619282658248, -286.8488919766878098, -229.9197855791585141 ) ) ;
#20348 = CARTESIAN_POINT ( 'NONE',  ( 33.12973779667621699, -286.6443033693179814, -250.9274074458705570 ) ) ;
#20349 = CARTESIAN_POINT ( 'NONE',  ( -109.2476828459184759, -283.7114212697549647, -297.8785047394810022 ) ) ;
#20350 = CARTESIAN_POINT ( 'NONE',  ( -46.53614222585672167, -278.3335305031370126, -197.0844433046759150 ) ) ;
#20351 = CARTESIAN_POINT ( 'NONE',  ( 24.55101473945552115, -288.8522035838777811, -229.2783718491601519 ) ) ;
#20352 = CARTESIAN_POINT ( 'NONE',  ( 18.50247568030931689, -279.3534957848438580, -222.2570678281635139 ) ) ;
#20353 = CARTESIAN_POINT ( 'NONE',  ( -16.22324682259606732, -278.0886709919066107, -340.8080568013381253 ) ) ;
#20354 = CARTESIAN_POINT ( 'NONE',  ( 16.58080453554351408, -276.7512609193424851, -319.6783793734903156 ) ) ;
#20355 = CARTESIAN_POINT ( 'NONE',  ( -36.10870396393215742, -287.8319791788437669, -346.9671660871619565 ) ) ;
#20356 =( BOUNDED_SURFACE ( )  B_SPLINE_SURFACE ( 3, 2, ( 
 ( #25654, #67832, #61215 ),
 ( #10976, #47896, #32775 ),
 ( #38923, #90495, #76798 ),
 ( #25202, #11924, #55019 ),
 ( #26606, #74943, #76334 ),
 ( #40311, #39381, #19040 ) ),
 .UNSPECIFIED., .F., .F., .F. ) 
 B_SPLINE_SURFACE_WITH_KNOTS ( ( 4, 2, 4 ),
 ( 3, 3 ),
 ( -7.034303695085952768E-16, 0.001865377553711360711, 0.003730755107423424852 ),
 ( 0.000000000000000000, 1.000000000000000000 ),
 .UNSPECIFIED. ) 
 GEOMETRIC_REPRESENTATION_ITEM ( )  RATIONAL_B_SPLINE_SURFACE ( (
 ( 1.000000000000000000, 0.7905694150420948807, 1.000000000000000000),
 ( 1.000000000000000000, 0.7808937784651016623, 1.000000000000000000),
 ( 1.000000000000000000, 0.7692487437979422804, 1.000000000000000000),
 ( 1.000000000000000000, 0.7414446453488179323, 1.000000000000000000),
 ( 1.000000000000000000, 0.7251800859724746307, 1.000000000000000000),
 ( 1.000000000000000000, 0.7071067811865491270, 1.000000000000000000) ) ) 
 REPRESENTATION_ITEM ( '' )  SURFACE ( )  );
#20357 = CARTESIAN_POINT ( 'NONE',  ( -61.17186062352296716, -284.1565611471980333, -343.4665442839381626 ) ) ;
#20358 = CARTESIAN_POINT ( 'NONE',  ( -114.2653783477883280, -285.0850247193957898, -267.1232558986135928 ) ) ;
#20359 = CARTESIAN_POINT ( 'NONE',  ( -8.492288266139274455, -282.8303592510270050, -337.4186413467698458 ) ) ;
#20360 = ORIENTED_EDGE ( 'NONE', *, *, #64884, .T. ) ;
#20361 = ORIENTED_EDGE ( 'NONE', *, *, #8476, .F. ) ;
#20362 = CARTESIAN_POINT ( 'NONE',  ( 156.5440870305766055, 214.9910457053126720, 17.21343741151179429 ) ) ;
#20363 = CARTESIAN_POINT ( 'NONE',  ( -72.87571208577669779, -293.4469955150468650, -203.4312889108192053 ) ) ;
#20364 =( BOUNDED_SURFACE ( )  B_SPLINE_SURFACE ( 3, 2, ( 
 ( #74400, #60682, #59285 ),
 ( #89997, #82444, #82893 ),
 ( #30869, #9530, #46901 ),
 ( #66843, #25152, #54026 ),
 ( #38415, #10000, #23289 ),
 ( #52162, #39794, #81045 ) ),
 .UNSPECIFIED., .F., .F., .F. ) 
 B_SPLINE_SURFACE_WITH_KNOTS ( ( 4, 2, 4 ),
 ( 3, 3 ),
 ( 3.871320309816757899, 4.291854645100723786, 4.712388980384689674 ),
 ( 0.000000000000000000, 1.000000000000000000 ),
 .UNSPECIFIED. ) 
 GEOMETRIC_REPRESENTATION_ITEM ( )  RATIONAL_B_SPLINE_SURFACE ( (
 ( 1.000000000000000000, 0.7827533893364964079, 1.000000000000000000),
 ( 1.000000000000000000, 0.7737378266087827638, 1.000000000000000000),
 ( 1.000000000000000000, 0.7623946665074067264, 1.000000000000000000),
 ( 1.000000000000000000, 0.7365781863258152873, 1.000000000000000000),
 ( 1.000000000000000000, 0.7221049970984646516, 1.000000000000000000),
 ( 1.000000000000000000, 0.7071067811865487940, 1.000000000000000000) ) ) 
 REPRESENTATION_ITEM ( '' )  SURFACE ( )  );
#20365 = CARTESIAN_POINT ( 'NONE',  ( 10.82141655263135149, -291.3867604471241179, -210.8487498597131946 ) ) ;
#20366 = AXIS2_PLACEMENT_3D ( 'NONE', #74111, #15426, #29173 ) ;
#20367 = CARTESIAN_POINT ( 'NONE',  ( -110.1182556951474822, -271.7185119488624423, -262.1769009944317759 ) ) ;
#20368 = CARTESIAN_POINT ( 'NONE',  ( 22.20243145212455715, -293.5549947794885952, -319.0419260028627377 ) ) ;
#20369 = CARTESIAN_POINT ( 'NONE',  ( -111.0002282934223388, -288.9854729676389979, -273.9233504028511561 ) ) ;
#20370 = CARTESIAN_POINT ( 'NONE',  ( 9.507355118070325517, -290.9460687350726289, -212.9959346869703438 ) ) ;
#20371 = CARTESIAN_POINT ( 'NONE',  ( -104.4043105776840576, -291.3563450861241790, -300.3150304319308930 ) ) ;
#20372 = FACE_OUTER_BOUND ( 'NONE', #28244, .T. ) ;
#20373 = CARTESIAN_POINT ( 'NONE',  ( -112.1162529703692314, -292.4695425237663926, -276.8077118694866385 ) ) ;
#20374 = CARTESIAN_POINT ( 'NONE',  ( -111.9959173749538195, -288.4342144578347984, -279.5541570975560148 ) ) ;
#20375 = CARTESIAN_POINT ( 'NONE',  ( -111.8132970794172962, -292.4328340594520341, -279.6665501502061488 ) ) ;
#20376 = CARTESIAN_POINT ( 'NONE',  ( 17.94597146388631614, -287.8108963234392377, -222.3331904971062727 ) ) ;
#20377 = CARTESIAN_POINT ( 'NONE',  ( 35.30401363080866162, -295.3041644976250382, -251.0079314282764926 ) ) ;
#20378 = CARTESIAN_POINT ( 'NONE',  ( -114.1722217312759540, -271.7244848033647031, -270.3505797943694802 ) ) ;
#20379 = CARTESIAN_POINT ( 'NONE',  ( 207.5108682301385272, 1.050453206927881578, -7.446924052135294403 ) ) ;
#20380 = CARTESIAN_POINT ( 'NONE',  ( 23.97355982315887246, -276.9388371821778492, -226.5344224396591812 ) ) ;
#20381 = VECTOR ( 'NONE', #30789, 1000.000000000000000 ) ;
#20382 = CARTESIAN_POINT ( 'NONE',  ( -93.57827538333187078, -295.0339150718002657, -322.7408510826488737 ) ) ;
#20383 = CARTESIAN_POINT ( 'NONE',  ( -6.080875328583586814, -272.7086000561169499, -203.2736016389281701 ) ) ;
#20384 = CARTESIAN_POINT ( 'NONE',  ( -95.59490970013662547, -275.9899914341070257, -316.7266888545676693 ) ) ;
#20385 = CARTESIAN_POINT ( 'NONE',  ( -110.7393439293485642, -273.7929662064518084, -267.6377504097686710 ) ) ;
#20386 = CARTESIAN_POINT ( 'NONE',  ( -108.1649983417875944, -297.7153431090846993, -290.3469967014856365 ) ) ;
#20387 = CARTESIAN_POINT ( 'NONE',  ( 208.6208076322478746, 32.98517505407394168, 10.00000000000000000 ) ) ;
#20388 = CARTESIAN_POINT ( 'NONE',  ( -105.9608351776847144, -297.6943620034685978, -244.8374633001775464 ) ) ;
#20389 = LINE ( 'NONE', #76271, #80699 ) ;
#20391 = CARTESIAN_POINT ( 'NONE',  ( -40.51797094619345785, -298.0111363078657405, -197.4177026184339070 ) ) ;
#20390 = CARTESIAN_POINT ( 'NONE',  ( -4.189732732382841718, -284.5071157111722187, -202.6759742074747521 ) ) ;
#20392 = CARTESIAN_POINT ( 'NONE',  ( -40.81647239334181165, -286.0097118476170408, -193.3873677658204144 ) ) ;
#20393 = CARTESIAN_POINT ( 'NONE',  ( -73.16779326350092560, -289.1805869427522566, -338.5098221935239167 ) ) ;
#20394 = CARTESIAN_POINT ( 'NONE',  ( -77.35098809753694127, -299.4982394415907834, -206.5045311814060085 ) ) ;
#20395 = CARTESIAN_POINT ( 'NONE',  ( -28.70916093807228364, -292.9424050465045752, -344.7471701519687599 ) ) ;
#20396 = CARTESIAN_POINT ( 'NONE',  ( 12.89433644350913610, -279.9300911685031110, -212.2190553290860464 ) ) ;
#20397 = CARTESIAN_POINT ( 'NONE',  ( -37.37352853689063181, -292.5523547857347353, -345.3611179825600175 ) ) ;
#20398 = DIRECTION ( 'NONE',  ( 0.000000000000000000, 0.000000000000000000, -1.000000000000000000 ) ) ;
#20399 = CARTESIAN_POINT ( 'NONE',  ( 24.56506794068272725, -286.8893215445875171, -309.7905812284823810 ) ) ;
#20400 = EDGE_CURVE ( 'NONE', #40555, #65034, #12510, .T. ) ;
#20401 = CARTESIAN_POINT ( 'NONE',  ( 208.6208076322478746, 32.98517505407394168, 10.50000000000000000 ) ) ;
#20402 = CARTESIAN_POINT ( 'NONE',  ( -99.78969702237375827, -287.9905435754104701, -311.9206185007499812 ) ) ;
#20403 = CARTESIAN_POINT ( 'NONE',  ( -107.8656598809634630, -274.3547632669784662, -248.8067601240361739 ) ) ;
#20404 = CARTESIAN_POINT ( 'NONE',  ( -59.15145743101420095, -281.2005355267744449, -197.1290158828732046 ) ) ;
#20406 = CARTESIAN_POINT ( 'NONE',  ( 28.15106865862283669, -281.9904623679659039, -302.7201711499558314 ) ) ;
#20405 = CARTESIAN_POINT ( 'NONE',  ( -111.5878040651456757, -294.4038743814309100, -283.5376433228851170 ) ) ;
#20407 = CARTESIAN_POINT ( 'NONE',  ( -97.34768214340299153, -297.3654946523606100, -222.1088421096634704 ) ) ;
#20408 = CARTESIAN_POINT ( 'NONE',  ( -67.11706186295245402, -299.1747116739355192, -202.9371024031307797 ) ) ;
#20409 = EDGE_CURVE ( 'NONE', #75708, #83756, #76029, .T. ) ;
#20410 = CARTESIAN_POINT ( 'NONE',  ( 31.33118711821918012, -283.1575354286335369, -240.2109073186401247 ) ) ;
#20411 = CARTESIAN_POINT ( 'NONE',  ( -92.01258371637722178, -296.3054952123812882, -221.6322462927990955 ) ) ;
#20412 = VERTEX_POINT ( 'NONE', #23006 ) ;
#20413 = CYLINDRICAL_SURFACE ( 'NONE', #84660, 0.5000000000000004441 ) ;
#20414 = CARTESIAN_POINT ( 'NONE',  ( -29.24166137129510190, -284.9290526642578811, -344.6167773334036042 ) ) ;
#20415 = CARTESIAN_POINT ( 'NONE',  ( 142.6449502718966755, -27.00396092263537540, 22.50000000000000000 ) ) ;
#20416 = CARTESIAN_POINT ( 'NONE',  ( -69.91165696735023971, -286.9809262143061801, -337.9199732462171255 ) ) ;
#20417 = CARTESIAN_POINT ( 'NONE',  ( 39.21874136230186991, -274.8311757613735153, -276.8923980205372573 ) ) ;
#20418 = CARTESIAN_POINT ( 'NONE',  ( 10.93239676687030837, -292.5752655871932575, -215.5340840883249314 ) ) ;
#20419 = CARTESIAN_POINT ( 'NONE',  ( 24.72474253690069190, -283.6178104478464093, -310.1848575823437386 ) ) ;
#20420 = CARTESIAN_POINT ( 'NONE',  ( 32.81603944175314780, -276.8497865366781525, -247.2985686333061039 ) ) ;
#20421 = CARTESIAN_POINT ( 'NONE',  ( -61.03161698088980813, -284.7789006027329037, -343.0620464176307109 ) ) ;
#20422 = CARTESIAN_POINT ( 'NONE',  ( -3.451609935358393333, -281.3892701338144775, -335.4796701952996614 ) ) ;
#20423 = CARTESIAN_POINT ( 'NONE',  ( -88.92415308158687992, -281.3280777168766349, -215.8443851696565332 ) ) ;
#20424 = CARTESIAN_POINT ( 'NONE',  ( -71.40471085081489377, -273.7813799926016145, -201.3052615688016544 ) ) ;
#20425 = CARTESIAN_POINT ( 'NONE',  ( 29.09487630824069626, -275.8921433325166959, -309.2864479864536520 ) ) ;
#20426 = CARTESIAN_POINT ( 'NONE',  ( 4.648432004541546370, -296.4005354107971471, -331.8277186633598603 ) ) ;
#20427 = VECTOR ( 'NONE', #9899, 1000.000000000000000 ) ;
#20428 = DIRECTION ( 'NONE',  ( -1.000000000000000000, -0.000000000000000000, -0.000000000000000000 ) ) ;
#20429 = CARTESIAN_POINT ( 'NONE',  ( 153.6987871352711181, 19.48326534539917887, -11.45812909362560639 ) ) ;
#20430 = CARTESIAN_POINT ( 'NONE',  ( -104.8677544210669907, -294.2407672179093652, -304.8357088850556238 ) ) ;
#20431 = CARTESIAN_POINT ( 'NONE',  ( 24.03267669443869892, -275.6092042692771429, -310.0924314130461426 ) ) ;
#20432 = AXIS2_PLACEMENT_3D ( 'NONE', #14044, #26375, #34415 ) ;
#20433 = CARTESIAN_POINT ( 'NONE',  ( -3.518533633770426050, -296.1340106258576839, -338.7766237963248273 ) ) ;
#20434 = CARTESIAN_POINT ( 'NONE',  ( 21.07485016374559095, -295.4286133554568323, -319.9142750130876607 ) ) ;
#20435 = CARTESIAN_POINT ( 'NONE',  ( -109.8920098641454075, -292.7890840106984456, -251.9655124535315451 ) ) ;
#20436 = CARTESIAN_POINT ( 'NONE',  ( -79.68995846552437001, -275.6253767907149381, -332.1223138632049086 ) ) ;
#20437 = CARTESIAN_POINT ( 'NONE',  ( -95.93925932665489142, -281.1072399395815751, -224.4315488720263829 ) ) ;
#20438 = CARTESIAN_POINT ( 'NONE',  ( -64.10919113912578382, -293.4837654725556035, -339.8766338976153634 ) ) ;
#20439 = CARTESIAN_POINT ( 'NONE',  ( 35.40695193088384940, -283.1422870585941496, -249.1500865670410860 ) ) ;
#20440 = CIRCLE ( 'NONE', #67344, 24.00000000000001066 ) ;
#20441 = CARTESIAN_POINT ( 'NONE',  ( -42.68298839893505914, -284.9035396823200017, -197.2341673077121413 ) ) ;
#20442 = CARTESIAN_POINT ( 'NONE',  ( 191.3483536179935811, 269.5978400234172909, -139.1112103393494408 ) ) ;
#20443 = ORIENTED_EDGE ( 'NONE', *, *, #15864, .F. ) ;
#20444 = CARTESIAN_POINT ( 'NONE',  ( -109.0010619064832156, -284.0337586821974014, -284.3976188413744239 ) ) ;
#20445 = VERTEX_POINT ( 'NONE', #51884 ) ;
#20446 = CARTESIAN_POINT ( 'NONE',  ( -0.5117588490551993052, -283.6541554314484870, -337.6444748426573028 ) ) ;
#20447 = CARTESIAN_POINT ( 'NONE',  ( -106.3148956329049071, -283.7769125809925299, -237.0338465774220253 ) ) ;
#20448 = CARTESIAN_POINT ( 'NONE',  ( -111.5967773064131876, -279.2483762994376661, -289.8807546587031538 ) ) ;
#20449 = CLOSED_SHELL ( 'NONE', ( #27401, #8136, #58097, #83433, #447, #23737, #3367, #41920, #88676, #10909, #93028, #88549, #21965, #23016 ) ) ;
#20450 = CARTESIAN_POINT ( 'NONE',  ( -112.3802523404528984, -279.8965311945877943, -284.2864536832291833 ) ) ;
#20451 = CARTESIAN_POINT ( 'NONE',  ( 24.50481641118622278, -281.5954315467186575, -224.6629650787219532 ) ) ;
#20452 = CARTESIAN_POINT ( 'NONE',  ( -6.941161984400256557, -271.9809262143061233, -207.3071070584150277 ) ) ;
#20453 = CARTESIAN_POINT ( 'NONE',  ( 140.1412609228563042, 179.8917986951376236, -241.4356369855332787 ) ) ;
#20454 = ORIENTED_EDGE ( 'NONE', *, *, #88734, .F. ) ;
#20455 = CARTESIAN_POINT ( 'NONE',  ( 24.55475842122751828, -276.9814485145686831, -228.2803643704477281 ) ) ;
#20456 = CARTESIAN_POINT ( 'NONE',  ( -84.51206451544574350, -219.2010842044853689, -352.3091733033897981 ) ) ;
#20457 = CARTESIAN_POINT ( 'NONE',  ( -41.10955073043210461, -278.0245956044685158, -195.8114693833978492 ) ) ;
#20458 = CARTESIAN_POINT ( 'NONE',  ( 35.31145055632104857, -295.0290512471046327, -248.1014299877745941 ) ) ;
#20459 = CARTESIAN_POINT ( 'NONE',  ( 33.74883734666483548, -292.6757340138491941, -253.2774021417273502 ) ) ;
#20460 = CARTESIAN_POINT ( 'NONE',  ( -73.15079238616165469, -289.0215466378542146, -338.4731157773885002 ) ) ;
#20461 = CARTESIAN_POINT ( 'NONE',  ( 175.2296996224750103, 214.5000000000000568, 0.000000000000000000 ) ) ;
#20462 = EDGE_CURVE ( 'NONE', #92893, #48357, #80777, .T. ) ;
#20464 = CARTESIAN_POINT ( 'NONE',  ( -14.29706308860500741, -284.7557386602671841, -200.1977050575218300 ) ) ;
#20463 = CARTESIAN_POINT ( 'NONE',  ( 15.06130190458702067, -292.9046557263863519, -325.9716535823719141 ) ) ;
#20465 = CARTESIAN_POINT ( 'NONE',  ( -105.8520131514659681, -292.7912150865183776, -241.6404922226025178 ) ) ;
#20466 = ADVANCED_FACE ( 'NONE', ( #42936 ), #57170, .F. ) ;
#20467 = CARTESIAN_POINT ( 'NONE',  ( -110.5858853170589100, -285.7881341990832880, -276.4053559942871630 ) ) ;
#20468 = ORIENTED_EDGE ( 'NONE', *, *, #43976, .T. ) ;
#20469 = CARTESIAN_POINT ( 'NONE',  ( -73.33403450289934256, -292.5279801310514358, -202.5423389306555180 ) ) ;
#20470 = CARTESIAN_POINT ( 'NONE',  ( -16.10863393030117052, -283.2624068247573064, -340.2692386936687399 ) ) ;
#20471 = CARTESIAN_POINT ( 'NONE',  ( 10.93610531442968892, -293.1964200974447294, -329.9043511323453686 ) ) ;
#20472 = CARTESIAN_POINT ( 'NONE',  ( 31.54719535292074895, -288.7946355083011554, -304.5175835615713140 ) ) ;
#20473 = CARTESIAN_POINT ( 'NONE',  ( -57.26890966671346206, -289.7948203679932249, -344.7292534169084206 ) ) ;
#20474 = CARTESIAN_POINT ( 'NONE',  ( 20.35877036529091555, -288.3488345981965040, -315.0988680951542733 ) ) ;
#20475 = VERTEX_POINT ( 'NONE', #71845 ) ;
#20476 = DIRECTION ( 'NONE',  ( -0.3994899938747922263, 0.000000000000000000, 0.9167375550253837879 ) ) ;
#20477 = CARTESIAN_POINT ( 'NONE',  ( -112.5515424773979731, -298.5289093366816928, -261.2076982133957586 ) ) ;
#20478 = CARTESIAN_POINT ( 'NONE',  ( -59.98604504535602899, -296.4496552780331626, -197.2270128695543292 ) ) ;
#20479 = CARTESIAN_POINT ( 'NONE',  ( -38.34507198342080869, -279.0980197211071641, -197.1202562168407724 ) ) ;
#20480 = CARTESIAN_POINT ( 'NONE',  ( -24.16397506914693238, -273.7236238496915917, -194.5054476279020719 ) ) ;
#20481 = EDGE_CURVE ( 'NONE', #26669, #13683, #83518, .T. ) ;
#20482 = CARTESIAN_POINT ( 'NONE',  ( -20.71034507222360332, -293.3147647427265952, -342.2058151733558020 ) ) ;
#20483 = CARTESIAN_POINT ( 'NONE',  ( 34.57644041368872934, -277.5404733683647578, -287.9004279230227326 ) ) ;
#20484 = CARTESIAN_POINT ( 'NONE',  ( -66.27305071856305574, -271.8088978262707087, -201.9956118050231453 ) ) ;
#20485 = CARTESIAN_POINT ( 'NONE',  ( -35.62603008020256823, -296.2352632241772312, -343.7507013140864274 ) ) ;
#20486 = CARTESIAN_POINT ( 'NONE',  ( -47.82369977251103421, -296.2681204860084563, -342.9684803419327181 ) ) ;
#20487 = FACE_OUTER_BOUND ( 'NONE', #74806, .T. ) ;
#20488 = CARTESIAN_POINT ( 'NONE',  ( -81.39244645041365800, -297.2399530912869068, -332.6024950123676831 ) ) ;
#20489 = CARTESIAN_POINT ( 'NONE',  ( -99.22646076874328003, -295.1292966932009563, -227.6734785380151607 ) ) ;
#20490 = CARTESIAN_POINT ( 'NONE',  ( -20.05609399799226722, -292.9314918050943675, -199.2799061855964453 ) ) ;
#20491 = CARTESIAN_POINT ( 'NONE',  ( -113.7033333701804878, -273.4621055185214686, -261.8136160753545028 ) ) ;
#20492 = CARTESIAN_POINT ( 'NONE',  ( -90.22726264439558008, -289.8604473470688845, -219.1899132447925354 ) ) ;
#20493 = CARTESIAN_POINT ( 'NONE',  ( -55.32532138856537784, -274.3191160726446469, -195.5539240142365145 ) ) ;
#20494 = CARTESIAN_POINT ( 'NONE',  ( -101.2351153521751570, -297.3684484705749469, -235.0097534021477372 ) ) ;
#20495 = CARTESIAN_POINT ( 'NONE',  ( 16.03975319350223216, -282.7838889098434834, -217.1012560017240105 ) ) ;
#20496 = CARTESIAN_POINT ( 'NONE',  ( -3.858216683970966177, -279.1694462342545648, -201.5560330292473736 ) ) ;
#20497 = CARTESIAN_POINT ( 'NONE',  ( -66.54523214032158762, -282.7733014816466834, -341.5122418298900584 ) ) ;
#20498 = CARTESIAN_POINT ( 'NONE',  ( 21.64709106172834652, -275.5655154088543100, -319.6930072728634400 ) ) ;
#20499 = CARTESIAN_POINT ( 'NONE',  ( 36.90270245428426676, -279.7346075005963257, -253.1511964099847773 ) ) ;
#20500 = CARTESIAN_POINT ( 'NONE',  ( 21.08182723941909131, -280.2018833302793723, -317.6753896169302038 ) ) ;
#20501 = CARTESIAN_POINT ( 'NONE',  ( -67.28073941702785987, -272.2264205976156859, -203.1235940001424183 ) ) ;
#20502 = CARTESIAN_POINT ( 'NONE',  ( -35.01683794608413081, -279.0231413477883393, -345.3376455229458202 ) ) ;
#20503 = CARTESIAN_POINT ( 'NONE',  ( 121.3395553409046670, -299.5541904835127980, -195.3611179825600175 ) ) ;
#20504 = DIRECTION ( 'NONE',  ( 0.000000000000000000, 0.000000000000000000, -1.000000000000000000 ) ) ;
#20505 = CARTESIAN_POINT ( 'NONE',  ( -3.942567235151725580, -296.7046938696523171, -194.3842891811289917 ) ) ;
#20506 = CARTESIAN_POINT ( 'NONE',  ( -41.92811500392247837, -290.0147222715382895, -195.1456169040285431 ) ) ;
#20507 = CARTESIAN_POINT ( 'NONE',  ( -88.64948411077057244, -291.3553147882960843, -212.9458647584758637 ) ) ;
#20508 = CARTESIAN_POINT ( 'NONE',  ( 200.2296996224750103, 66.43830042146294090, -4.834471782559336933E-14 ) ) ;
#20509 = CARTESIAN_POINT ( 'NONE',  ( 36.91245703652465693, -277.4016548826752455, -258.6014898098471804 ) ) ;
#20510 = CARTESIAN_POINT ( 'NONE',  ( 32.03429725566758890, -273.1786910845457896, -241.7295174292877107 ) ) ;
#20511 = CARTESIAN_POINT ( 'NONE',  ( 191.4749582765727212, -21.37379927922774314, 13.00000000000000178 ) ) ;
#20512 = CARTESIAN_POINT ( 'NONE',  ( 36.73867465573334101, -283.6619425252267206, -285.2410465099249564 ) ) ;
#20513 = FILL_AREA_STYLE_COLOUR ( '', #22966 ) ;
#20514 = CARTESIAN_POINT ( 'NONE',  ( -109.0741376417059172, -282.8362388024168013, -248.2923273916712219 ) ) ;
#20515 = VECTOR ( 'NONE', #70891, 1000.000000000000000 ) ;
#20516 = CARTESIAN_POINT ( 'NONE',  ( 197.2126074028028313, 40.90928511441033777, 12.12147092472265264 ) ) ;
#20517 = CARTESIAN_POINT ( 'NONE',  ( 4.027608214087640803, -293.2758089049786463, -330.9887588017700182 ) ) ;
#20518 = CARTESIAN_POINT ( 'NONE',  ( -9.000254227003669172, -284.5663571159282128, -201.7352234822287755 ) ) ;
#20519 = CARTESIAN_POINT ( 'NONE',  ( 159.4572718888341569, 15.57755555264324521, -9.020884447463142664 ) ) ;
#20520 = CARTESIAN_POINT ( 'NONE',  ( -17.72116012565841814, -292.7989158357086126, -342.7492044050287632 ) ) ;
#20521 = CARTESIAN_POINT ( 'NONE',  ( -91.95118824806618818, -282.2943464781878902, -323.6575677650159832 ) ) ;
#20522 = CARTESIAN_POINT ( 'NONE',  ( -95.43306958051316258, -280.7872660989660858, -224.8233755152020876 ) ) ;
#20523 = CARTESIAN_POINT ( 'NONE',  ( -112.6110239454851012, -285.9395592664937453, -255.8532544176854628 ) ) ;
#20524 = CARTESIAN_POINT ( 'NONE',  ( 28.42095924687072639, -279.2903717269009007, -232.2921457894609603 ) ) ;
#20525 = CARTESIAN_POINT ( 'NONE',  ( -8.254947446710065861, -286.4439793904407452, -203.4062016697698425 ) ) ;
#20526 = CARTESIAN_POINT ( 'NONE',  ( -109.3375112250729728, -279.7781157698582888, -285.5919453840065216 ) ) ;
#20527 = CARTESIAN_POINT ( 'NONE',  ( -98.13347169816687199, -279.9201761581308574, -229.5653423659223336 ) ) ;
#20528 = CARTESIAN_POINT ( 'NONE',  ( -90.75528151023307544, -287.2790405708038861, -217.2066626127095219 ) ) ;
#20529 = ORIENTED_EDGE ( 'NONE', *, *, #44158, .F. ) ;
#20530 = CARTESIAN_POINT ( 'NONE',  ( -35.82601815709919890, -297.9039588445401705, -193.3611594079439442 ) ) ;
#20531 = CARTESIAN_POINT ( 'NONE',  ( -39.99162214153800221, -291.0653794007516808, -345.0095633290131900 ) ) ;
#20532 = DIRECTION ( 'NONE',  ( 0.9531768234072897084, -0.3024135303176576084, 0.000000000000000000 ) ) ;
#20533 = CARTESIAN_POINT ( 'NONE',  ( -106.6662871844225293, -275.4805209788417528, -237.0123917617630980 ) ) ;
#20534 = ORIENTED_EDGE ( 'NONE', *, *, #20150, .T. ) ;
#20535 = CARTESIAN_POINT ( 'NONE',  ( -36.92372284428714124, -272.0572502180299352, -195.1828672871213541 ) ) ;
#20536 = CARTESIAN_POINT ( 'NONE',  ( 37.54287019753216015, -291.7738682656586775, -256.2635457052647894 ) ) ;
#20537 = CARTESIAN_POINT ( 'NONE',  ( -35.13913671767085845, -297.5881088752313417, -197.2997692740603952 ) ) ;
#20538 = CARTESIAN_POINT ( 'NONE',  ( -87.18420506855721896, -291.2815427122679353, -324.7113769294397230 ) ) ;
#20540 = EDGE_CURVE ( 'NONE', #23299, #135, #53306, .T. ) ;
#20539 = CARTESIAN_POINT ( 'NONE',  ( 35.22863737886870439, -283.5023556844174664, -284.9687244640829817 ) ) ;
#20541 = CARTESIAN_POINT ( 'NONE',  ( -96.00209079540667290, -291.2018441956485617, -319.4961638596646480 ) ) ;
#20542 = CARTESIAN_POINT ( 'NONE',  ( -112.3091949344336484, -286.5806676303881773, -268.1530943802150091 ) ) ;
#20543 = CARTESIAN_POINT ( 'NONE',  ( -35.33815598716348916, -280.2432961900918826, -193.3740517007247206 ) ) ;
#20544 = CARTESIAN_POINT ( 'NONE',  ( -47.46333827471196543, -293.2596920061812966, -345.2401313140499610 ) ) ;
#20545 = CARTESIAN_POINT ( 'NONE',  ( 32.39148862436221066, -281.8050054480718245, -303.1407087741107489 ) ) ;
#20546 = CARTESIAN_POINT ( 'NONE',  ( 36.81959874666089405, -277.3565715043815203, -266.0439140182618303 ) ) ;
#20547 = CARTESIAN_POINT ( 'NONE',  ( 30.89617123739170168, -277.8376638359844719, -254.7536222014695397 ) ) ;
#20548 = CARTESIAN_POINT ( 'NONE',  ( 38.60947445830576896, -273.8383533252995790, -274.0178505739139609 ) ) ;
#20549 = DIRECTION ( 'NONE',  ( 0.000000000000000000, 0.000000000000000000, -1.000000000000000000 ) ) ;
#20550 = CARTESIAN_POINT ( 'NONE',  ( 17.11286042825096132, -280.3635147099731171, -221.6508595519935056 ) ) ;
#20551 = CARTESIAN_POINT ( 'NONE',  ( -34.29146492694944470, -278.2196694269658224, -346.9032944910129004 ) ) ;
#20552 = CARTESIAN_POINT ( 'NONE',  ( -5.106770209196980659, -275.8007882320975455, -204.3006068977298071 ) ) ;
#20553 = CARTESIAN_POINT ( 'NONE',  ( -114.1054157559419195, -283.6157953064064827, -269.9710214781242144 ) ) ;
#20554 = CARTESIAN_POINT ( 'NONE',  ( -107.5393938696417564, -292.6195669391524916, -246.9035433754005737 ) ) ;
#20555 = CARTESIAN_POINT ( 'NONE',  ( -57.92531130860410826, -275.3908608601349783, -196.9390011479957820 ) ) ;
#20556 = CARTESIAN_POINT ( 'NONE',  ( -113.8485494440449202, -273.8671145182713076, -270.3778261331385124 ) ) ;
#20557 = FACE_BOUND ( 'NONE', #43970, .T. ) ;
#20558 = CARTESIAN_POINT ( 'NONE',  ( -110.8512665761547851, -298.7335213448432683, -256.2794686918437606 ) ) ;
#20559 = CARTESIAN_POINT ( 'NONE',  ( -59.51506101398956616, -281.3396374703711444, -341.8884658692127800 ) ) ;
#20560 = CARTESIAN_POINT ( 'NONE',  ( -72.15890625234015943, -291.2710885767406239, -201.6915418408783296 ) ) ;
#20561 = CARTESIAN_POINT ( 'NONE',  ( 16.77332832658423456, -274.2971306752575060, -321.7752259495853764 ) ) ;
#20562 = CARTESIAN_POINT ( 'NONE',  ( -20.65157451555334589, -290.4415928164342517, -344.7649358072233099 ) ) ;
#20563 = CARTESIAN_POINT ( 'NONE',  ( -60.34296287108740131, -290.6672399465470562, -200.7006164639592498 ) ) ;
#20564 = ORIENTED_EDGE ( 'NONE', *, *, #13930, .T. ) ;
#20565 = CARTESIAN_POINT ( 'NONE',  ( -112.0599370379590169, -289.3291897885905541, -254.3059781325443964 ) ) ;
#20566 = CARTESIAN_POINT ( 'NONE',  ( -108.1279254967938925, -290.4560197681713021, -252.3827060009795105 ) ) ;
#20567 = ORIENTED_EDGE ( 'NONE', *, *, #34464, .F. ) ;
#20568 = CARTESIAN_POINT ( 'NONE',  ( 35.55091329399895272, -288.3287971700274284, -246.3552834759147743 ) ) ;
#20569 = CARTESIAN_POINT ( 'NONE',  ( -109.3061973778969360, -278.7212299547822454, -282.8123436188760707 ) ) ;
#20570 = CARTESIAN_POINT ( 'NONE',  ( -69.41123858578896488, -294.3846748009860903, -340.0392384753142210 ) ) ;
#20571 = CARTESIAN_POINT ( 'NONE',  ( -114.2526729939563239, -285.1723432283396278, -272.8542163725981027 ) ) ;
#20572 = CARTESIAN_POINT ( 'NONE',  ( -113.8823868297742621, -284.7828308592328312, -278.5627989511127112 ) ) ;
#20573 = CARTESIAN_POINT ( 'NONE',  ( -3.607841525799501792, -282.9273782984321315, -335.1371091619191134 ) ) ;
#20574 = CARTESIAN_POINT ( 'NONE',  ( -48.09564758678637730, -154.9642027764678289, -365.2473460210824214 ) ) ;
#20575 = CARTESIAN_POINT ( 'NONE',  ( -105.0018845002311565, -254.6799856396871462, -325.8108064456704938 ) ) ;
#20576 = CARTESIAN_POINT ( 'NONE',  ( -48.36594557731149280, -154.7337953574015899, -361.4374211060301718 ) ) ;
#20577 = CARTESIAN_POINT ( 'NONE',  ( -110.5027959604814072, -271.7853810092052527, -267.6210354056324263 ) ) ;
#20578 = CARTESIAN_POINT ( 'NONE',  ( 9.693896526445993089, -273.6373114254649863, -214.0640462950258893 ) ) ;
#20579 = CARTESIAN_POINT ( 'NONE',  ( 11.15465836344534800, -293.9090339482976333, -330.1594115452946880 ) ) ;
#20580 = CARTESIAN_POINT ( 'NONE',  ( -61.85293824084561720, -183.3176616290708978, -359.0448971616088443 ) ) ;
#20581 = ADVANCED_FACE ( 'NONE', ( #66580 ), #1700, .F. ) ;
#20582 = CARTESIAN_POINT ( 'NONE',  ( -102.2914863981954028, -271.7693718857182716, -229.9281668713755380 ) ) ;
#20583 = CARTESIAN_POINT ( 'NONE',  ( -80.46449502298644063, -299.3210897720525736, -209.9352126245723866 ) ) ;
#20584 = EDGE_CURVE ( 'NONE', #71834, #31036, #54802, .T. ) ;
#20585 = CARTESIAN_POINT ( 'NONE',  ( -69.16416843489774635, -292.7031567126353480, -204.3051734595368316 ) ) ;
#20586 = ORIENTED_EDGE ( 'NONE', *, *, #2931, .F. ) ;
#20587 = CARTESIAN_POINT ( 'NONE',  ( -65.46699705325973184, -298.6346813656243739, -198.8774979795657885 ) ) ;
#20588 = CARTESIAN_POINT ( 'NONE',  ( 35.71677250282696292, -288.0533248545674496, -271.0304596698283603 ) ) ;
#20589 = CARTESIAN_POINT ( 'NONE',  ( -30.59492504527749901, -295.7717194548351927, -346.9028702906401804 ) ) ;
#20590 = CARTESIAN_POINT ( 'NONE',  ( -8.405358854199741714, -295.1758240623362894, -341.7072127273230535 ) ) ;
#20591 = CARTESIAN_POINT ( 'NONE',  ( 22.58672043617612601, -293.1375790046675434, -228.6547514383005932 ) ) ;
#20592 = EDGE_LOOP ( 'NONE', ( #29508, #68190, #59002, #61897 ) ) ;
#20593 = CARTESIAN_POINT ( 'NONE',  ( 20.72819778475617625, -276.8096241888264899, -222.0165096189973610 ) ) ;
#20594 = ORIENTED_EDGE ( 'NONE', *, *, #66162, .F. ) ;
#20595 = CARTESIAN_POINT ( 'NONE',  ( -109.5462627524148900, -278.3976335827215962, -243.6361517084054356 ) ) ;
#20596 = CARTESIAN_POINT ( 'NONE',  ( -14.00176467120770241, -275.3037913642411922, -200.9445791702334532 ) ) ;
#20597 = CARTESIAN_POINT ( 'NONE',  ( 17.34453868686904698, -276.5795275588117761, -217.5277734039811719 ) ) ;
#20598 = CARTESIAN_POINT ( 'NONE',  ( -112.5908924339967285, -276.5211947720129615, -274.3568478868846796 ) ) ;
#20599 = CARTESIAN_POINT ( 'NONE',  ( -90.12520409805796362, -297.9330644373174550, -219.7140250709381348 ) ) ;
#20600 = CARTESIAN_POINT ( 'NONE',  ( -106.5474714951690487, -294.7944984498337249, -295.5297720092256100 ) ) ;
#20601 = DIRECTION ( 'NONE',  ( -1.000000000000000000, 0.000000000000000000, 0.000000000000000000 ) ) ;
#20602 = CARTESIAN_POINT ( 'NONE',  ( -106.1233782964871750, -279.4896621579867997, -235.7662531688034733 ) ) ;
#20603 = CARTESIAN_POINT ( 'NONE',  ( -8.736720786006902273, -276.8338497945538279, -337.5368163789413529 ) ) ;
#20604 = CARTESIAN_POINT ( 'NONE',  ( -12.84565473796202362, -285.0488624312961292, -197.8818655564179210 ) ) ;
#20605 = CARTESIAN_POINT ( 'NONE',  ( -79.61551375678384090, -299.4829905163437616, -208.1458641003685273 ) ) ;
#20606 = CARTESIAN_POINT ( 'NONE',  ( 2.197429475817664013, -229.5268262511776527, 25.50000000000000000 ) ) ;
#20607 = CARTESIAN_POINT ( 'NONE',  ( -0.9199129578981691813, -287.7528504982832942, -333.8706304382895382 ) ) ;
#20608 = CARTESIAN_POINT ( 'NONE',  ( -16.61678434090731571, -278.5634683795046271, -199.3086593551412307 ) ) ;
#20610 = CARTESIAN_POINT ( 'NONE',  ( -40.31589792167037700, -281.1696790036205584, -344.7416822955788120 ) ) ;
#20609 = CARTESIAN_POINT ( 'NONE',  ( -110.2026008664295915, -277.2666439599022397, -259.6803181408615160 ) ) ;
#20611 = CARTESIAN_POINT ( 'NONE',  ( 37.47492556833609001, -289.4762135491798745, -264.4340648264293350 ) ) ;
#20612 = CARTESIAN_POINT ( 'NONE',  ( -4.876711406066927879, -277.8199528496396056, -336.2017895178984759 ) ) ;
#20613 = DIRECTION ( 'NONE',  ( 1.000000000000000000, -0.000000000000000000, 0.000000000000000000 ) ) ;
#20614 = CARTESIAN_POINT ( 'NONE',  ( -104.0962041061745538, -276.3160045221297310, -306.6627737323630640 ) ) ;
#20615 = CARTESIAN_POINT ( 'NONE',  ( -36.74355774891985504, -274.7112778488695994, -197.2491995169925474 ) ) ;
#20616 = CARTESIAN_POINT ( 'NONE',  ( 3.569741778591647208, -284.5038572337506366, -333.4804175768238110 ) ) ;
#20617 = DIRECTION ( 'NONE',  ( 0.000000000000000000, -1.000000000000000000, 0.000000000000000000 ) ) ;
#20618 = CARTESIAN_POINT ( 'NONE',  ( 13.65029814504605987, -290.2649952785097298, -326.1916170002156150 ) ) ;
#20619 = CARTESIAN_POINT ( 'NONE',  ( -23.47894108206374852, -290.2290642114985530, -196.6013032327773544 ) ) ;
#20620 = CARTESIAN_POINT ( 'NONE',  ( 82.15666016531748994, -298.9416642213269029, -197.2723373383452383 ) ) ;
#20621 = CARTESIAN_POINT ( 'NONE',  ( 22.69329040579045298, -273.6490041103211297, -227.9477779744090071 ) ) ;
#20622 = CARTESIAN_POINT ( 'NONE',  ( -1.828028687576657818, -290.6674034986428978, -205.1573821108576112 ) ) ;
#20623 = CARTESIAN_POINT ( 'NONE',  ( 68.56402772857219929, 46.98157435473511612, -321.4867780223927980 ) ) ;
#20624 = PLANE ( 'NONE',  #3571 ) ;
#20625 = CARTESIAN_POINT ( 'NONE',  ( -109.2190586751007402, -288.7039528740641003, -296.1372691806154762 ) ) ;
#20626 = CARTESIAN_POINT ( 'NONE',  ( -91.31276540261265495, -285.4362405398349551, -320.6956441906409623 ) ) ;
#20627 = CARTESIAN_POINT ( 'NONE',  ( 35.40865071816693899, -286.0715831718487152, -292.3461931515810761 ) ) ;
#20628 = CARTESIAN_POINT ( 'NONE',  ( -93.86307815798451770, -285.3140703446956650, -317.4855144701957101 ) ) ;
#20629 = CARTESIAN_POINT ( 'NONE',  ( -108.5801924970181744, -285.1349949749995289, -287.0795220944924608 ) ) ;
#20630 = CARTESIAN_POINT ( 'NONE',  ( -112.6072130482546214, -292.4850761205244680, -274.0366267838651879 ) ) ;
#20631 = CARTESIAN_POINT ( 'NONE',  ( 37.30912635175043590, -273.7851145521747185, -282.3750768043902895 ) ) ;
#20632 = CARTESIAN_POINT ( 'NONE',  ( 26.05188392677884224, -276.4631487834815289, -314.1225709385395248 ) ) ;
#20633 = CARTESIAN_POINT ( 'NONE',  ( -112.3864280376646860, -288.5142079795967334, -279.6034059470242141 ) ) ;
#20634 = CARTESIAN_POINT ( 'NONE',  ( -67.70860737833254461, -277.4397783517609355, -341.1202230083772520 ) ) ;
#20635 = CARTESIAN_POINT ( 'NONE',  ( -61.52267975163120894, -297.3475836450063525, -341.0354864051587924 ) ) ;
#20636 = CARTESIAN_POINT ( 'NONE',  ( -48.18343439338621437, -252.7258303143705120, -489.5392129326988311 ) ) ;
#20637 = DIRECTION ( 'NONE',  ( 0.000000000000000000, 0.000000000000000000, 1.000000000000000000 ) ) ;
#20638 = CARTESIAN_POINT ( 'NONE',  ( -85.19548484829935830, -282.4143702902513837, -326.1397766668883378 ) ) ;
#20639 = CARTESIAN_POINT ( 'NONE',  ( -50.56142015072196472, -277.8831487152559703, -196.5353795947974049 ) ) ;
#20640 = DIRECTION ( 'NONE',  ( 0.000000000000000000, 0.000000000000000000, 1.000000000000000000 ) ) ;
#20641 = CARTESIAN_POINT ( 'NONE',  ( 38.92947524948860405, -274.0783339532729883, -274.0301079433759810 ) ) ;
#20642 = CARTESIAN_POINT ( 'NONE',  ( -37.81873970715011524, -276.4068319517576811, -343.4739650071252299 ) ) ;
#20643 = CARTESIAN_POINT ( 'NONE',  ( -2.801818328652338597, -296.1069215368674463, -335.4587701603929304 ) ) ;
#20644 = CARTESIAN_POINT ( 'NONE',  ( 39.31041463148132920, -280.5031009006950171, -272.7995215156219615 ) ) ;
#20645 = CARTESIAN_POINT ( 'NONE',  ( -94.11737487915920042, -296.8404814350064953, -316.6402141705581812 ) ) ;
#20646 = CARTESIAN_POINT ( 'NONE',  ( 0.3124782378701334573, -295.8766939259398328, -336.9754596470872343 ) ) ;
#20647 = CARTESIAN_POINT ( 'NONE',  ( 94.41209358101258431, -299.5800556217366193, -197.3651080369727708 ) ) ;
#20648 = CARTESIAN_POINT ( 'NONE',  ( -69.90847475729853500, -293.6234967485889342, -202.7865481686931162 ) ) ;
#20649 = CARTESIAN_POINT ( 'NONE',  ( -114.1520200293542473, -284.7952553521871550, -264.2503526948493118 ) ) ;
#20650 = CARTESIAN_POINT ( 'NONE',  ( -13.42950850562544929, -272.4989993467435738, -198.4687500235213804 ) ) ;
#20651 = CARTESIAN_POINT ( 'NONE',  ( 16.30070993815878566, -286.6220970128609338, -215.1208080017152326 ) ) ;
#20652 = CARTESIAN_POINT ( 'NONE',  ( -96.93989397299300492, -281.1496530507380385, -225.3965717038308014 ) ) ;
#20653 = CARTESIAN_POINT ( 'NONE',  ( -67.63411484682815455, -284.7033705575130398, -203.6844499546599536 ) ) ;
#20654 = CARTESIAN_POINT ( 'NONE',  ( -36.14498329869359594, -287.0370230935881182, -345.3643443442269927 ) ) ;
#20655 = CARTESIAN_POINT ( 'NONE',  ( -65.60899210820664962, -198.9355752380678553, -358.8784014864789924 ) ) ;
#20656 = CARTESIAN_POINT ( 'NONE',  ( 6.969220374530967099, -286.1813703017011790, -212.2064806298952249 ) ) ;
#20657 = CARTESIAN_POINT ( 'NONE',  ( -53.32857801162950295, -290.9108321976858633, -195.2252330318355860 ) ) ;
#20658 = CARTESIAN_POINT ( 'NONE',  ( -113.5778603670490128, -280.1723693397156580, -268.7714838195372522 ) ) ;
#20659 = CARTESIAN_POINT ( 'NONE',  ( -112.3070299301571993, -279.6741693204269268, -285.7064214304120355 ) ) ;
#20660 = CARTESIAN_POINT ( 'NONE',  ( 24.12929439058094871, -281.9312803662752458, -309.8281039256343092 ) ) ;
#20661 = CARTESIAN_POINT ( 'NONE',  ( -29.81377501960339771, -276.1476309346280118, -195.7398677138005780 ) ) ;
#20662 = CARTESIAN_POINT ( 'NONE',  ( -68.22617953468768803, -295.4467134199439329, -340.8958536224056388 ) ) ;
#20663 = CARTESIAN_POINT ( 'NONE',  ( -5.104402729032415209, -286.6457822885271298, -337.6857305970476091 ) ) ;
#20664 = CARTESIAN_POINT ( 'NONE',  ( -107.1679009692855402, -295.1756813818711862, -292.8532874764903795 ) ) ;
#20665 = EDGE_LOOP ( 'NONE', ( #9105, #11929, #43855, #60477 ) ) ;
#20666 = CARTESIAN_POINT ( 'NONE',  ( -56.66968670148714438, -285.2234287546890528, -342.2481344050952998 ) ) ;
#20667 = CARTESIAN_POINT ( 'NONE',  ( -63.58055407155491423, -295.0703823581748679, -338.5587319541636475 ) ) ;
#20668 = CARTESIAN_POINT ( 'NONE',  ( -8.639715598758026971, -293.4987615638497118, -199.2436897807114349 ) ) ;
#20669 = CARTESIAN_POINT ( 'NONE',  ( -38.87891642067148723, -283.7233205021925073, -343.4593954369836979 ) ) ;
#20670 = ADVANCED_FACE ( 'NONE', ( #23941 ), #53283, .T. ) ;
#20671 = CARTESIAN_POINT ( 'NONE',  ( -32.68486343263671756, -273.1682157176454666, -193.7246816214905323 ) ) ;
#20672 = CARTESIAN_POINT ( 'NONE',  ( 3.133547090913871624, -289.1754214415847173, -335.8075846623377174 ) ) ;
#20673 = CARTESIAN_POINT ( 'NONE',  ( -35.94609271736964473, -281.1744479031477226, -346.1259737302938788 ) ) ;
#20674 = CARTESIAN_POINT ( 'NONE',  ( -112.2976526568304649, -291.1047519415854481, -252.8297326358438966 ) ) ;
#20675 = CARTESIAN_POINT ( 'NONE',  ( 23.52946783180308898, -288.4452092015594076, -310.7174236836295336 ) ) ;
#20676 = CARTESIAN_POINT ( 'NONE',  ( 222.2216768131362130, 37.54180348216212337, 10.00000000000000000 ) ) ;
#20677 = CARTESIAN_POINT ( 'NONE',  ( 128.9467878515196162, -299.5541904835127980, -198.8526868767648352 ) ) ;
#20678 = CARTESIAN_POINT ( 'NONE',  ( -38.83267329410574575, -140.1998172465924313, -360.9197421274957378 ) ) ;
#20679 = CARTESIAN_POINT ( 'NONE',  ( -4.771743288812454686, -289.9809262143061801, -202.8022627189028810 ) ) ;
#20680 = ORIENTED_EDGE ( 'NONE', *, *, #23679, .T. ) ;
#20681 = CARTESIAN_POINT ( 'NONE',  ( -102.4240027089262810, -277.9307569353740064, -236.5087154671401777 ) ) ;
#20682 = CARTESIAN_POINT ( 'NONE',  ( 35.71123962399595086, -274.9113823402823300, -245.9234868334324062 ) ) ;
#20683 = CARTESIAN_POINT ( 'NONE',  ( -111.4407549128927002, -280.6915240882544254, -259.5432454525962385 ) ) ;
#20684 = CARTESIAN_POINT ( 'NONE',  ( -45.97742063028599802, -156.0892642442967713, -362.7395337765181011 ) ) ;
#20685 = EDGE_CURVE ( 'NONE', #87609, #47159, #1482, .T. ) ;
#20686 = CARTESIAN_POINT ( 'NONE',  ( 8.209942395161199613, -279.2359934933105023, -208.9467070802182036 ) ) ;
#20687 = CARTESIAN_POINT ( 'NONE',  ( -90.07370503217666169, -281.8214467921291089, -323.2653367409481575 ) ) ;
#20688 = CARTESIAN_POINT ( 'NONE',  ( -92.93263769845842148, -297.5964752944574911, -322.1839592232947780 ) ) ;
#20689 = CARTESIAN_POINT ( 'NONE',  ( 33.83679862977677288, -294.2623806580214705, -286.8968421600630450 ) ) ;
#20690 = ORIENTED_EDGE ( 'NONE', *, *, #26705, .T. ) ;
#20691 = CARTESIAN_POINT ( 'NONE',  ( -109.7597976945589693, -289.4048864911461010, -257.5464503063615780 ) ) ;
#20692 = CARTESIAN_POINT ( 'NONE',  ( 2.358265231522841177, -275.2209044652397552, -204.5035023488277943 ) ) ;
#20693 = CARTESIAN_POINT ( 'NONE',  ( -102.0304462058307422, -273.0138301201752142, -236.4231523912723674 ) ) ;
#20694 = ORIENTED_EDGE ( 'NONE', *, *, #62216, .T. ) ;
#20695 = DIRECTION ( 'NONE',  ( 0.000000000000000000, 0.000000000000000000, -1.000000000000000000 ) ) ;
#20696 = CARTESIAN_POINT ( 'NONE',  ( 222.8344101925596306, 0.000000000000000000, 21.50000000000000000 ) ) ;
#20697 = CYLINDRICAL_SURFACE ( 'NONE', #54855, 2.500000000000002220 ) ;
#20698 = CARTESIAN_POINT ( 'NONE',  ( -39.72499874009503174, -281.1012280292210903, -197.0781832256423058 ) ) ;
#20699 = CARTESIAN_POINT ( 'NONE',  ( -66.98805117935783926, -281.4290139896001506, -200.3963562490588117 ) ) ;
#20700 = CARTESIAN_POINT ( 'NONE',  ( -82.95059137580459208, -282.7523340880581486, -327.7257419291232168 ) ) ;
#20701 = CARTESIAN_POINT ( 'NONE',  ( 34.64770173359642058, -283.1767846151940375, -252.1879640621988017 ) ) ;
#20702 = CARTESIAN_POINT ( 'NONE',  ( -4.776966075357743868, -275.0951963103696016, -336.4829738990276837 ) ) ;
#20703 = FACE_OUTER_BOUND ( 'NONE', #31970, .T. ) ;
#20704 = DIRECTION ( 'NONE',  ( -0.2456588035076310295, 0.9693563597868428694, 1.734723475976805517E-15 ) ) ;
#20705 = CARTESIAN_POINT ( 'NONE',  ( -35.70467828869394111, -277.8349667625615780, -347.1952981290345406 ) ) ;
#20706 = ORIENTED_EDGE ( 'NONE', *, *, #63388, .F. ) ;
#20707 = ORIENTED_EDGE ( 'NONE', *, *, #16197, .F. ) ;
#20708 = CARTESIAN_POINT ( 'NONE',  ( 140.6539576904058606, 275.5000000000000568, -10.49999999999999822 ) ) ;
#20709 = CARTESIAN_POINT ( 'NONE',  ( -41.45361806466899424, -285.0834465771308146, -345.6552603841092264 ) ) ;
#20710 = CARTESIAN_POINT ( 'NONE',  ( 23.48116052620613203, -292.1859238670654122, -229.7017851198063454 ) ) ;
#20711 = CARTESIAN_POINT ( 'NONE',  ( -28.99649650406889734, -288.2977377251822872, -346.8584760208775037 ) ) ;
#20712 = CARTESIAN_POINT ( 'NONE',  ( -10.35995967590083033, -284.6489722053108267, -201.4274510843903556 ) ) ;
#20714 = CARTESIAN_POINT ( 'NONE',  ( -5.374778843717738397, -286.8654976820677689, -337.1150688794369330 ) ) ;
#20713 = CARTESIAN_POINT ( 'NONE',  ( -109.5032299632216137, -283.3156465319873973, -255.9358439664611922 ) ) ;
#20715 = CARTESIAN_POINT ( 'NONE',  ( -16.00248016678046525, -283.9750205940136993, -340.5876670606424454 ) ) ;
#20716 = CARTESIAN_POINT ( 'NONE',  ( -30.00842227774316484, -272.1448144038657802, -195.7204877319498166 ) ) ;
#20717 = CARTESIAN_POINT ( 'NONE',  ( -113.5259403506055662, -282.9928859177989580, -267.1278141250662088 ) ) ;
#20718 = CARTESIAN_POINT ( 'NONE',  ( -92.20852106584543151, -297.8364558175825891, -321.5135038868004358 ) ) ;
#20719 = CARTESIAN_POINT ( 'NONE',  ( -63.87561090928890906, -283.7068214045204400, -200.0196279862317397 ) ) ;
#20720 = CARTESIAN_POINT ( 'NONE',  ( -110.3941962026603676, -279.5614070086731999, -265.1899222917380712 ) ) ;
#20721 = CARTESIAN_POINT ( 'NONE',  ( 23.21089669944873535, -288.9462715007371116, -225.8256102786311317 ) ) ;
#20722 = DIRECTION ( 'NONE',  ( 0.000000000000000000, 0.000000000000000000, 1.000000000000000000 ) ) ;
#20723 = CARTESIAN_POINT ( 'NONE',  ( 154.1407330040854333, 275.0000000000000568, -13.42592592592594158 ) ) ;
#20724 = CARTESIAN_POINT ( 'NONE',  ( 30.93942987269103284, -295.8962521824159353, -302.8405713993465156 ) ) ;
#20725 = CARTESIAN_POINT ( 'NONE',  ( -40.61794608402050244, -275.0931724838617924, -345.3023351529357114 ) ) ;
#20726 = CARTESIAN_POINT ( 'NONE',  ( -86.40205771588632899, -290.5883884781811730, -211.1545715365120657 ) ) ;
#20727 = CARTESIAN_POINT ( 'NONE',  ( 17.66337529269165074, -292.6484605857987162, -319.5826248361901776 ) ) ;
#20728 = CARTESIAN_POINT ( 'NONE',  ( -34.27610397999585956, -278.7762859959636330, -196.9193022093285208 ) ) ;
#20729 = CARTESIAN_POINT ( 'NONE',  ( -50.14403857545830334, -296.0266086211211700, -197.2381694088662698 ) ) ;
#20730 = CARTESIAN_POINT ( 'NONE',  ( -3.423451136932255778, -293.8250127401769873, -205.1629902137349575 ) ) ;
#20731 = CARTESIAN_POINT ( 'NONE',  ( 35.77081079830085031, -283.8376638359844719, -253.6410175316879361 ) ) ;
#20732 = CARTESIAN_POINT ( 'NONE',  ( -70.41090225979451134, -296.1039986695323023, -201.5924068826096516 ) ) ;
#20733 = CARTESIAN_POINT ( 'NONE',  ( -85.18837032191426317, -291.3255891978590171, -326.6169565860685111 ) ) ;
#20734 = CARTESIAN_POINT ( 'NONE',  ( -67.90040479831368714, -289.8963981491785376, -200.7758306376524047 ) ) ;
#20735 = CARTESIAN_POINT ( 'NONE',  ( -109.2904588517238267, -292.1796265437973830, -254.9095472839576928 ) ) ;
#20736 = DIRECTION ( 'NONE',  ( -0.000000000000000000, -0.000000000000000000, -1.000000000000000000 ) ) ;
#20737 = CARTESIAN_POINT ( 'NONE',  ( -66.63810330690455430, -292.4611100834927697, -203.3214096886038078 ) ) ;
#20738 = DIRECTION ( 'NONE',  ( -0.000000000000000000, -0.000000000000000000, -1.000000000000000000 ) ) ;
#20739 = CARTESIAN_POINT ( 'NONE',  ( -95.37021874277319000, -292.4361418703693403, -220.3340665504157414 ) ) ;
#20741 = CARTESIAN_POINT ( 'NONE',  ( -4.833079267209935637, -292.4925839043611973, -204.9852046106930175 ) ) ;
#20740 = CARTESIAN_POINT ( 'NONE',  ( 29.60410717336755937, -280.0279259554579880, -304.9539739589831129 ) ) ;
#20742 = CARTESIAN_POINT ( 'NONE',  ( 36.17570850998654919, -281.2645293550647239, -247.4659082839496591 ) ) ;
#20743 = CARTESIAN_POINT ( 'NONE',  ( 0.8541787609222049049, -282.2238465905517160, -337.2106116602250268 ) ) ;
#20744 = CARTESIAN_POINT ( 'NONE',  ( 10.32058661838865987, -284.7097257661956178, -212.4533718015969725 ) ) ;
#20745 = CARTESIAN_POINT ( 'NONE',  ( 18.51896090282600227, -280.3777764790950755, -319.2533671761889877 ) ) ;
#20746 = CARTESIAN_POINT ( 'NONE',  ( -36.56000823155557811, -284.0618060800927651, -195.3524865577254275 ) ) ;
#20747 = CARTESIAN_POINT ( 'NONE',  ( 228.6245981097501101, -142.7221692137691775, -32.50000000000000711 ) ) ;
#20748 = CARTESIAN_POINT ( 'NONE',  ( -19.89575639285349595, -278.7522021942000379, -196.0212611830721414 ) ) ;
#20749 = CARTESIAN_POINT ( 'NONE',  ( -57.66074642615794232, -284.7162334006808351, -196.3558130224410547 ) ) ;
#20750 = CARTESIAN_POINT ( 'NONE',  ( -24.57829108891397141, -275.0219112077140267, -198.2698641523999186 ) ) ;
#20751 = CARTESIAN_POINT ( 'NONE',  ( 197.1656530321902494, 41.90019538913896469, 12.64285714285713524 ) ) ;
#20752 = CARTESIAN_POINT ( 'NONE',  ( 36.00436258126122624, -295.2648036968413976, -278.9839979288634595 ) ) ;
#20753 = CARTESIAN_POINT ( 'NONE',  ( -31.32470331478227976, -275.5519792272103814, -194.1744386914177483 ) ) ;
#20754 = CARTESIAN_POINT ( 'NONE',  ( -110.3014391925587887, -278.1793846025415178, -273.3551056796637795 ) ) ;
#20755 = CARTESIAN_POINT ( 'NONE',  ( -84.26803050584193500, -291.5936904634081657, -209.2454148529283771 ) ) ;
#20756 = CARTESIAN_POINT ( 'NONE',  ( 21.76448100599156277, -278.9896011899159589, -223.2685349867159914 ) ) ;
#20757 = CARTESIAN_POINT ( 'NONE',  ( -72.17036813410757645, -291.4376627662732631, -201.6736429756137454 ) ) ;
#20758 = CARTESIAN_POINT ( 'NONE',  ( -57.70891937894879931, -290.8414966902099081, -199.9618948131748368 ) ) ;
#20759 = CARTESIAN_POINT ( 'NONE',  ( -4.137748087443496203, -292.6142979437767622, -337.6248627875890520 ) ) ;
#20760 = ORIENTED_EDGE ( 'NONE', *, *, #67389, .F. ) ;
#20761 = CARTESIAN_POINT ( 'NONE',  ( 151.0528680457221355, 20.99319481056636505, 6.529293081340417082 ) ) ;
#20762 = CARTESIAN_POINT ( 'NONE',  ( 28.79689196603782975, -292.6394019826446993, -239.1985781341939514 ) ) ;
#20763 = CARTESIAN_POINT ( 'NONE',  ( 209.3197381339219874, 28.92950916896207048, 12.09245862089610490 ) ) ;
#20764 = CARTESIAN_POINT ( 'NONE',  ( -109.1418805571601069, -276.0523547857346784, -270.3284710469131937 ) ) ;
#20765 = CARTESIAN_POINT ( 'NONE',  ( -106.2966940996912939, -296.0454374831130053, -236.6264322918149219 ) ) ;
#20766 = CARTESIAN_POINT ( 'NONE',  ( -94.95227913953195298, -285.1820416947531953, -320.7031427688282292 ) ) ;
#20767 = CARTESIAN_POINT ( 'NONE',  ( 0.1704845652020387514, -286.3996527890865877, -207.6776213788750169 ) ) ;
#20768 = CARTESIAN_POINT ( 'NONE',  ( 36.33569530298197492, -277.0522532264325264, -268.8284232869652328 ) ) ;
#20769 = CARTESIAN_POINT ( 'NONE',  ( -98.54615216451782089, -293.9896120425282788, -313.0912227646948054 ) ) ;
#20770 = CARTESIAN_POINT ( 'NONE',  ( -106.7640101030666528, -298.6515164449539839, -244.5515823946464593 ) ) ;
#20771 = CARTESIAN_POINT ( 'NONE',  ( -13.67178574940730762, -275.5330076962840735, -339.8901880931460937 ) ) ;
#20772 = ORIENTED_EDGE ( 'NONE', *, *, #92502, .F. ) ;
#20773 = FACE_OUTER_BOUND ( 'NONE', #32634, .T. ) ;
#20774 = CARTESIAN_POINT ( 'NONE',  ( -69.52294920914108900, -295.1309442718950322, -340.3048797477754874 ) ) ;
#20775 = CARTESIAN_POINT ( 'NONE',  ( 20.65040558188598396, -290.1193487647574329, -317.0326283204814786 ) ) ;
#20776 = CARTESIAN_POINT ( 'NONE',  ( 60.24221760881081167, -297.2734843241957492, -195.3943839220979442 ) ) ;
#20777 = CARTESIAN_POINT ( 'NONE',  ( -15.81372404671005683, -289.4177381614483693, -340.2741573733025575 ) ) ;
#20779 = ORIENTED_EDGE ( 'NONE', *, *, #85278, .T. ) ;
#20778 = EDGE_CURVE ( 'NONE', #42785, #15573, #74387, .T. ) ;
#20780 = CARTESIAN_POINT ( 'NONE',  ( -88.76491776713821480, -278.4094828741769447, -213.3657418541260142 ) ) ;
#20781 = CARTESIAN_POINT ( 'NONE',  ( -100.6714333068340466, -297.7804423898321602, -226.7185096576982062 ) ) ;
#20782 = CARTESIAN_POINT ( 'NONE',  ( -108.7101548051434889, -288.3637137330772475, -295.9500226618915235 ) ) ;
#20783 = CARTESIAN_POINT ( 'NONE',  ( -68.21380337838547803, -295.7799407258559086, -340.8781906139090552 ) ) ;
#20784 = CARTESIAN_POINT ( 'NONE',  ( 14.33424181413710130, -294.6345595904641641, -322.0237333995472682 ) ) ;
#20785 = CARTESIAN_POINT ( 'NONE',  ( 223.4306832106270804, -135.2391364535880882, 22.50000000000000000 ) ) ;
#20786 = CARTESIAN_POINT ( 'NONE',  ( 221.4259212729440094, 36.93618551656547311, 7.000000000000000000 ) ) ;
#20787 = CARTESIAN_POINT ( 'NONE',  ( 140.6539576904058606, 130.0000000000000568, 12.50000000000000000 ) ) ;
#20788 = CARTESIAN_POINT ( 'NONE',  ( -37.48071883607661903, -290.5739415982342848, -346.6806149350667283 ) ) ;
#20789 = CARTESIAN_POINT ( 'NONE',  ( 25.22466315766300227, -284.6948066931273047, -320.2154176792147382 ) ) ;
#20790 = VERTEX_POINT ( 'NONE', #52813 ) ;
#20791 = CARTESIAN_POINT ( 'NONE',  ( 37.09105149305234761, -281.1428124644008335, -289.6763522041675287 ) ) ;
#20792 = CARTESIAN_POINT ( 'NONE',  ( -59.46645619217912326, -285.3393142992701428, -341.9035144645726518 ) ) ;
#20793 = CARTESIAN_POINT ( 'NONE',  ( 37.97914149102219739, -285.9638418723594100, -257.4241356919386021 ) ) ;
#20794 = CARTESIAN_POINT ( 'NONE',  ( -108.7702767015497045, -288.9044534800641486, -249.3570768277865000 ) ) ;
#20795 = CARTESIAN_POINT ( 'NONE',  ( 37.69748899773254891, -277.2796082793372534, -259.9004499528941778 ) ) ;
#20796 = ORIENTED_EDGE ( 'NONE', *, *, #29441, .F. ) ;
#20798 = CARTESIAN_POINT ( 'NONE',  ( 34.66893093770704581, -280.7349615901142670, -257.7769341837247907 ) ) ;
#20797 = CARTESIAN_POINT ( 'NONE',  ( -94.45303514320988825, -277.9098345345587404, -315.8486053523699297 ) ) ;
#20799 = CARTESIAN_POINT ( 'NONE',  ( 9.311370640959509615, -275.7561441169557952, -209.4925423733004664 ) ) ;
#20800 = CARTESIAN_POINT ( 'NONE',  ( -72.31178479362132805, -278.3948331338272055, -202.1915589963417972 ) ) ;
#20801 = CARTESIAN_POINT ( 'NONE',  ( 171.9668532218946950, 242.4161052218647683, -177.9424729848912534 ) ) ;
#20802 = CARTESIAN_POINT ( 'NONE',  ( -15.85474592014891471, -275.2646036841996420, -196.6097434540513689 ) ) ;
#20803 = EDGE_CURVE ( 'NONE', #11722, #85835, #45229, .T. ) ;
#20804 = CARTESIAN_POINT ( 'NONE',  ( -77.90515536138023833, -298.9437089510076362, -205.6060997081535504 ) ) ;
#20805 = CARTESIAN_POINT ( 'NONE',  ( -20.25526795762937127, -288.7662352645560304, -195.3538533559490702 ) ) ;
#20806 = DIRECTION ( 'NONE',  ( 0.6056179655966478226, -0.7957555401921982963, 0.000000000000000000 ) ) ;
#20807 = CARTESIAN_POINT ( 'NONE',  ( 35.86041165532898134, -288.5686672958799477, -265.5527860586612974 ) ) ;
#20808 = CARTESIAN_POINT ( 'NONE',  ( -5.222919879042626334, -288.2292120952364485, -201.4963376337424563 ) ) ;
#20809 = EDGE_CURVE ( 'NONE', #61882, #75307, #3098, .T. ) ;
#20810 = CARTESIAN_POINT ( 'NONE',  ( -10.69466430851150207, -288.0439238285759984, -338.4876342318938782 ) ) ;
#20811 = CARTESIAN_POINT ( 'NONE',  ( -113.7577895998465465, -284.1718320527639889, -261.4108010605994536 ) ) ;
#20812 = CARTESIAN_POINT ( 'NONE',  ( 9.803081668116483627, -279.1133610424893732, -213.5158808613807935 ) ) ;
#20813 = CARTESIAN_POINT ( 'NONE',  ( 3.100423554835791684, -288.4621026972658910, -208.1092094905771432 ) ) ;
#20814 = CARTESIAN_POINT ( 'NONE',  ( 35.25339923136706943, -279.8663931735749770, -257.6859729172309130 ) ) ;
#20815 = CARTESIAN_POINT ( 'NONE',  ( -93.97541681768129251, -279.2075490431035973, -317.2195489370879500 ) ) ;
#20816 = CARTESIAN_POINT ( 'NONE',  ( 2.958663204777464362, -275.1013428891782837, -209.3591351345004341 ) ) ;
#20817 = CARTESIAN_POINT ( 'NONE',  ( -9.720893520471410199, -287.4941441396226196, -341.8110988145703004 ) ) ;
#20818 = CARTESIAN_POINT ( 'NONE',  ( 22.40417680613827045, -283.0044226538180965, -318.6994661230260135 ) ) ;
#20819 = CARTESIAN_POINT ( 'NONE',  ( -113.0752690445126376, -284.8710785474981435, -284.2164490515212947 ) ) ;
#20820 = CARTESIAN_POINT ( 'NONE',  ( 35.70285155340491201, -281.7313722969014407, -271.3116399768088058 ) ) ;
#20821 = ORIENTED_EDGE ( 'NONE', *, *, #70919, .T. ) ;
#20822 = ORIENTED_EDGE ( 'NONE', *, *, #81991, .F. ) ;
#20823 = CARTESIAN_POINT ( 'NONE',  ( 209.0105194359445875, 28.85114552632395046, 12.07126757350762603 ) ) ;
#20824 = CARTESIAN_POINT ( 'NONE',  ( -90.71135064313021701, -291.6590203382359618, -324.2120837381959859 ) ) ;
#20825 = CARTESIAN_POINT ( 'NONE',  ( -47.66019399952322289, -290.6085495531888228, -194.4998400290960774 ) ) ;
#20826 = CARTESIAN_POINT ( 'NONE',  ( -93.95264491281066910, -272.2671482226831472, -223.8806758915478952 ) ) ;
#20827 = CARTESIAN_POINT ( 'NONE',  ( 15.40273597902006131, -293.6783901606851259, -326.3194707647933797 ) ) ;
#20828 = CARTESIAN_POINT ( 'NONE',  ( -76.25108930946325358, -288.0625010808399225, -332.9451989097763658 ) ) ;
#20829 = CARTESIAN_POINT ( 'NONE',  ( 27.12809868588586681, -291.2999926311069885, -233.9023377423723957 ) ) ;
#20830 = CARTESIAN_POINT ( 'NONE',  ( 26.70641927683401207, -288.2682997489649210, -234.4107056613696614 ) ) ;
#20831 = CARTESIAN_POINT ( 'NONE',  ( -85.28047601435908120, -292.1948066931273615, -330.5268031993605859 ) ) ;
#20832 = CARTESIAN_POINT ( 'NONE',  ( -105.4550436317330764, -292.9660349834684325, -238.8434519815604062 ) ) ;
#20833 = CARTESIAN_POINT ( 'NONE',  ( -109.8572355757293906, -288.8064335118996269, -250.5253350984313272 ) ) ;
#20834 = CARTESIAN_POINT ( 'NONE',  ( -94.45811135570875194, -293.2253713033337590, -221.7338168028446148 ) ) ;
#20835 = CARTESIAN_POINT ( 'NONE',  ( -81.63036289327303052, -286.3734245513336987, -212.0351135088597232 ) ) ;
#20836 = CARTESIAN_POINT ( 'NONE',  ( 31.63177611316188376, -295.1622739673917408, -240.4832332030868542 ) ) ;
#20837 = CARTESIAN_POINT ( 'NONE',  ( -114.0814599542016055, -271.5444506490974277, -270.3482875283361295 ) ) ;
#20838 = CARTESIAN_POINT ( 'NONE',  ( -82.61252422152907116, -275.4173829585836870, -210.0549499711476074 ) ) ;
#20839 = CARTESIAN_POINT ( 'NONE',  ( -7.727338375026176820, -280.6638689043281261, -339.2667797889253620 ) ) ;
#20840 = CARTESIAN_POINT ( 'NONE',  ( -81.78664796669242776, -294.8373789485053180, -333.1062935041177298 ) ) ;
#20841 = CARTESIAN_POINT ( 'NONE',  ( -54.42395768749048557, -272.0695322114916621, -198.3460467296720253 ) ) ;
#20842 = CARTESIAN_POINT ( 'NONE',  ( -94.73153460467943887, -275.9727444448810161, -317.7912353738931870 ) ) ;
#20843 = CARTESIAN_POINT ( 'NONE',  ( -94.00444279580118234, -298.5265294166450190, -223.5379345244646458 ) ) ;
#20844 = CARTESIAN_POINT ( 'NONE',  ( 36.02526616560538031, -273.8549504354530200, -248.8243745535157530 ) ) ;
#20845 = CARTESIAN_POINT ( 'NONE',  ( -109.0553079769267839, -298.1934588575022076, -253.8525332928154796 ) ) ;
#20846 = DIRECTION ( 'NONE',  ( 0.000000000000000000, 0.000000000000000000, 1.000000000000000000 ) ) ;
#20847 = CARTESIAN_POINT ( 'NONE',  ( -105.1076338115589124, -296.9864173394244062, -297.9361058983351427 ) ) ;
#20848 = CARTESIAN_POINT ( 'NONE',  ( 196.6877655503061533, 293.9636489450775230, -7.999911143031724237 ) ) ;
#20850 = CARTESIAN_POINT ( 'NONE',  ( -63.07946570484787685, -297.7075374107682819, -201.9953597351392318 ) ) ;
#20849 = CARTESIAN_POINT ( 'NONE',  ( 6.605588592710036622, -284.6659594329059360, -209.0837433538838184 ) ) ;
#20851 = CARTESIAN_POINT ( 'NONE',  ( -0.9695574409687663930, -286.5214441691337015, -202.4931046305520681 ) ) ;
#20852 = CARTESIAN_POINT ( 'NONE',  ( 28.88339296018956404, -287.7302878641962707, -309.6037139327642649 ) ) ;
#20853 = CARTESIAN_POINT ( 'NONE',  ( -112.6934909867121490, -298.5412128329006123, -269.6438912791250004 ) ) ;
#20854 = CARTESIAN_POINT ( 'NONE',  ( -25.95290673324288377, -292.9066093389956791, -344.3227553983004441 ) ) ;
#20855 = CARTESIAN_POINT ( 'NONE',  ( -92.94981500799279672, -278.4765414177834373, -217.2577905456915062 ) ) ;
#20856 = CARTESIAN_POINT ( 'NONE',  ( -95.95921662488163406, -282.6952119285918457, -223.5744983911110353 ) ) ;
#20857 = CARTESIAN_POINT ( 'NONE',  ( 0.000000000000000000, 0.000000000000000000, 74.50000000000001421 ) ) ;
#20858 = CARTESIAN_POINT ( 'NONE',  ( 23.83200740056147637, -286.9071004384716161, -310.9415329595228741 ) ) ;
#20859 = DIRECTION ( 'NONE',  ( 0.000000000000000000, 0.000000000000000000, 1.000000000000000000 ) ) ;
#20860 = CARTESIAN_POINT ( 'NONE',  ( 2.348985582641040626, -286.5201396420990818, -333.9979792785127302 ) ) ;
#20861 = CARTESIAN_POINT ( 'NONE',  ( -35.81499124644425791, -299.6717045007252977, -196.5606880296625150 ) ) ;
#20862 = CARTESIAN_POINT ( 'NONE',  ( -74.73554353817104356, -280.9897158211193187, -203.7254911128403307 ) ) ;
#20864 = CARTESIAN_POINT ( 'NONE',  ( 29.31445927877850366, -281.9544478712251134, -300.2502529616966171 ) ) ;
#20863 = CARTESIAN_POINT ( 'NONE',  ( -110.9875180258348450, -294.7769342965548276, -254.3416535049790070 ) ) ;
#20865 = CARTESIAN_POINT ( 'NONE',  ( -113.2035059311331935, -296.5500998639170120, -283.8527604264756974 ) ) ;
#20866 = CARTESIAN_POINT ( 'NONE',  ( -41.93067324659531181, -299.5133995266389775, -196.8108013356921902 ) ) ;
#20867 = EDGE_CURVE ( 'NONE', #63636, #10890, #45652, .T. ) ;
#20868 = CARTESIAN_POINT ( 'NONE',  ( 36.69767369867167162, -283.7069798679340806, -282.4069486354017613 ) ) ;
#20869 = CARTESIAN_POINT ( 'NONE',  ( -86.24854588009516476, -296.4121609665739356, -215.8493863450990773 ) ) ;
#20870 = ORIENTED_EDGE ( 'NONE', *, *, #54992, .F. ) ;
#20871 = CARTESIAN_POINT ( 'NONE',  ( 180.5131398354828320, 250.0000000000000568, -23.92352941176473635 ) ) ;
#20872 = CARTESIAN_POINT ( 'NONE',  ( 15.09774189537612266, -284.2881463440410812, -323.5559644895413385 ) ) ;
#20873 = CARTESIAN_POINT ( 'NONE',  ( 175.2296996224750103, 161.0000000000000853, 0.000000000000000000 ) ) ;
#20874 = CARTESIAN_POINT ( 'NONE',  ( 39.58706461736021254, -285.0523547857346784, -270.3937649182068981 ) ) ;
#20875 = CARTESIAN_POINT ( 'NONE',  ( 24.23211951927487817, -275.3620944536096999, -316.3265784392799560 ) ) ;
#20876 = CARTESIAN_POINT ( 'NONE',  ( 34.48355572900142363, -293.2124890900710739, -257.2481084673755731 ) ) ;
#20877 = CARTESIAN_POINT ( 'NONE',  ( 32.01363576934313926, -283.4026846541706846, -295.4228514966454213 ) ) ;
#20878 = CARTESIAN_POINT ( 'NONE',  ( 25.95156454694661008, -276.6347061329499297, -232.3095360414971253 ) ) ;
#20879 = CARTESIAN_POINT ( 'NONE',  ( -96.70307339674830871, -285.3269018771783294, -318.4943923195729099 ) ) ;
#20880 = CARTESIAN_POINT ( 'NONE',  ( 10.15402573352566051, -281.1753108169779125, -326.3858425914673944 ) ) ;
#20881 = CARTESIAN_POINT ( 'NONE',  ( -94.63404593460406034, -281.2219457813750978, -221.9410674431646271 ) ) ;
#20882 = CARTESIAN_POINT ( 'NONE',  ( -104.2305826856863433, -273.2154371772530226, -232.1112541988979103 ) ) ;
#20883 = CARTESIAN_POINT ( 'NONE',  ( 30.54206305521553944, -275.8564585850491540, -306.8164333988646604 ) ) ;
#20884 = CARTESIAN_POINT ( 'NONE',  ( 37.08266507870625617, -295.5132587783598979, -273.5262827114689230 ) ) ;
#20885 = DIRECTION ( 'NONE',  ( -0.000000000000000000, -0.000000000000000000, 1.000000000000000000 ) ) ;
#20886 = PLANE ( 'NONE',  #19396 ) ;
#20887 = ADVANCED_FACE ( 'NONE', ( #59954 ), #68437, .F. ) ;
#20888 = CARTESIAN_POINT ( 'NONE',  ( -111.1087109149389960, -294.4713458284537069, -287.7012183247330768 ) ) ;
#20889 = TOROIDAL_SURFACE ( 'NONE', #45050, 5.603083949679977138, 1.500000000000000000 ) ;
#20890 = CARTESIAN_POINT ( 'NONE',  ( -36.72926060950825899, -273.5677027891699140, -197.2897205765402475 ) ) ;
#20891 = CARTESIAN_POINT ( 'NONE',  ( 38.54967042548561551, -295.1787554741550821, -278.7987952378402383 ) ) ;
#20892 = CARTESIAN_POINT ( 'NONE',  ( 29.23719464318176620, -295.2529543887138743, -308.3531286958000805 ) ) ;
#20893 = CARTESIAN_POINT ( 'NONE',  ( 35.49114571992429035, -289.7734966724760284, -287.5484678839014236 ) ) ;
#20894 = CARTESIAN_POINT ( 'NONE',  ( -72.53843986620150019, -275.5189877936258540, -336.4150918836038500 ) ) ;
#20895 = CARTESIAN_POINT ( 'NONE',  ( 14.75626865719569913, -278.2319686839630890, -323.6035608671764976 ) ) ;
#20896 = CARTESIAN_POINT ( 'NONE',  ( -110.4554868740314646, -294.8138405551773076, -256.3044777016045259 ) ) ;
#20897 = CARTESIAN_POINT ( 'NONE',  ( 37.95243297095561275, -283.2995713388204990, -261.4709942221876418 ) ) ;
#20898 = CARTESIAN_POINT ( 'NONE',  ( -35.91371754338383226, -284.9908065015312673, -197.0659139083344371 ) ) ;
#20899 = CARTESIAN_POINT ( 'NONE',  ( 105.0235304841314559, 114.7859377953624858, -281.8760858939756417 ) ) ;
#20900 = ORIENTED_EDGE ( 'NONE', *, *, #79581, .T. ) ;
#20901 = CARTESIAN_POINT ( 'NONE',  ( -85.73698815178835275, -285.0271910793953793, -215.6127974910766056 ) ) ;
#20902 = CARTESIAN_POINT ( 'NONE',  ( 35.32065431153155544, -282.9438863643317745, -295.0553005351545153 ) ) ;
#20903 =( BOUNDED_CURVE ( )  B_SPLINE_CURVE ( 3, ( #22789, #50273, #21885, #42700 ),
 .UNSPECIFIED., .F., .F. ) 
 B_SPLINE_CURVE_WITH_KNOTS ( ( 4, 4 ),
 ( 1.570796326794896780, 3.141592653589793116 ),
 .UNSPECIFIED. ) 
 CURVE ( )  GEOMETRIC_REPRESENTATION_ITEM ( )  RATIONAL_B_SPLINE_CURVE ( ( 1.000000000000000000, 0.8047378541243650485, 0.8047378541243650485, 1.000000000000000000 ) ) 
 REPRESENTATION_ITEM ( '' )  );
#20904 = CARTESIAN_POINT ( 'NONE',  ( -110.7319923787162708, -283.0696657928144191, -292.3583210136864636 ) ) ;
#20905 = CARTESIAN_POINT ( 'NONE',  ( -86.66274888914290386, -280.3274454312755779, -211.4678977715739450 ) ) ;
#20906 = ADVANCED_FACE ( 'NONE', ( #81693 ), #89721, .F. ) ;
#20907 =( LENGTH_UNIT ( ) NAMED_UNIT ( * ) SI_UNIT ( .MILLI., .METRE. ) );
#20908 = CARTESIAN_POINT ( 'NONE',  ( -84.42324187753636977, -279.2066402739680484, -330.4785258047362504 ) ) ;
#20909 = CARTESIAN_POINT ( 'NONE',  ( -21.33282851196159058, -297.3376638359844719, -340.3538533559490702 ) ) ;
#20910 = CARTESIAN_POINT ( 'NONE',  ( 204.5909265758117783, 295.1816420246624944, -54.00000000003019096 ) ) ;
#20911 = VERTEX_POINT ( 'NONE', #9252 ) ;
#20912 = CARTESIAN_POINT ( 'NONE',  ( -110.3285070359494853, -274.7649140686125406, -253.8397848411426594 ) ) ;
#20913 = CARTESIAN_POINT ( 'NONE',  ( -3.581603521288127645, -278.5200243446983563, -203.7728729229347664 ) ) ;
#20914 = CARTESIAN_POINT ( 'NONE',  ( -111.9345783728541761, -292.4967461168567979, -255.8061178496796515 ) ) ;
#20915 = CARTESIAN_POINT ( 'NONE',  ( 1.617149468239181820, -293.8651663714132951, -332.2765475686803711 ) ) ;
#20916 = CARTESIAN_POINT ( 'NONE',  ( -103.7484836467933746, -289.5525222358883752, -309.3209310175312794 ) ) ;
#20917 = DIRECTION ( 'NONE',  ( 0.000000000000000000, 1.000000000000000000, 0.000000000000000000 ) ) ;
#20919 = CARTESIAN_POINT ( 'NONE',  ( -72.74002389682556213, -283.9749907883933702, -205.5902876120702842 ) ) ;
#20918 = CARTESIAN_POINT ( 'NONE',  ( 24.39937915826459758, -292.7292676166636625, -315.4014300198842875 ) ) ;
#20920 = CARTESIAN_POINT ( 'NONE',  ( -32.09321001925210481, -293.9794481883918138, -196.2988490738038365 ) ) ;
#20921 = CARTESIAN_POINT ( 'NONE',  ( -74.02853751089649847, -284.8652946725479183, -334.1004946108089939 ) ) ;
#20922 = VERTEX_POINT ( 'NONE', #16841 ) ;
#20923 = CARTESIAN_POINT ( 'NONE',  ( -34.97969836027586865, -293.0223524817867542, -193.6196484299239273 ) ) ;
#20924 = CARTESIAN_POINT ( 'NONE',  ( 4.953682423873231322, -281.1336348153731137, -210.7868865038511785 ) ) ;
#20925 = CARTESIAN_POINT ( 'NONE',  ( -24.98705582815863124, -293.6930045112302423, -346.0149791639322530 ) ) ;
#20926 = CARTESIAN_POINT ( 'NONE',  ( 19.51166936137877883, -289.0591087946734206, -322.0706911991779293 ) ) ;
#20927 = CARTESIAN_POINT ( 'NONE',  ( -60.00316417309279871, -289.8305322261256833, -343.8865214185864829 ) ) ;
#20928 = CARTESIAN_POINT ( 'NONE',  ( 23.53289057147818752, -287.1587408663851875, -229.9796017682292302 ) ) ;
#20929 = VERTEX_POINT ( 'NONE', #38130 ) ;
#20930 = CARTESIAN_POINT ( 'NONE',  ( 196.7536206669780086, 25.83949066589314469, 12.63456096898028669 ) ) ;
#20931 = CARTESIAN_POINT ( 'NONE',  ( 32.29085992876478173, -295.8005927074665351, -300.3535846594114105 ) ) ;
#20932 = CARTESIAN_POINT ( 'NONE',  ( -36.17678014040627232, -296.7512821218360841, -193.8545191211221947 ) ) ;
#20933 = ADVANCED_FACE ( 'NONE', ( #67971 ), #23394, .T. ) ;
#20934 = CARTESIAN_POINT ( 'NONE',  ( -83.16328309463075641, -276.7559123518670390, -327.5559923027261107 ) ) ;
#20935 = CARTESIAN_POINT ( 'NONE',  ( -63.53025098054684605, -273.2274431866519535, -198.0168942503060805 ) ) ;
#20936 = CARTESIAN_POINT ( 'NONE',  ( -8.981782967233312931, -293.1542597173978493, -338.3926640260614818 ) ) ;
#20937 = CARTESIAN_POINT ( 'NONE',  ( 20.63548272896129276, -276.6715377598141004, -224.3341054917140411 ) ) ;
#20938 = CARTESIAN_POINT ( 'NONE',  ( -55.52117181844066351, -296.0549884609121136, -198.5621394372791144 ) ) ;
#20939 = CARTESIAN_POINT ( 'NONE',  ( 33.13573248648712877, -295.0274081169410465, -290.9017386271651162 ) ) ;
#20940 = CARTESIAN_POINT ( 'NONE',  ( -68.63685933805450645, -296.5530192012665793, -336.6684889897231869 ) ) ;
#20941 = CARTESIAN_POINT ( 'NONE',  ( -43.43097417488520762, -259.9284170800161178, -439.2763949627545799 ) ) ;
#20942 = CARTESIAN_POINT ( 'NONE',  ( -101.5627680980408769, -294.0295443666564665, -309.4211084301740584 ) ) ;
#20943 = CARTESIAN_POINT ( 'NONE',  ( -107.9332090816532599, -273.7438928579061326, -239.8785732479233559 ) ) ;
#20944 = CARTESIAN_POINT ( 'NONE',  ( 10.48454465268249791, -286.9515741042035870, -326.3572326024889776 ) ) ;
#20945 = CARTESIAN_POINT ( 'NONE',  ( -112.1864798006810275, -274.6238543444303559, -264.7895706816638040 ) ) ;
#20946 = CARTESIAN_POINT ( 'NONE',  ( -60.85827982244397560, -274.2474350844931337, -197.0491494324768098 ) ) ;
#20947 = CARTESIAN_POINT ( 'NONE',  ( -107.4808590807963071, -297.1540169585817353, -250.0489081515501084 ) ) ;
#20948 = CARTESIAN_POINT ( 'NONE',  ( -35.40414227653018742, -282.0562151002807241, -195.0179709589839092 ) ) ;
#20949 = CARTESIAN_POINT ( 'NONE',  ( 27.44274510741312056, -279.6995619370768509, -229.5644554990647066 ) ) ;
#20950 = ORIENTED_EDGE ( 'NONE', *, *, #74672, .T. ) ;
#20951 = CARTESIAN_POINT ( 'NONE',  ( 13.60703821590156082, -281.7093275045192513, -328.0300693289917149 ) ) ;
#20952 = CARTESIAN_POINT ( 'NONE',  ( 24.40298689390812470, -274.2905066446334672, -224.5254723403164974 ) ) ;
#20953 = CARTESIAN_POINT ( 'NONE',  ( -3.989172553448509184, -278.8845380209128280, -201.8336158705793935 ) ) ;
#20954 = CARTESIAN_POINT ( 'NONE',  ( -5.692183963668587587, -278.4672254734427952, -202.1824075429152856 ) ) ;
#20955 = CARTESIAN_POINT ( 'NONE',  ( -81.40946127837015922, -272.0145324676538507, -211.3615682054955585 ) ) ;
#20956 = CARTESIAN_POINT ( 'NONE',  ( 26.85111234636556432, -278.0730929238549720, -309.2452779252170671 ) ) ;
#20957 = AXIS2_PLACEMENT_3D ( 'NONE', #28197, #21538, #66051 ) ;
#20958 = CARTESIAN_POINT ( 'NONE',  ( 154.5853110399403931, 19.45846805016676484, 12.72325134073231112 ) ) ;
#20959 = CARTESIAN_POINT ( 'NONE',  ( -30.81407025375910536, -290.1542461436179678, -195.2375421658138066 ) ) ;
#20960 = CARTESIAN_POINT ( 'NONE',  ( -67.01544435105675745, -291.6737943119039755, -199.3085395368101445 ) ) ;
#20961 = B_SPLINE_CURVE_WITH_KNOTS ( 'NONE', 3,
 ( #44565, #66817, #66367, #53062, #9502, #65924, #15704, #29914, #74376, #89496, #46419, #81021, #73468, #16623, #8580, #45960, #38390, #24659, #74865, #73918, #81474, #1036, #1950, #81937, #37913, #59740, #2882, #23263, #67302, #9035, #30847, #1485, #9977, #2430, #58798, #17092, #45477, #88582, #60196, #53547, #30368, #89034, #24184, #67756, #31767, #60659, #23730, #82420, #37458, #59257, #17568, #87643, #52593, #8126, #45017, #22791, #51660, #80547, #88105, #52141, #75781, #61591, #68220, #90423, #33159, #10901, #54933, #12319, #41163, #55421, #68693, #26533, #84274, #11386, #19425, #70100, #19889, #62050, #90884, #75320, #39768, #47341, #18966, #26047, #69617, #55888, #5241, #40238, #83813, #34112, #33625, #3340, #47819, #63014, #39303, #83333, #91845, #61139, #3824, #10437, #27000, #76721, #32705, #69153, #48287, #11847, #40697, #32231, #62534, #84742, #18025, #4281, #25580, #77190, #4745, #89975, #82872, #25129, #91375, #54003, #46879, #54463, #18479, #76258, #86146, #27956, #57304, #70574, #12817, #5699, #87080, #34574, #41657, #48760, #35972, #64433, #78599, #64892, #57760, #63483, #56821, #13279, #50652, #21297, #77665, #28873, #50169, #13742, #71983, #456, #42116, #42591, #56846, #6166, #71506, #63949, #71032, #79066, #86606, #58236, #43535, #92314, #49703, #27468, #85687, #93259, #20834, #6639, #21776, #14218, #49246, #43078, #85224, #65349, #35519, #7101, #28413, #79540, #35035, #56361, #7549, #14679, #72432, #36434, #29343, #20375, #78141, #92788, #39071, #22229, #81705, #24898, #31537, #46647, #75549, #65817, #51099, #10673, #23952, #2658, #88805, #24415, #67984, #16854, #90204, #32474, #60425, #54233, #3110, #72883, #79986, #31993, #17337, #83102, #60885, #18255, #89736, #8008, #15123, #53778, #46188, #43986, #82645, #25353, #82181, #61820, #36900, #53295, #45709, #47108, #76015, #2195, #31079, #89265, #17794, #74622, #75093, #61371, #39528, #68449, #59967, #52827, #67528, #3584, #9751, #38625, #11148, #40010, #68927, #10202, #4058, #32928, #13510, #48523, #62288, #20611, #49481, #34343, #69853, #5473, #18729, #62782, #70347, #49013, #25813, #55655, #41889, #26770, #77424, #85464, #12085, #27236, #91615, #84508, #55189, #92545, #63250, #54693, #70800, #92081, #19654, #83567, #47590, #11617, #56124, #77911, #84977, #20128, #13053, #12563, #42359, #91124, #26295, #5935, #76494, #41414, #90652, #4987, #34807, #63720, #27713, #71272, #56612, #78371, #76957, #40462, #40933, #6399, #84047, #35271, #69380, #4512, #33389, #19193, #48052, #33873, #224, #44219, #58919, #8704, #22010, #64200, #28644, #65586, #72207, #87308, #22455, #13976, #93031, #51328, #64663, #43311, #35750, #30038, #93491, #36666, #7780, #58464, #14454, #49934, #57534, #28187, #36202, #701, #21529, #29104, #73127, #14904, #29585, #21066, #80221, #1155, #6877, #57998, #86378, #15359, #8254, #57076, #71751, #85915, #37135, #80679, #50880, #50409, #87767, #22919, #66043, #7324, #72659, #78830, #42834, #79315, #65121, #86854, #79762, #43759, #51789, #15835, #44692, #73593, #46544, #38524, #9637, #2086, #39430, #10104, #66493, #17694, #74993, #67428, #60785, #82999, #30976, #2556, #16749, #88705, #31435, #52719, #59864, #67883, #24791, #66947, #46086, #23400, #60325, #37582, #45604, #53190, #89162, #24312, #75447, #38972, #38039, #3007, #74042, #54128, #74506, #89623, #82068, #10565, #23853, #68347, #81601, #82543, #3474, #17224, #32365, #61266, #75908, #31892, #53676, #1610, #90101, #25252, #18151, #47004, #30495, #81146, #59389, #88241, #52266, #16290, #45143, #9160, #55549, #69277, #77794, #20015, #83941, #41782, #84398, #61714, #68822, #19547, #4875, #70693, #26660, #63141, #32824, #48413, #5823, #11976, #4406, #12944, #90548, #34235, #70234, #3952, #77316, #34697, #69743, #49371, #11033, #40824, #33285, #63610, #92434, #25706, #54589, #76849, #12450, #91970, #62180, #27598, #40360, #33759, #83460, #76389, #55072, #5368, #18616, #11513, #56495, #27125, #85354, #91013, #26181, #19094, #20502, #62670, #47947, #41298, #47480, #48893, #56008, #39901, #91504, #84864, #57881, #36552, #13402, #43201, #29469, #14342, #36092, #73009, #93382, #14797, #79199, #50293, #42717, #20956, #29925, #6766, #92918, #79656, #65469, #42246, #71159, #28080, #50771, #586, #43652, #86736, #72548, #72102, #1046, #78722, #13863, #21898, #64079, #71634, #78264, #7219, #37021, #58809, #35641, #87653, #7670, #80107, #64558, #6287, #28534, #65013, #57426, #58357, #15246, #44104, #87197, #86267, #22345, #22804, #28993, #85806, #51216, #35158, #21418, #113, #8138, #56968, #65935, #49825, #67310, #45969, #32240, #17578, #81483, #2440, #46427, #75330, #52602, #24193, #89043, #74875, #1964, #45027, #10445, #15715, #66825, #38401, #24670, #37921, #1495, #39311, #53070, #80562, #61148, #31318, #59270, #81945, #44577, #60205, #51671 ),
 .UNSPECIFIED., .F., .F.,
 ( 4, 1, 1, 1, 2, 2, 2, 2, 2, 2, 2, 2, 2, 2, 2, 2, 2, 2, 2, 2, 2, 2, 2, 2, 2, 2, 2, 2, 2, 2, 2, 2, 2, 2, 2, 2, 2, 2, 2, 2, 2, 2, 2, 2, 2, 2, 2, 2, 2, 2, 2, 2, 2, 2, 2, 2, 2, 2, 2, 2, 2, 2, 2, 2, 2, 2, 2, 2, 2, 2, 2, 2, 2, 2, 2, 2, 2, 2, 2, 2, 2, 2, 2, 2, 2, 2, 2, 2, 2, 2, 2, 2, 2, 2, 2, 2, 2, 2, 2, 2, 2, 2, 2, 2, 2, 2, 2, 2, 2, 2, 2, 2, 2, 2, 2, 2, 2, 2, 2, 2, 2, 2, 2, 2, 2, 2, 2, 2, 2, 2, 2, 2, 2, 2, 2, 2, 2, 2, 2, 2, 2, 2, 2, 2, 2, 2, 2, 2, 2, 2, 2, 2, 2, 2, 2, 2, 2, 2, 2, 2, 2, 2, 2, 2, 2, 2, 2, 2, 2, 2, 2, 2, 2, 2, 2, 2, 2, 2, 2, 2, 2, 2, 2, 2, 2, 2, 2, 2, 2, 2, 2, 2, 2, 2, 2, 2, 2, 2, 2, 2, 2, 2, 2, 2, 2, 2, 2, 2, 2, 2, 2, 2, 2, 2, 2, 2, 2, 2, 2, 2, 2, 2, 2, 2, 2, 2, 2, 2, 2, 2, 2, 2, 2, 2, 2, 2, 2, 2, 2, 2, 2, 2, 2, 2, 2, 2, 2, 2, 2, 2, 2, 2, 2, 2, 2, 2, 2, 2, 2, 2, 2, 2, 2, 2, 2, 2, 2, 2, 2, 2, 2, 2, 2, 2, 2, 2, 2, 2, 2, 2, 2, 2, 2, 2, 2, 2, 2, 2, 2, 2, 2, 2, 2, 2, 2, 2, 2, 2, 2, 2, 2, 2, 4 ),
 ( -0.05114157420909415386, -0.02298090003068697235, -0.008900562941483385060, -0.001860394396881591417, -0.0001003522607311430059, 0.0007796688073440846689, 0.001659689875419305405, 0.005179774147720181410, 0.008699858420021057415, 0.01221994269232193342, 0.01397998482847236101, 0.01574002696462277473, 0.01926011123692361604, 0.02278019550922444347, 0.02630027978152527091, 0.02806032191767569850, 0.02982036405382612609, 0.03334044832612698128, 0.03686053259842785035, 0.04038061687072870554, 0.04214065900687911925, 0.04390070114302953297, 0.04742078541533041591, 0.05094086968763129886, 0.05446095395993218180, 0.05622099609608263715, 0.05798103823223307862, 0.06150112250453390605, 0.06502120677683471961, 0.06854129104913554704, 0.07030133318528596076, 0.07206137532143638835, 0.07558145959373727130, 0.07910154386603812648, 0.08262162813833900943, 0.08438167027448945090, 0.08614171241063992013, 0.08966179668294077532, 0.09318188095524163050, 0.09670196522754251345, 0.09846200736369295492, 0.1002220494998433964, 0.1037421337721442793, 0.1072622180444451623, 0.1107823023167460175, 0.1143023865890469004, 0.1178224708613477834, 0.1213425551336486385, 0.1248626394059495215, 0.1283827236782504044, 0.1301427658144008181, 0.1319028079505512596, 0.1354228922228521148, 0.1389429764951529978, 0.1424630607674538807, 0.1442231029036042944, 0.1459831450397547081, 0.1495032293120556466, 0.1530233135843565850, 0.1565433978566575512, 0.1583034399928080482, 0.1600634821289586007, 0.1635835664012597057, 0.1671036506735608385, 0.1706237349458619434, 0.1723837770820125237, 0.1741438192181630762, 0.1776639034904642367, 0.1811839877627653972, 0.1847040720350665299, 0.1864641141712171102, 0.1882241563073677459, 0.1917442405796688787, 0.1952643248519700392, 0.1987844091242711719, 0.2005444512604217522, 0.2023044933965723602, 0.2058245776688735207, 0.2093446619411746812, 0.2128647462134758417, 0.2146247883496263942, 0.2163848304857770022, 0.2199049147580781627, 0.2234249990303793787, 0.2269450833026805947, 0.2287051254388311472, 0.2304651675749816997, 0.2339852518472829157, 0.2375053361195841317, 0.2410254203918853477, 0.2427854625280359002, 0.2445455046641863972, 0.2480655889364875022, 0.2515856732087886072, 0.2551057574810897122, 0.2568657996172403202, 0.2586258417533908172, 0.2621459260256919221, 0.2656660102979930271, 0.2691860945702941321, 0.2709461367064446846, 0.2727061788425952371, 0.2762262631148963421, 0.2797463473871973916, 0.2832664316594984966, 0.2850264737956491601, 0.2867865159317997126, 0.2903066002041009286, 0.2938266844764020891, 0.2973467687487033051, 0.2991068108848539131, 0.3008668530210045211, 0.3043869372933057371, 0.3079070215656068976, 0.3114271058379081136, 0.3131871479740586661, 0.3149471901102093296, 0.3184672743825104901, 0.3219873586548117061, 0.3255074429271129222, 0.3272674850632635302, 0.3290275271994141937, 0.3325476114717154652, 0.3360676957440166812, 0.3395877800163179527, 0.3413478221524685607, 0.3431078642886192243, 0.3466279485609204958, 0.3501480328332218228, 0.3536681171055230943, 0.3571882013778244214, 0.3607082856501256929, 0.3642283699224270199, 0.3677484541947282914, 0.3712685384670296185, 0.3730285806031802820, 0.3747886227393308900, 0.3783087070116322725, 0.3818287912839335996, 0.3853488755562349266, 0.3871089176923856456, 0.3888689598285362536, 0.3923890441008375807, 0.3959091283731389632, 0.3994292126454403458, 0.4011892547815910093, 0.4029492969177416173, 0.4064693811900430553, 0.4099894654623443824, 0.4135095497346458204, 0.4152695918707965395, 0.4170296340069470920, 0.4205497182792485300, 0.4240698025515499126, 0.4275898868238513506, 0.4293499289600020141, 0.4311099710961525666, 0.4346300553684539492, 0.4381501396407551652, 0.4416702239130565477, 0.4434302660492072112, 0.4451903081853577637, 0.4487103924576591463, 0.4522304767299604178, 0.4557505610022617448, 0.4575106031384122973, 0.4592706452745629608, 0.4627907295468641768, 0.4663108138191653929, 0.4698308980914666089, 0.4715909402276171614, 0.4733509823637678249, 0.4768710666360691519, 0.4803911509083702569, 0.4839112351806714729, 0.4856712773168221364, 0.4874313194529727999, 0.4909514037252741270, 0.4944714879975753430, 0.4979915722698766700, 0.4997516144060273335, 0.5015116565421779971, 0.5050317408144793241, 0.5085518250867805401, 0.5120719093590818671, 0.5138319514952325306, 0.5155919936313831942, 0.5191120779036842992, 0.5226321621759855152, 0.5261522464482867312, 0.5279122885844372837, 0.5296723307205878362, 0.5331924149928890522, 0.5367124992651902682, 0.5402325835374913732, 0.5419926256736420367, 0.5437526678097925892, 0.5472727520820938052, 0.5507928363543951322, 0.5543129206266964593, 0.5560729627628470118, 0.5578330048989975642, 0.5613530891712987803, 0.5648731734436001073, 0.5683932577159014343, 0.5701532998520520978, 0.5719133419882027614, 0.5754334262605039774, 0.5789535105328053044, 0.5824735948051066314, 0.5842336369412572949, 0.5859936790774079585, 0.5895137633497090635, 0.5930338476220103905, 0.5965539318943114955, 0.6000740161666127115, 0.6035941004389139275, 0.6071141847112151435, 0.6106342689835162485, 0.6141543532558175755, 0.6159143953919681280, 0.6176744375281187915, 0.6211945218004200076, 0.6247146060727212236, 0.6282346903450223286, 0.6299947324811729921, 0.6317547746173236556, 0.6352748588896248716, 0.6387949431619260876, 0.6423150274342271926, 0.6440750695703779671, 0.6458351117065286306, 0.6493551959788298467, 0.6528752802511311737, 0.6563953645234323897, 0.6581554066595831642, 0.6599154487957338278, 0.6634355330680350438, 0.6669556173403363708, 0.6704757016126375868, 0.6722357437487883614, 0.6739957858849390249, 0.6775158701572402409, 0.6810359544295415679, 0.6845560387018427839, 0.6863160808379935585, 0.6880761229741442220, 0.6915962072464454380, 0.6951162915187467650, 0.6986363757910479810, 0.7003964179271987556, 0.7021564600633494191, 0.7056765443356506351, 0.7091966286079519621, 0.7127167128802531781, 0.7144767550164039527, 0.7162367971525546162, 0.7197568814248558322, 0.7232769656971571592, 0.7267970499694583753, 0.7285570921056091498, 0.7303171342417598133, 0.7338372185140609183, 0.7373573027863620233, 0.7408773870586633503, 0.7426374291948140138, 0.7443974713309645663, 0.7479175556032657823, 0.7514376398755669983, 0.7549577241478682144, 0.7567177662840187669, 0.7584778084201693193, 0.7619978926924704243, 0.7655179769647714183, 0.7690380612370726343, 0.7707981033732231868, 0.7725581455093736283, 0.7760782297816749553, 0.7795983140539760603, 0.7831183983262772763, 0.7848784404624279398, 0.7866384825985783813, 0.7901585668708795973, 0.7936786511431808133, 0.7971987354154820293, 0.7989587775516325818, 0.8007188196877832453, 0.8042389039600844614, 0.8077589882323856774, 0.8112790725046868934, 0.8130391146408373348, 0.8147991567769879984, 0.8183192410492892144, 0.8218393253215903194, 0.8253594095938916464, 0.8271194517300421989, 0.8288794938661928624, 0.8323995781384940784, 0.8359196624107952944, 0.8394397466830965104, 0.8429598309553976154, 0.8464799152276989425, 0.8499999995000000474 ),
 .UNSPECIFIED. ) ;
#20962 = CARTESIAN_POINT ( 'NONE',  ( 37.55594080225193210, -277.6337173120213038, -276.7149992892133810 ) ) ;
#20963 = CARTESIAN_POINT ( 'NONE',  ( -4.407434547962546745, -272.4859908285420147, -202.9649056997094476 ) ) ;
#20964 = LINE ( 'NONE', #78728, #36226 ) ;
#20965 = CARTESIAN_POINT ( 'NONE',  ( 210.1640492649781322, 37.84931640281058662, 13.95110425196124027 ) ) ;
#20966 = CARTESIAN_POINT ( 'NONE',  ( -108.2114402159723028, -282.8714997662547148, -245.6595842048252791 ) ) ;
#20967 = CARTESIAN_POINT ( 'NONE',  ( 175.2296996224750103, 247.0000000000001137, 0.000000000000000000 ) ) ;
#20968 = CARTESIAN_POINT ( 'NONE',  ( 1.768504347131608645, -293.3115930758016816, -332.5302597307751853 ) ) ;
#20969 = CARTESIAN_POINT ( 'NONE',  ( 24.52604001798687250, -286.2518659473237221, -311.4117337935249452 ) ) ;
#20970 = DIRECTION ( 'NONE',  ( -1.000000000000000000, -0.000000000000000000, 0.000000000000000000 ) ) ;
#20971 = PLANE ( 'NONE',  #57870 ) ;
#20972 = CARTESIAN_POINT ( 'NONE',  ( -31.47052432468297312, -292.9779849412669250, -345.1824508631195272 ) ) ;
#20973 = CARTESIAN_POINT ( 'NONE',  ( -105.1767457852696026, -282.5762602560212144, -305.4209095206774691 ) ) ;
#20974 = CARTESIAN_POINT ( 'NONE',  ( -106.2686978920281291, -280.5023525591585098, -243.8453675696348171 ) ) ;
#20975 = CARTESIAN_POINT ( 'NONE',  ( -113.9572554671480162, -285.7259166477047643, -272.8517141236003454 ) ) ;
#20976 = CARTESIAN_POINT ( 'NONE',  ( 37.66393624701710507, -279.9472852888584953, -282.6130566177410515 ) ) ;
#20977 = CARTESIAN_POINT ( 'NONE',  ( 24.95072229601622027, -287.0277528565018770, -232.2999289767265054 ) ) ;
#20978 = CARTESIAN_POINT ( 'NONE',  ( -48.68086744841769331, -278.6245043657041265, -343.1232920335880863 ) ) ;
#20979 = CARTESIAN_POINT ( 'NONE',  ( -78.71491368497885333, -278.4279185479413741, -330.7623315307636744 ) ) ;
#20980 = CARTESIAN_POINT ( 'NONE',  ( -99.65097874842462033, -287.1041281900666604, -227.8901231934778195 ) ) ;
#20981 = ORIENTED_EDGE ( 'NONE', *, *, #93067, .F. ) ;
#20982 = CARTESIAN_POINT ( 'NONE',  ( -105.2526074958591806, -296.8557454040462176, -233.9560239301554816 ) ) ;
#20983 = CARTESIAN_POINT ( 'NONE',  ( -2.578389189232592749, -290.5703104147995077, -336.4741027412723042 ) ) ;
#20984 = CARTESIAN_POINT ( 'NONE',  ( 197.3474984796250169, 24.88324032512257844, 12.41094495000513298 ) ) ;
#20985 = CARTESIAN_POINT ( 'NONE',  ( -119.3990491898856732, -287.0519495502701943, -270.3937649182068412 ) ) ;
#20986 = ORIENTED_EDGE ( 'NONE', *, *, #13330, .T. ) ;
#20987 = CARTESIAN_POINT ( 'NONE',  ( -57.60236806042784252, -271.7911514786489988, -197.9223941613907698 ) ) ;
#20988 = CARTESIAN_POINT ( 'NONE',  ( 25.84110480896405804, -291.3838489219122039, -227.6727997809887256 ) ) ;
#20989 = CARTESIAN_POINT ( 'NONE',  ( -105.0212628728115476, -295.6914460922606622, -297.8832041714238130 ) ) ;
#20990 = CARTESIAN_POINT ( 'NONE',  ( 33.32942174276556813, -288.7979529030894241, -249.4288412032416602 ) ) ;
#20991 = PRODUCT ( 'High-Pressure Air Hose', 'High-Pressure Air Hose', '', ( #24624 ) ) ;
#20992 = CARTESIAN_POINT ( 'NONE',  ( 33.70105190369956460, -283.0414435020989572, -249.6029533667195324 ) ) ;
#20993 = CARTESIAN_POINT ( 'NONE',  ( -99.38116766687564052, -291.3813436920794402, -314.9897021226811944 ) ) ;
#20994 = CARTESIAN_POINT ( 'NONE',  ( -110.3064229726024763, -291.5743301758000143, -293.5437952325392530 ) ) ;
#20995 = CARTESIAN_POINT ( 'NONE',  ( -84.02010819400756247, -285.6932732885861128, -329.1314622496981315 ) ) ;
#20996 = CARTESIAN_POINT ( 'NONE',  ( -54.12918068643331537, -277.4285212899328030, -345.5634825142376485 ) ) ;
#20997 = VERTEX_POINT ( 'NONE', #48999 ) ;
#20998 = CARTESIAN_POINT ( 'NONE',  ( -63.78556762282077131, -293.4741203252553987, -341.1427262545600456 ) ) ;
#20999 = CARTESIAN_POINT ( 'NONE',  ( 31.07617318620259539, -281.8408462702693100, -305.6880852403859876 ) ) ;
#21000 = CARTESIAN_POINT ( 'NONE',  ( -40.85674713035532335, -275.8680216950203885, -196.1586392236647498 ) ) ;
#21001 = CARTESIAN_POINT ( 'NONE',  ( 39.58706461736021254, -290.0519495502703080, -270.3284710469133074 ) ) ;
#21002 = CARTESIAN_POINT ( 'NONE',  ( 37.22868403769292911, -273.6069568449494795, -255.7586585530844445 ) ) ;
#21003 = FACE_OUTER_BOUND ( 'NONE', #74970, .T. ) ;
#21004 = CARTESIAN_POINT ( 'NONE',  ( 22.16725555787966684, -280.4681939593478432, -227.9739426233922188 ) ) ;
#21005 = CARTESIAN_POINT ( 'NONE',  ( -113.6498229292669606, -279.8489205516154925, -263.0670781371906060 ) ) ;
#21006 = CARTESIAN_POINT ( 'NONE',  ( -100.4110810367438091, -298.4961095583690849, -232.3459152040091737 ) ) ;
#21007 = CARTESIAN_POINT ( 'NONE',  ( -16.21812605038069321, -281.8444377094382958, -344.2174164699054586 ) ) ;
#21008 = CARTESIAN_POINT ( 'NONE',  ( -110.7076259378346208, -292.4443482789500308, -260.2120705860857584 ) ) ;
#21009 = CARTESIAN_POINT ( 'NONE',  ( -67.24071266760248022, -275.2667106382818361, -200.2719642868421488 ) ) ;
#21010 = CARTESIAN_POINT ( 'NONE',  ( -80.98291549295413461, -274.7886540384796490, -207.4578900942628650 ) ) ;
#21011 = DIRECTION ( 'NONE',  ( 1.000000000000000000, -0.000000000000000000, 0.000000000000000000 ) ) ;
#21012 = CARTESIAN_POINT ( 'NONE',  ( -7.227749053095210208, -296.6564308410267472, -338.8818150961515130 ) ) ;
#21013 = CARTESIAN_POINT ( 'NONE',  ( -97.40816235265968714, -281.9413254738955175, -314.9934890276267083 ) ) ;
#21014 = CARTESIAN_POINT ( 'NONE',  ( -68.31636199602947102, -291.3230275388935411, -199.8746715106072998 ) ) ;
#21015 = CARTESIAN_POINT ( 'NONE',  ( 8.572711529114068085, -274.4402099682191647, -329.2802861744372080 ) ) ;
#21016 = CARTESIAN_POINT ( 'NONE',  ( -3.859450391070875064, -288.0865563404634031, -201.8969122317749907 ) ) ;
#21017 = CARTESIAN_POINT ( 'NONE',  ( -93.66855322616524404, -290.1355808120229085, -223.4212561549220766 ) ) ;
#21018 = VERTEX_POINT ( 'NONE', #77898 ) ;
#21019 = CARTESIAN_POINT ( 'NONE',  ( -113.8007302467491542, -289.1162581910467111, -271.2040025293756571 ) ) ;
#21020 = CARTESIAN_POINT ( 'NONE',  ( -98.86186408727481023, -289.6749262385654333, -309.6975757944746874 ) ) ;
#21021 = EDGE_LOOP ( 'NONE', ( #11984, #48862, #42087 ) ) ;
#21022 = CARTESIAN_POINT ( 'NONE',  ( 36.49057284273963830, -288.8933597157793542, -291.1526935178251847 ) ) ;
#21023 = CARTESIAN_POINT ( 'NONE',  ( 17.45390565889626444, -276.5746131182507952, -318.6451781088040889 ) ) ;
#21024 = CARTESIAN_POINT ( 'NONE',  ( 13.18181335384396391, -293.2858785741150882, -328.1278525517369644 ) ) ;
#21025 = CARTESIAN_POINT ( 'NONE',  ( -58.45079190907373601, -283.9693619512170812, -344.3605674878631930 ) ) ;
#21026 = CARTESIAN_POINT ( 'NONE',  ( -91.89100066589773519, -285.6326949933856554, -216.0461283174732614 ) ) ;
#21028 = CARTESIAN_POINT ( 'NONE',  ( 17.62357177023229937, -282.5711191151791581, -318.4330055258355969 ) ) ;
#21027 = AXIS2_PLACEMENT_3D ( 'NONE', #5836, #78276, #49834 ) ;
#21029 = CARTESIAN_POINT ( 'NONE',  ( -56.32961566068995296, -169.3491268111188219, -364.4629006607140127 ) ) ;
#21030 = CARTESIAN_POINT ( 'NONE',  ( 198.4191458182635017, 289.3439720879956099, -97.25198484077063199 ) ) ;
#21031 = CARTESIAN_POINT ( 'NONE',  ( -112.1541305756452402, -270.5365672045004430, -270.3354547578530287 ) ) ;
#21032 = CARTESIAN_POINT ( 'NONE',  ( -62.07469003415040731, -272.9193124220362847, -201.5070626395322790 ) ) ;
#21033 = CARTESIAN_POINT ( 'NONE',  ( -36.71969321418954024, -272.9804737547783589, -197.0421757620138123 ) ) ;
#21034 = CARTESIAN_POINT ( 'NONE',  ( -19.30779366272476949, -294.3339289529244525, -345.2110462503962367 ) ) ;
#21035 = CARTESIAN_POINT ( 'NONE',  ( -87.69934636623491997, -230.2613027696342840, -344.8992764788239356 ) ) ;
#21036 = CARTESIAN_POINT ( 'NONE',  ( -36.92548852504683765, -272.7421257071342779, -193.8424301553349949 ) ) ;
#21037 = CARTESIAN_POINT ( 'NONE',  ( -35.80686752662442274, -299.9319789466649127, -196.1254176205127067 ) ) ;
#21038 = CARTESIAN_POINT ( 'NONE',  ( 1.586900746562427189, -289.8349396974593333, -332.6973635512485430 ) ) ;
#21039 = CARTESIAN_POINT ( 'NONE',  ( -110.5552296144252438, -291.6926677895818329, -265.7297335455925804 ) ) ;
#21040 = ORIENTED_EDGE ( 'NONE', *, *, #91063, .T. ) ;
#21041 = CARTESIAN_POINT ( 'NONE',  ( -112.9096099239331039, -297.6627823977966614, -256.8588506751494833 ) ) ;
#21042 = CARTESIAN_POINT ( 'NONE',  ( 29.48388025221274944, -288.4431397842553793, -300.0219005406169686 ) ) ;
#21043 = CARTESIAN_POINT ( 'NONE',  ( 24.76181545558662123, -294.9570124622788398, -315.6305189611206856 ) ) ;
#21044 = CARTESIAN_POINT ( 'NONE',  ( -36.26901294854877023, -295.5314227784099899, -347.3051948174285712 ) ) ;
#21045 = CARTESIAN_POINT ( 'NONE',  ( 35.42460380009403309, -293.7958266790826087, -276.1976423869222117 ) ) ;
#21046 = ORIENTED_EDGE ( 'NONE', *, *, #89041, .F. ) ;
#21047 = CARTESIAN_POINT ( 'NONE',  ( 24.14068485488863658, -276.8791087063765985, -226.4159862955499420 ) ) ;
#21048 = EDGE_CURVE ( 'NONE', #83682, #21221, #10913, .T. ) ;
#21049 = ORIENTED_EDGE ( 'NONE', *, *, #5869, .T. ) ;
#21050 = CARTESIAN_POINT ( 'NONE',  ( -91.01074608189379944, -278.8225538302208975, -215.1582707267325532 ) ) ;
#21051 = CARTESIAN_POINT ( 'NONE',  ( 20.49504038287555119, -273.3118124547708589, -224.5003849545063304 ) ) ;
#21052 = CARTESIAN_POINT ( 'NONE',  ( 20.03237936985398449, -275.8527811600368409, -224.8259661269908065 ) ) ;
#21053 = CARTESIAN_POINT ( 'NONE',  ( -24.35513660618481779, -275.9757496940782175, -195.4389608324812002 ) ) ;
#21054 = CARTESIAN_POINT ( 'NONE',  ( 37.29853088105747361, -273.4399196808178090, -260.0053119979341432 ) ) ;
#21055 = CARTESIAN_POINT ( 'NONE',  ( -82.01295401248555095, -298.0764271405614068, -212.4318408627218275 ) ) ;
#21056 = CARTESIAN_POINT ( 'NONE',  ( -110.8310390908306573, -295.0767137119880772, -274.1941291371088028 ) ) ;
#21057 = DIRECTION ( 'NONE',  ( -0.000000000000000000, -0.000000000000000000, -1.000000000000000000 ) ) ;
#21058 = CARTESIAN_POINT ( 'NONE',  ( -104.7426967551842978, -279.5254439140075533, -233.2581186867105032 ) ) ;
#21059 = CARTESIAN_POINT ( 'NONE',  ( -45.90599148361290105, -277.3303090215767384, -342.9076257397211975 ) ) ;
#21060 = CARTESIAN_POINT ( 'NONE',  ( 36.90234632908327939, -286.0044285509882229, -251.8916881014038438 ) ) ;
#21061 = CARTESIAN_POINT ( 'NONE',  ( -109.8903953936069513, -274.7990515606630879, -251.1440210749231596 ) ) ;
#21062 = CARTESIAN_POINT ( 'NONE',  ( 82.64408888120264862, -299.9321935367201490, -197.8381816864644520 ) ) ;
#21063 = CARTESIAN_POINT ( 'NONE',  ( 33.23496061135709567, -287.0056384659935134, -289.8243024082034367 ) ) ;
#21064 = CARTESIAN_POINT ( 'NONE',  ( 5.528082745358883443, -278.8815090242043766, -210.0274148995039809 ) ) ;
#21065 = CARTESIAN_POINT ( 'NONE',  ( -7.745948802577005132, -279.0225108815593558, -202.9717709099863328 ) ) ;
#21066 = CARTESIAN_POINT ( 'NONE',  ( -67.46184869737096790, -285.4473543557164703, -339.0610184254437627 ) ) ;
#21067 = CARTESIAN_POINT ( 'NONE',  ( 15.89640231059415854, -277.4815847903368535, -320.8867051006063775 ) ) ;
#21068 = FACE_OUTER_BOUND ( 'NONE', #68565, .T. ) ;
#21069 = CARTESIAN_POINT ( 'NONE',  ( -5.727086149433370466, -274.8819777967572691, -339.4588039038982288 ) ) ;
#21070 = CARTESIAN_POINT ( 'NONE',  ( 20.75750026452003283, -275.5802556465244493, -225.9741374621141574 ) ) ;
#21071 = CARTESIAN_POINT ( 'NONE',  ( 35.54709598299938023, -283.3169278434688749, -251.9967004419412149 ) ) ;
#21072 = CARTESIAN_POINT ( 'NONE',  ( 208.4306832106271088, 0.04196010845015941959, 7.500000000000013323 ) ) ;
#21073 = CARTESIAN_POINT ( 'NONE',  ( 35.75763782286033177, -289.7162696096799550, -289.4870425833998979 ) ) ;
#21074 = CARTESIAN_POINT ( 'NONE',  ( 25.08619535696503178, -292.1138942037821380, -311.9504398847830657 ) ) ;
#21075 = CARTESIAN_POINT ( 'NONE',  ( 82.15506381819601245, -299.0670410310526108, -197.3076072666646326 ) ) ;
#21076 = CARTESIAN_POINT ( 'NONE',  ( -68.47635553081295257, -272.3191494584230554, -203.7749868104250197 ) ) ;
#21077 = CARTESIAN_POINT ( 'NONE',  ( 36.13362775344320710, -291.5542996729639640, -259.7667009052776166 ) ) ;
#21078 = CARTESIAN_POINT ( 'NONE',  ( 89.65909921107042635, 79.73535476480827811, -300.8268380169218972 ) ) ;
#21079 = DIRECTION ( 'NONE',  ( 0.4988042400434494761, -0.06911816301596634959, -0.8639542867860402486 ) ) ;
#21080 = CARTESIAN_POINT ( 'NONE',  ( -69.08668196632139313, -287.9419974301690104, -339.7653544813170470 ) ) ;
#21081 = CARTESIAN_POINT ( 'NONE',  ( -65.60341423208502931, -285.0281113846423864, -338.5490225238742710 ) ) ;
#21082 = CARTESIAN_POINT ( 'NONE',  ( 11.44437779676107780, -284.9573874184537772, -212.0353161358927423 ) ) ;
#21083 = CARTESIAN_POINT ( 'NONE',  ( -42.95993448864535225, -284.5495851033617214, -343.7860621014394269 ) ) ;
#21084 = CARTESIAN_POINT ( 'NONE',  ( -109.6563736073138244, -285.2046216848851259, -281.7849389376270892 ) ) ;
#21085 = CARTESIAN_POINT ( 'NONE',  ( -91.64468435172817351, -293.2635032283860141, -218.0413508963960112 ) ) ;
#21086 = CIRCLE ( 'NONE', #90590, 0.4999999999999989453 ) ;
#21087 = CARTESIAN_POINT ( 'NONE',  ( 30.55047328220840441, -274.0673387295746011, -303.6459637433583225 ) ) ;
#21088 = CARTESIAN_POINT ( 'NONE',  ( -44.04514827787810560, -274.3030101501432796, -193.6213972867191444 ) ) ;
#21089 = CARTESIAN_POINT ( 'NONE',  ( -93.62209232859034103, -289.3289734142277894, -219.9445368509293246 ) ) ;
#21090 = CARTESIAN_POINT ( 'NONE',  ( 14.88317882177516971, -276.3404187383079602, -327.0160342192095300 ) ) ;
#21091 = CARTESIAN_POINT ( 'NONE',  ( 31.00599725859574107, -295.9268299466259577, -300.3684347852315000 ) ) ;
#21092 = CARTESIAN_POINT ( 'NONE',  ( 156.5191989162425727, 249.5000000000000568, 16.58062614384861178 ) ) ;
#21093 = CARTESIAN_POINT ( 'NONE',  ( 35.77081079830085031, -295.8376638359844719, -253.6410175316879361 ) ) ;
#21094 = CARTESIAN_POINT ( 'NONE',  ( -106.9943554979259801, -283.5482330340972226, -246.7551050580815968 ) ) ;
#21095 = EDGE_CURVE ( 'NONE', #75426, #34536, #47579, .T. ) ;
#21096 = CARTESIAN_POINT ( 'NONE',  ( 2.774307903011629772, -278.5897569054384917, -206.9301572612380937 ) ) ;
#21097 = EDGE_CURVE ( 'NONE', #82136, #26035, #39627, .T. ) ;
#21098 = CARTESIAN_POINT ( 'NONE',  ( -113.1714934331925377, -271.1395254068419263, -261.8434775121861549 ) ) ;
#21099 = CARTESIAN_POINT ( 'NONE',  ( -61.83177852398269181, -276.7274862005567684, -339.2925720075747904 ) ) ;
#21100 = CARTESIAN_POINT ( 'NONE',  ( 26.82886369925037684, -294.5797277384135668, -234.0237491028881038 ) ) ;
#21101 = CARTESIAN_POINT ( 'NONE',  ( 27.37158344524206299, -294.9602609106559044, -304.7565312643018842 ) ) ;
#21102 = CARTESIAN_POINT ( 'NONE',  ( -11.20980534635519810, -296.0339181902334076, -342.3229789612057061 ) ) ;
#21103 = CARTESIAN_POINT ( 'NONE',  ( -107.6033856567162559, -296.1236479623738092, -290.1675702442213378 ) ) ;
#21104 = CARTESIAN_POINT ( 'NONE',  ( -9.971109543656687890, -290.6950696756996422, -340.2441247845581529 ) ) ;
#21105 = CARTESIAN_POINT ( 'NONE',  ( -105.7831740440014840, -284.2627908078724204, -305.7586700857913797 ) ) ;
#21106 = CARTESIAN_POINT ( 'NONE',  ( -35.52919970570834352, -272.2142258109196291, -194.6050780441710231 ) ) ;
#21107 = CARTESIAN_POINT ( 'NONE',  ( -30.88173815167097302, -285.9649563307573317, -193.6192828684417009 ) ) ;
#21108 = CARTESIAN_POINT ( 'NONE',  ( -29.51647577905713504, -278.9325948321531428, -344.6466729639312234 ) ) ;
#21109 = CARTESIAN_POINT ( 'NONE',  ( -5.686123378546612095, -285.5376497310342643, -204.3069002407272592 ) ) ;
#21110 = CARTESIAN_POINT ( 'NONE',  ( -100.6276949432456860, -288.0092793917290805, -310.7045135057646235 ) ) ;
#21111 = CARTESIAN_POINT ( 'NONE',  ( 122.2132510144744231, 146.9671518294229884, -260.0597590233358574 ) ) ;
#21112 = CARTESIAN_POINT ( 'NONE',  ( 31.03440590732131099, -286.7148616216642836, -244.4753765253276754 ) ) ;
#21113 = CARTESIAN_POINT ( 'NONE',  ( 19.61700487003165350, -283.1950339229233009, -321.9027351537781669 ) ) ;
#21114 = CARTESIAN_POINT ( 'NONE',  ( -74.55430958609520076, -290.6282217033115671, -203.2191645515357266 ) ) ;
#21115 = CARTESIAN_POINT ( 'NONE',  ( -48.02696793397387154, -281.5186604497420717, -194.8607274821272028 ) ) ;
#21116 = CARTESIAN_POINT ( 'NONE',  ( -106.9772587562155195, -280.2764112352208485, -238.5445908078931438 ) ) ;
#21117 = CARTESIAN_POINT ( 'NONE',  ( 2.705758260382665537, -280.4388651034481086, -209.2660366015047657 ) ) ;
#21118 = CARTESIAN_POINT ( 'NONE',  ( -13.45184927674018738, -276.3625292210851399, -199.2676887956133953 ) ) ;
#21119 = CARTESIAN_POINT ( 'NONE',  ( 8.906156743853365754, -294.4371410363464179, -331.9251962648914969 ) ) ;
#21120 = CARTESIAN_POINT ( 'NONE',  ( -74.38258807489297908, -287.5673298601061560, -335.1818703558597008 ) ) ;
#21121 = CARTESIAN_POINT ( 'NONE',  ( -27.96792527687896168, -293.7692496346715529, -194.6867571202456304 ) ) ;
#21122 = CARTESIAN_POINT ( 'NONE',  ( -97.44465230440238201, -294.8896874827739794, -312.3356485179066908 ) ) ;
#21123 = EDGE_LOOP ( 'NONE', ( #33789, #34515, #77819 ) ) ;
#21124 = CARTESIAN_POINT ( 'NONE',  ( -10.43285348184764949, -284.6185987577881633, -339.8220185831044660 ) ) ;
#21125 = CARTESIAN_POINT ( 'NONE',  ( -103.7360461296461551, -296.6301310111882685, -239.8440627133898886 ) ) ;
#21126 = CARTESIAN_POINT ( 'NONE',  ( -13.97377717797410490, -293.4279248445182020, -197.2613249583244510 ) ) ;
#21127 = CARTESIAN_POINT ( 'NONE',  ( 31.45334110770835068, -282.5341158614627375, -295.2319777552705773 ) ) ;
#21128 = CARTESIAN_POINT ( 'NONE',  ( -63.46572195458924170, -272.7786107733008407, -198.1783243518403310 ) ) ;
#21129 = CARTESIAN_POINT ( 'NONE',  ( -23.32236650191881111, -289.5289617630800194, -346.0244937158390712 ) ) ;
#21130 = CARTESIAN_POINT ( 'NONE',  ( -0.9892477441648872549, -280.7145429992540926, -336.8499056821429463 ) ) ;
#21131 = CARTESIAN_POINT ( 'NONE',  ( -112.9050191481909735, -291.0701167630201098, -255.5979045358685084 ) ) ;
#21132 = CARTESIAN_POINT ( 'NONE',  ( 35.14571657019750006, -288.0016543015505022, -279.1737173247350938 ) ) ;
#21133 = CARTESIAN_POINT ( 'NONE',  ( 209.2568086740256206, 34.98978593258856051, 15.00000000000000000 ) ) ;
#21134 = CARTESIAN_POINT ( 'NONE',  ( 153.8801639287781029, 129.5385997557426379, -11.85807839311486234 ) ) ;
#21135 = CARTESIAN_POINT ( 'NONE',  ( 202.4139397029900636, 292.0436245958289874, -68.22449661283333455 ) ) ;
#21136 = CARTESIAN_POINT ( 'NONE',  ( -20.19161114001082069, -271.7666405000205714, -195.3683826091709363 ) ) ;
#21137 = CARTESIAN_POINT ( 'NONE',  ( -76.90059059506310746, -278.7049333687505737, -208.7564712338032109 ) ) ;
#21138 = ORIENTED_EDGE ( 'NONE', *, *, #65268, .F. ) ;
#21139 = CARTESIAN_POINT ( 'NONE',  ( -69.86510219893355611, -278.5337602417895937, -204.6474865008337076 ) ) ;
#21140 = CARTESIAN_POINT ( 'NONE',  ( 2.410716822162965567, -274.2363688864952564, -204.4407900243765255 ) ) ;
#21141 = CARTESIAN_POINT ( 'NONE',  ( 198.5597165885725133, 282.1031016261414948, -110.8136125372897993 ) ) ;
#21142 = CARTESIAN_POINT ( 'NONE',  ( -56.39206956557844563, -278.3861985372600998, -196.3086388897377219 ) ) ;
#21143 = CARTESIAN_POINT ( 'NONE',  ( -95.58387239043544525, -281.9268742885003007, -317.0686768613675213 ) ) ;
#21144 = CARTESIAN_POINT ( 'NONE',  ( -86.81966061962245362, -299.1354330460225128, -212.6210731168986001 ) ) ;
#21145 = CARTESIAN_POINT ( 'NONE',  ( 24.89700902263355431, -293.5162968812755366, -231.9985016091159480 ) ) ;
#21146 = EDGE_LOOP ( 'NONE', ( #91677, #71969, #5321, #30801 ) ) ;
#21147 = CARTESIAN_POINT ( 'NONE',  ( -103.9965963978455363, -289.6520629994708429, -239.4035941822990878 ) ) ;
#21148 = CARTESIAN_POINT ( 'NONE',  ( 33.61628151908885798, -275.8246180384253989, -240.5878761696732226 ) ) ;
#21149 = CARTESIAN_POINT ( 'NONE',  ( -55.29571555057212606, -297.9814996829738902, -199.5510982856281714 ) ) ;
#21150 = ORIENTED_EDGE ( 'NONE', *, *, #37532, .F. ) ;
#21151 = CARTESIAN_POINT ( 'NONE',  ( 155.7140808774800007, 20.99999999999998934, -15.62500000000000711 ) ) ;
#21152 = VECTOR ( 'NONE', #92349, 1000.000000000000000 ) ;
#21153 = DIRECTION ( 'NONE',  ( 1.000000000000000000, 0.000000000000000000, 0.000000000000000000 ) ) ;
#21154 = CARTESIAN_POINT ( 'NONE',  ( -71.09618173569496946, -280.6754041129343022, -205.2711597043160054 ) ) ;
#21155 = CARTESIAN_POINT ( 'NONE',  ( -38.18149286942044540, -281.8018979483874205, -194.3790887557871656 ) ) ;
#21156 = AXIS2_PLACEMENT_3D ( 'NONE', #13871, #42723, #71168 ) ;
#21157 = CARTESIAN_POINT ( 'NONE',  ( -78.51878970601758567, -282.6805531654070478, -330.9239427311221675 ) ) ;
#21158 = CARTESIAN_POINT ( 'NONE',  ( -41.13764488955257548, -281.8642833332503415, -196.2230286819362561 ) ) ;
#21159 = CARTESIAN_POINT ( 'NONE',  ( 35.38826112719358008, -274.1912504007178768, -282.5458535948769168 ) ) ;
#21160 = DIRECTION ( 'NONE',  ( 0.000000000000000000, -1.000000000000000000, 0.000000000000000000 ) ) ;
#21161 = DIRECTION ( 'NONE',  ( -0.3428573139466628561, 0.000000000000000000, 0.9393874931428880526 ) ) ;
#21162 = CARTESIAN_POINT ( 'NONE',  ( -22.95907811108590835, -277.6756135734006534, -345.8956448764176912 ) ) ;
#21163 = CARTESIAN_POINT ( 'NONE',  ( 164.6329196456214277, 214.9910457053126720, 23.09031830825856346 ) ) ;
#21164 = ORIENTED_EDGE ( 'NONE', *, *, #34074, .T. ) ;
#21165 = CARTESIAN_POINT ( 'NONE',  ( 144.2857639756989272, -299.5541904835127980, -188.7068768330456123 ) ) ;
#21166 = CARTESIAN_POINT ( 'NONE',  ( -67.20580790827278861, -285.4216638236208041, -339.5459564341089731 ) ) ;
#21167 = CARTESIAN_POINT ( 'NONE',  ( 32.49790794043295250, -293.0375026586251010, -292.1563209385726054 ) ) ;
#21168 = CARTESIAN_POINT ( 'NONE',  ( 27.35454246723739757, -287.4478698461635418, -312.0250026353834869 ) ) ;
#21169 = CARTESIAN_POINT ( 'NONE',  ( -98.93814621192655068, -283.3538802424283745, -229.3263541432489205 ) ) ;
#21171 = CARTESIAN_POINT ( 'NONE',  ( -50.95960474744624946, -287.4682508542301775, -343.1632709709842857 ) ) ;
#21170 = CARTESIAN_POINT ( 'NONE',  ( -69.01220709553993515, -284.2020079797344465, -203.9216675777556418 ) ) ;
#21172 = CARTESIAN_POINT ( 'NONE',  ( 20.50333807851700030, -283.3905603016838768, -315.5394541738708085 ) ) ;
#21173 = CARTESIAN_POINT ( 'NONE',  ( -43.84331899308399727, -271.9699448504277939, -195.5915290422074122 ) ) ;
#21174 = CARTESIAN_POINT ( 'NONE',  ( -66.86014849885927447, -284.0716050805226018, -200.1108395333039596 ) ) ;
#21175 = CARTESIAN_POINT ( 'NONE',  ( -111.7925888053599408, -298.6686313517778331, -261.3020990961549046 ) ) ;
#21176 = CARTESIAN_POINT ( 'NONE',  ( -70.24028501929326751, -283.6194677641286717, -202.7762709860772645 ) ) ;
#21177 = CARTESIAN_POINT ( 'NONE',  ( -105.7383238995555814, -279.8435822688368830, -244.0405856772781306 ) ) ;
#21178 = CARTESIAN_POINT ( 'NONE',  ( 30.05516742116387618, -289.9917707600530434, -303.7605733105853005 ) ) ;
#21179 = CARTESIAN_POINT ( 'NONE',  ( 195.4562561984918148, 27.35676323194514126, 13.99999999999999822 ) ) ;
#21180 = CARTESIAN_POINT ( 'NONE',  ( 199.0061125298537377, 275.5000000000000568, -7.725424859374024678 ) ) ;
#21181 = CARTESIAN_POINT ( 'NONE',  ( 16.55193879744521013, -296.2138652272377044, -323.3958293713237140 ) ) ;
#21182 = CARTESIAN_POINT ( 'NONE',  ( -112.3505877992131872, -276.5846707956379191, -267.8156500431153404 ) ) ;
#21183 = CARTESIAN_POINT ( 'NONE',  ( -111.4743014381466963, -290.0035679183544062, -250.0994313474726880 ) ) ;
#21184 = CARTESIAN_POINT ( 'NONE',  ( 29.10607921092357131, -292.3832851757165372, -302.5901628751475414 ) ) ;
#21185 = CARTESIAN_POINT ( 'NONE',  ( -54.59240484389143688, -278.5107660067846496, -198.8686899550340854 ) ) ;
#21186 = CARTESIAN_POINT ( 'NONE',  ( -66.02852212518352815, -295.8122873910523936, -201.8926454901307181 ) ) ;
#21187 = CARTESIAN_POINT ( 'NONE',  ( -107.0442816173390241, -292.1746714847028557, -247.0631864953041372 ) ) ;
#21188 = CARTESIAN_POINT ( 'NONE',  ( -106.6662871844225293, -275.4805209788416960, -237.0123917617630696 ) ) ;
#21189 = CARTESIAN_POINT ( 'NONE',  ( 10.74623573116364916, -292.8814245578822693, -329.6766284268210256 ) ) ;
#21190 = CARTESIAN_POINT ( 'NONE',  ( -93.00181338863293945, -291.4680984658751299, -318.8976727400695381 ) ) ;
#21191 = CARTESIAN_POINT ( 'NONE',  ( 3.614486301459465700, -290.8344452406145706, -206.2943258002021309 ) ) ;
#21192 = CARTESIAN_POINT ( 'NONE',  ( -34.53751184212538305, -290.4416423302682801, -343.9468823945292115 ) ) ;
#21193 = FACE_BOUND ( 'NONE', #77112, .T. ) ;
#21194 = CARTESIAN_POINT ( 'NONE',  ( -0.9021591587043433780, -289.3582565351172207, -333.8604446192612727 ) ) ;
#21195 = DIRECTION ( 'NONE',  ( 1.000000000000000000, 0.000000000000000000, 0.000000000000000000 ) ) ;
#21196 = CARTESIAN_POINT ( 'NONE',  ( -93.29222475175984641, -291.0392984489857326, -322.7591251942047279 ) ) ;
#21198 = CARTESIAN_POINT ( 'NONE',  ( -99.71160790639525828, -291.0745972829884636, -232.4270356327176614 ) ) ;
#21197 = CARTESIAN_POINT ( 'NONE',  ( 36.08073246584901739, -279.3549051956842959, -253.3469468220091585 ) ) ;
#21199 = CARTESIAN_POINT ( 'NONE',  ( -79.90262721556769066, -279.8271021939681873, -206.1542720985193853 ) ) ;
#21200 = CARTESIAN_POINT ( 'NONE',  ( 38.77447446082106808, -281.0707796424130152, -258.5230041031413180 ) ) ;
#21201 = CARTESIAN_POINT ( 'NONE',  ( 37.55141082777899442, -285.4893312303795483, -265.4812786776086568 ) ) ;
#21202 = CARTESIAN_POINT ( 'NONE',  ( -112.1436901920290268, -274.5519900738175920, -270.3865807095265268 ) ) ;
#21203 = CARTESIAN_POINT ( 'NONE',  ( 34.84581001808292910, -279.9170585126622655, -287.7306951100896413 ) ) ;
#21204 = ADVANCED_FACE ( 'NONE', ( #39998 ), #34334, .F. ) ;
#21205 = CARTESIAN_POINT ( 'NONE',  ( -21.38401343115940278, -284.2566516355674366, -197.0784264318440933 ) ) ;
#21206 = CARTESIAN_POINT ( 'NONE',  ( 221.8344101925596306, 1.000000000000000222, 7.000000000000000000 ) ) ;
#21207 = CARTESIAN_POINT ( 'NONE',  ( -113.5406919127116367, -276.9808909827281127, -274.4134509030984646 ) ) ;
#21208 = CARTESIAN_POINT ( 'NONE',  ( 22.75826059940336066, -285.8322306536472297, -222.7010461313469989 ) ) ;
#21209 = CARTESIAN_POINT ( 'NONE',  ( -37.83609679892234823, -298.9870633562416629, -197.1274916838459603 ) ) ;
#21210 = DIRECTION ( 'NONE',  ( 0.000000000000000000, 1.000000000000000000, 0.000000000000000000 ) ) ;
#21211 = CARTESIAN_POINT ( 'NONE',  ( -77.70960297263444261, -293.1002333730833698, -208.5802727794157931 ) ) ;
#21212 = CARTESIAN_POINT ( 'NONE',  ( 36.70967539353675591, -276.7398320786147110, -251.5196722312257975 ) ) ;
#21213 = CARTESIAN_POINT ( 'NONE',  ( -110.1897712811958598, -278.1434978350496294, -276.0763131487547639 ) ) ;
#21214 = CARTESIAN_POINT ( 'NONE',  ( -14.97268084463497928, -296.7627049932192449, -342.0022565749762293 ) ) ;
#21215 = CARTESIAN_POINT ( 'NONE',  ( -81.93211057851669921, -291.6294689600409811, -207.5861603931744526 ) ) ;
#21216 = CARTESIAN_POINT ( 'NONE',  ( 19.07021333941937158, -278.9373534073271230, -220.0722790313181463 ) ) ;
#21217 = CARTESIAN_POINT ( 'NONE',  ( -8.509249530970711461, -292.2526113399259771, -198.9630101849645030 ) ) ;
#21219 = CARTESIAN_POINT ( 'NONE',  ( -108.6538487480726189, -289.8308538928027929, -253.6335571990357494 ) ) ;
#21218 = AXIS2_PLACEMENT_3D ( 'NONE', #53725, #23899, #2603 ) ;
#21220 = CARTESIAN_POINT ( 'NONE',  ( -32.17635856413464523, -292.9868597423189840, -345.1959494806206408 ) ) ;
#21221 = VERTEX_POINT ( 'NONE', #34795 ) ;
#21222 = FACE_OUTER_BOUND ( 'NONE', #73438, .T. ) ;
#21223 = CARTESIAN_POINT ( 'NONE',  ( -1.220801655145375086, -292.0528605345135134, -206.8386057230477491 ) ) ;
#21224 = DIRECTION ( 'NONE',  ( -0.000000000000000000, -0.000000000000000000, -1.000000000000000000 ) ) ;
#21225 = AXIS2_PLACEMENT_3D ( 'NONE', #20857, #86171, #58263 ) ;
#21226 = CARTESIAN_POINT ( 'NONE',  ( 7.399455738971487229, -279.9094976428775681, -326.5171145203363494 ) ) ;
#21227 = CARTESIAN_POINT ( 'NONE',  ( -109.2214567527080789, -295.2673111947250959, -297.4577819398419365 ) ) ;
#21228 = CARTESIAN_POINT ( 'NONE',  ( -78.87785338044611194, -284.9147102337576030, -334.6109914841913451 ) ) ;
#21229 = CARTESIAN_POINT ( 'NONE',  ( 33.99645877079259293, -287.1811639150399174, -254.8734748611770158 ) ) ;
#21230 = CARTESIAN_POINT ( 'NONE',  ( -7.206584965477648375, -278.1696225689579478, -337.6112673372305153 ) ) ;
#21231 = CARTESIAN_POINT ( 'NONE',  ( -34.25792316641321378, -293.0332903130373552, -344.9421955060753930 ) ) ;
#21232 = CARTESIAN_POINT ( 'NONE',  ( -50.63146142528317029, -296.9843619659567935, -343.1715310827281655 ) ) ;
#21233 = CARTESIAN_POINT ( 'NONE',  ( 21.14407994712002647, -274.9669138486726752, -314.7068509780767727 ) ) ;
#21234 = VERTEX_POINT ( 'NONE', #63710 ) ;
#21235 = CARTESIAN_POINT ( 'NONE',  ( 184.1778392089217107, 3.000000000000000444, -9.000000000000001776 ) ) ;
#21236 = CARTESIAN_POINT ( 'NONE',  ( -100.7308411919326971, -296.7959069380451638, -226.6623200645531142 ) ) ;
#21237 = CARTESIAN_POINT ( 'NONE',  ( 17.08011511308455255, -290.1892874970391745, -321.2261365017562866 ) ) ;
#21238 = CARTESIAN_POINT ( 'NONE',  ( 201.7538767631425003, 295.5538150823438173, -54.00000000004517631 ) ) ;
#21239 = CARTESIAN_POINT ( 'NONE',  ( -23.44333400179391091, -299.3019944946597661, -193.6677463287124681 ) ) ;
#21240 = CARTESIAN_POINT ( 'NONE',  ( 34.38578408321180291, -288.3902805497862687, -284.5347500568023520 ) ) ;
#21241 = ORIENTED_EDGE ( 'NONE', *, *, #43478, .T. ) ;
#21242 = CARTESIAN_POINT ( 'NONE',  ( -45.23721179709964701, -279.0133500514301659, -193.9507026689990710 ) ) ;
#21243 = CARTESIAN_POINT ( 'NONE',  ( 15.41478929567783318, -294.9810067277581425, -326.3081072673980429 ) ) ;
#21244 = CARTESIAN_POINT ( 'NONE',  ( -43.11223418036092170, -287.2638671257919327, -345.9058492181630982 ) ) ;
#21245 = CARTESIAN_POINT ( 'NONE',  ( -81.85601405369061467, -295.9733098157785207, -333.2292469481070611 ) ) ;
#21246 = CARTESIAN_POINT ( 'NONE',  ( 35.22843514771243889, -293.9981606856766234, -278.9088006615419886 ) ) ;
#21247 = CARTESIAN_POINT ( 'NONE',  ( 197.2083993959316786, 68.08024695722009767, -10.51981418967019799 ) ) ;
#21248 = FILL_AREA_STYLE ('',( #35925 ) ) ;
#21249 = DIRECTION ( 'NONE',  ( -1.000000000000000000, 0.000000000000000000, 0.000000000000000000 ) ) ;
#21250 = CARTESIAN_POINT ( 'NONE',  ( -0.07190842257235939561, -288.0588134374509650, -203.7603954838894822 ) ) ;
#21251 = CARTESIAN_POINT ( 'NONE',  ( -99.90806341382575795, -287.4094976428775112, -320.2154176792147382 ) ) ;
#21252 = CARTESIAN_POINT ( 'NONE',  ( -33.91150779519067981, -279.4428342949065041, -193.5395938674784873 ) ) ;
#21253 = CARTESIAN_POINT ( 'NONE',  ( -2.751879263566934242, -284.5939880970526019, -336.7348976013009860 ) ) ;
#21254 = CARTESIAN_POINT ( 'NONE',  ( -113.2322969655488407, -283.2390573494901673, -261.4603537522617671 ) ) ;
#21255 = CARTESIAN_POINT ( 'NONE',  ( -34.54798004935471312, -287.0967566587318629, -344.7992406314769482 ) ) ;
#21256 = CARTESIAN_POINT ( 'NONE',  ( 18.01713818169475800, -278.1295158048703229, -322.0883303720370918 ) ) ;
#21257 = CARTESIAN_POINT ( 'NONE',  ( -46.18554796405813789, -274.2701507500599405, -197.8775071302462720 ) ) ;
#21258 = EDGE_LOOP ( 'NONE', ( #52221, #92460, #86091, #65744 ) ) ;
#21260 = CARTESIAN_POINT ( 'NONE',  ( -46.46096050094721619, -279.2820928344401636, -197.7790429055923198 ) ) ;
#21259 = CARTESIAN_POINT ( 'NONE',  ( -101.8569219400553720, -278.0868628637650772, -304.5193696145124704 ) ) ;
#21261 = CARTESIAN_POINT ( 'NONE',  ( 22.50845317958115643, -275.9866561000245611, -222.3877001586689914 ) ) ;
#21262 = CARTESIAN_POINT ( 'NONE',  ( -112.0112268252158430, -277.5620727571622979, -253.2593489650623724 ) ) ;
#21263 = CARTESIAN_POINT ( 'NONE',  ( -113.6755508159304071, -270.8536776300014708, -283.8132029559086504 ) ) ;
#21264 = CARTESIAN_POINT ( 'NONE',  ( -64.82706478045440690, -274.6430830346805010, -198.6714911177868714 ) ) ;
#21265 = CARTESIAN_POINT ( 'NONE',  ( -91.23291200094298858, -298.7292094129201701, -216.1915363432169102 ) ) ;
#21266 = CARTESIAN_POINT ( 'NONE',  ( -37.37352853689063892, -282.5519495502701943, -195.3611179825600175 ) ) ;
#21267 = ORIENTED_EDGE ( 'NONE', *, *, #54642, .T. ) ;
#21268 = DIRECTION ( 'NONE',  ( 0.000000000000000000, 1.000000000000000000, 0.000000000000000000 ) ) ;
#21269 = CARTESIAN_POINT ( 'NONE',  ( -62.68257507134601525, -286.7942446521547595, -201.5169626913884997 ) ) ;
#21270 = CARTESIAN_POINT ( 'NONE',  ( -68.11124426436150259, -287.4138033428002359, -200.8688085861446950 ) ) ;
#21271 = CARTESIAN_POINT ( 'NONE',  ( -39.97003480951236298, -288.4345010232981963, -343.4654341373205284 ) ) ;
#21272 = CARTESIAN_POINT ( 'NONE',  ( -113.8433405749718474, -283.9573355507500310, -278.5480534333684091 ) ) ;
#21273 = CARTESIAN_POINT ( 'NONE',  ( -14.03713971575828978, -278.7592937563051692, -200.2832497034550272 ) ) ;
#21274 = CARTESIAN_POINT ( 'NONE',  ( -44.16103738394220102, -287.8254229133307263, -196.4397941343143827 ) ) ;
#21275 = CARTESIAN_POINT ( 'NONE',  ( 32.00047629107431391, -280.3629305433468630, -295.4592362771664398 ) ) ;
#21276 = CARTESIAN_POINT ( 'NONE',  ( -13.61041993946012418, -278.0528513790765714, -339.9708546693551625 ) ) ;
#21277 = CARTESIAN_POINT ( 'NONE',  ( 19.04234870993378337, -275.3865622127032680, -223.8979338634113390 ) ) ;
#21278 = CARTESIAN_POINT ( 'NONE',  ( -38.92741896036859117, -287.8665624559097864, -346.9476325643174732 ) ) ;
#21279 = CARTESIAN_POINT ( 'NONE',  ( 26.59321056689514506, -282.9171417432854128, -312.9813715582304212 ) ) ;
#21280 = CARTESIAN_POINT ( 'NONE',  ( -99.29841921454772091, -285.6520062994288196, -224.6566554609867126 ) ) ;
#21281 = CARTESIAN_POINT ( 'NONE',  ( -16.92374966210020304, -280.4899794279351113, -200.2746905999659646 ) ) ;
#21282 = ORIENTED_EDGE ( 'NONE', *, *, #58839, .F. ) ;
#21283 = ORIENTED_EDGE ( 'NONE', *, *, #37042, .T. ) ;
#21284 = CARTESIAN_POINT ( 'NONE',  ( 160.5350683151633291, 275.0000000000000568, 15.22542485937381329 ) ) ;
#21285 = CARTESIAN_POINT ( 'NONE',  ( -64.97409137456668304, -291.2695786855250617, -340.9626785477648241 ) ) ;
#21286 = CARTESIAN_POINT ( 'NONE',  ( -84.87149853817895462, -288.3765489830022375, -330.3805074032717357 ) ) ;
#21287 = CARTESIAN_POINT ( 'NONE',  ( -64.64541401129325493, -272.7454639000781071, -202.3923483293288541 ) ) ;
#21288 = CARTESIAN_POINT ( 'NONE',  ( 6.549008573836617053, -293.8216718229184607, -333.5680453066373730 ) ) ;
#21289 = AXIS2_PLACEMENT_3D ( 'NONE', #70282, #49419, #20549 ) ;
#21290 = CARTESIAN_POINT ( 'NONE',  ( -109.0293439096645756, -288.8088678295441127, -287.4371094214757250 ) ) ;
#21291 = CARTESIAN_POINT ( 'NONE',  ( 13.61685543193546089, -291.0177947290402471, -216.6843108199037147 ) ) ;
#21292 = CARTESIAN_POINT ( 'NONE',  ( 33.46905300474775657, -289.0132223566969856, -289.8622422578415581 ) ) ;
#21293 = CARTESIAN_POINT ( 'NONE',  ( -114.2704648735229114, -287.0519495502703080, -270.3937649182068981 ) ) ;
#21294 = CARTESIAN_POINT ( 'NONE',  ( 18.16176755763629203, -290.2562433903181613, -320.8219611049982518 ) ) ;
#21295 = CARTESIAN_POINT ( 'NONE',  ( -111.3332659755394900, -288.3814470593611077, -283.6731627468009833 ) ) ;
#21296 = CIRCLE ( 'NONE', #15206, 4.025000000000000355 ) ;
#21297 = CARTESIAN_POINT ( 'NONE',  ( -23.52876731164776203, -294.2287434121942624, -196.5919547122190920 ) ) ;
#21298 = CARTESIAN_POINT ( 'NONE',  ( -105.4282743961954196, -285.1320848982025495, -297.4736639907682729 ) ) ;
#21299 = CARTESIAN_POINT ( 'NONE',  ( -39.19270091967422331, -294.0291617513930191, -195.2045166616555321 ) ) ;
#21300 = CARTESIAN_POINT ( 'NONE',  ( 200.2296996224750103, 66.43830042153604154, -2.389358538587389003 ) ) ;
#21301 = CARTESIAN_POINT ( 'NONE',  ( 153.4750402936816727, 20.31599870471568536, -12.32002737771801115 ) ) ;
#21302 = CARTESIAN_POINT ( 'NONE',  ( -102.8132364824645748, -275.0283573855661530, -232.9483691663406546 ) ) ;
#21303 = CARTESIAN_POINT ( 'NONE',  ( 12.01811760469106005, -281.5416795939549957, -324.3630635026745495 ) ) ;
#21304 = CARTESIAN_POINT ( 'NONE',  ( -93.17039472124659483, -281.8542081279704803, -320.4619591663890787 ) ) ;
#21305 = CARTESIAN_POINT ( 'NONE',  ( -97.28789784910350136, -295.1037172037462142, -318.4507722160524281 ) ) ;
#21306 = CARTESIAN_POINT ( 'NONE',  ( 28.77644220285192134, -273.3467712171160997, -237.0990485095763631 ) ) ;
#21307 = CARTESIAN_POINT ( 'NONE',  ( -109.8951831907875487, -276.4158429125819225, -287.0702036927465883 ) ) ;
#21308 = CARTESIAN_POINT ( 'NONE',  ( -52.75474825975436488, -299.1658246299951429, -198.4501195967229989 ) ) ;
#21309 = CARTESIAN_POINT ( 'NONE',  ( -0.4469370417777366322, -295.9770761929294736, -334.0915021885120382 ) ) ;
#21310 = EDGE_CURVE ( 'NONE', #14641, #24267, #85453, .T. ) ;
#21311 = DIRECTION ( 'NONE',  ( 0.000000000000000000, 0.000000000000000000, 1.000000000000000000 ) ) ;
#21312 = CARTESIAN_POINT ( 'NONE',  ( 6.167159403133554818, -295.2476099321969514, -329.2424614016791224 ) ) ;
#21313 = CARTESIAN_POINT ( 'NONE',  ( 113.5000000000000568, -211.8141737103562434, -420.2472828204663529 ) ) ;
#21315 = CARTESIAN_POINT ( 'NONE',  ( -93.08239456204718465, -295.8820380417219553, -317.5183125269336415 ) ) ;
#21314 = CARTESIAN_POINT ( 'NONE',  ( 27.30083539783106161, -285.0550641877488260, -231.5338303023210926 ) ) ;
#21316 = CARTESIAN_POINT ( 'NONE',  ( -78.52246274269717219, -285.5139667304173940, -205.2984959136742589 ) ) ;
#21317 = CARTESIAN_POINT ( 'NONE',  ( 37.80337648723936894, -287.4285663488244040, -287.1234291388756219 ) ) ;
#21318 = CARTESIAN_POINT ( 'NONE',  ( -92.46862867832687982, -297.8161907965251203, -321.7554842977831413 ) ) ;
#21319 = CARTESIAN_POINT ( 'NONE',  ( -19.61375188303495065, -290.2803447588852919, -197.6043799376736558 ) ) ;
#21320 = CARTESIAN_POINT ( 'NONE',  ( -72.42394825665984115, -278.7970112352028877, -201.9842667297878620 ) ) ;
#21321 = CARTESIAN_POINT ( 'NONE',  ( -110.4542110544635705, -294.2666405000204577, -253.6410175316879361 ) ) ;
#21322 = FACE_OUTER_BOUND ( 'NONE', #40387, .T. ) ;
#21323 = CARTESIAN_POINT ( 'NONE',  ( -25.06035422671212487, -285.0070351367819512, -197.9472632055166343 ) ) ;
#21324 = FACE_OUTER_BOUND ( 'NONE', #91996, .T. ) ;
#21325 = CARTESIAN_POINT ( 'NONE',  ( -76.94589455299046676, -287.5825399559333846, -334.0518428317784583 ) ) ;
#21326 = CARTESIAN_POINT ( 'NONE',  ( -106.5632221731606819, -298.4915293816200688, -244.6241271892120608 ) ) ;
#21327 = CARTESIAN_POINT ( 'NONE',  ( 23.26874848992852662, -282.3517029414020953, -223.8104058276473154 ) ) ;
#21329 = CARTESIAN_POINT ( 'NONE',  ( 35.42901951167450392, -281.6364471782130181, -276.7511404148033307 ) ) ;
#21328 = CARTESIAN_POINT ( 'NONE',  ( -112.1390381335946813, -294.6892204006201723, -261.2087942729142469 ) ) ;
#21330 = CARTESIAN_POINT ( 'NONE',  ( -112.6009524058867868, -296.9231587029738648, -254.0193672505807854 ) ) ;
#21331 = CARTESIAN_POINT ( 'NONE',  ( -95.08627725284839016, -274.6159676476437426, -224.7438106114496179 ) ) ;
#21332 = CARTESIAN_POINT ( 'NONE',  ( 0.8159999791476266751, -284.6367183790358126, -205.1287033498456083 ) ) ;
#21333 = EDGE_CURVE ( 'NONE', #41136, #13227, #24515, .T. ) ;
#21334 = CARTESIAN_POINT ( 'NONE',  ( -35.41365353264124138, -282.0764801100624481, -195.3731042840245777 ) ) ;
#21335 = CARTESIAN_POINT ( 'NONE',  ( -69.34958648091600253, -296.6790175942991823, -204.4907630406402461 ) ) ;
#21336 = ORIENTED_EDGE ( 'NONE', *, *, #74127, .T. ) ;
#21337 = CARTESIAN_POINT ( 'NONE',  ( 83.14890176555634582, -297.1582149144751384, -195.3611179825600175 ) ) ;
#21338 = CARTESIAN_POINT ( 'NONE',  ( -85.91338271712612595, -285.7089061417845528, -327.0412595688014790 ) ) ;
#21339 = LINE ( 'NONE', #36015, #2055 ) ;
#21340 = CARTESIAN_POINT ( 'NONE',  ( -85.28047601435909542, -288.9094976428777386, -210.1954327657594206 ) ) ;
#21341 = CARTESIAN_POINT ( 'NONE',  ( 23.38413236604104384, -275.3795324871163643, -317.4625141535940429 ) ) ;
#21342 = CARTESIAN_POINT ( 'NONE',  ( 20.99508032478530950, -292.7692238509437175, -226.4769516930897169 ) ) ;
#21343 = CARTESIAN_POINT ( 'NONE',  ( 21.87466388457362854, -282.4627592899136062, -226.4749804589744429 ) ) ;
#21344 = CARTESIAN_POINT ( 'NONE',  ( 26.07329512816975736, -277.6656207090827593, -308.1100092324665525 ) ) ;
#21345 = CARTESIAN_POINT ( 'NONE',  ( 25.28458159991488685, -283.7319798563980839, -313.7936272354587004 ) ) ;
#21346 = CARTESIAN_POINT ( 'NONE',  ( 22.44580575025058877, -279.7555805469957591, -227.7866579592388803 ) ) ;
#21347 = CARTESIAN_POINT ( 'NONE',  ( -84.23801284099724285, -279.6968515522974599, -328.9577323644639364 ) ) ;
#21348 = CARTESIAN_POINT ( 'NONE',  ( -99.56830686352940063, -273.3217635584348386, -224.9202005216477858 ) ) ;
#21349 = CARTESIAN_POINT ( 'NONE',  ( -2.727012337184489432, -276.4405986332532734, -339.1567771311206911 ) ) ;
#21350 = CARTESIAN_POINT ( 'NONE',  ( 6.938773765591287557, -296.3647515999579127, -330.2631006016060837 ) ) ;
#21351 = CARTESIAN_POINT ( 'NONE',  ( 199.4757856505700886, 63.23505538068435783, -9.191047964625935762 ) ) ;
#21352 = DIRECTION ( 'NONE',  ( 0.000000000000000000, 0.000000000000000000, 1.000000000000000000 ) ) ;
#21353 = CARTESIAN_POINT ( 'NONE',  ( 8.145370589423139407, -292.5770245399876899, -330.9518093089620265 ) ) ;
#21354 = CARTESIAN_POINT ( 'NONE',  ( -35.38239740990338333, -273.5850209208139745, -197.3133396504947257 ) ) ;
#21355 = AXIS2_PLACEMENT_3D ( 'NONE', #30423, #15292, #79245 ) ;
#21356 = CARTESIAN_POINT ( 'NONE',  ( 31.61187946678717253, -295.4962844463024680, -303.1663340991964333 ) ) ;
#21357 = CARTESIAN_POINT ( 'NONE',  ( 24.48485388998581769, -294.1536275444740340, -225.1340692437146629 ) ) ;
#21359 = VECTOR ( 'NONE', #21011, 1000.000000000000000 ) ;
#21358 = CARTESIAN_POINT ( 'NONE',  ( 15.39294038702397494, -290.3048975160289729, -323.4561847501590819 ) ) ;
#21360 = CARTESIAN_POINT ( 'NONE',  ( -112.1838994929950530, -276.5846707936894973, -267.8212503199704315 ) ) ;
#21361 = CARTESIAN_POINT ( 'NONE',  ( -41.92121508043608458, -279.0304350080685367, -344.6729685723889816 ) ) ;
#21362 = CARTESIAN_POINT ( 'NONE',  ( 35.05384187436523291, -291.4071984988084978, -252.9803134857809823 ) ) ;
#21363 = CARTESIAN_POINT ( 'NONE',  ( 19.19098021615143068, -282.7173128192280842, -219.8999530194980139 ) ) ;
#21364 = CARTESIAN_POINT ( 'NONE',  ( -105.8489335441694976, -283.8194352437740804, -244.2654278646709542 ) ) ;
#21365 = ORIENTED_EDGE ( 'NONE', *, *, #29965, .F. ) ;
#21366 = CARTESIAN_POINT ( 'NONE',  ( -21.38772728848908500, -282.5087210543082961, -341.6701325559633915 ) ) ;
#21367 = CARTESIAN_POINT ( 'NONE',  ( -72.37790729830854275, -280.6792107811446044, -202.1266101619298468 ) ) ;
#21368 = CARTESIAN_POINT ( 'NONE',  ( -101.0972352662010252, -282.7842157071579550, -312.9209014827710575 ) ) ;
#21369 = CARTESIAN_POINT ( 'NONE',  ( -105.9706143199053940, -279.9384947163266020, -235.8494913762532406 ) ) ;
#21370 = CARTESIAN_POINT ( 'NONE',  ( -86.63244065416141382, -279.2425828732394280, -328.6808230668561350 ) ) ;
#21371 = CARTESIAN_POINT ( 'NONE',  ( 27.33386217378599881, -295.6233781216987495, -239.1787733560258573 ) ) ;
#21372 = VERTEX_POINT ( 'NONE', #91604 ) ;
#21373 = EDGE_LOOP ( 'NONE', ( #41245, #41609, #90007, #91075 ) ) ;
#21374 = CARTESIAN_POINT ( 'NONE',  ( -58.49254416103472920, -299.7788533544078859, -198.4052812288414316 ) ) ;
#21375 = CARTESIAN_POINT ( 'NONE',  ( -104.8467963803897050, -276.9946683709684976, -238.3820821732341244 ) ) ;
#21376 = CARTESIAN_POINT ( 'NONE',  ( -85.88315453333730431, -293.1509498526403945, -211.8316718680007966 ) ) ;
#21377 = CARTESIAN_POINT ( 'NONE',  ( -3.103347651892360393, -293.9357373727264644, -334.9492584431066007 ) ) ;
#21378 = CARTESIAN_POINT ( 'NONE',  ( -98.11485749106958565, -289.4292078704581854, -317.5432146682532561 ) ) ;
#21379 = CARTESIAN_POINT ( 'NONE',  ( 2.197429475817664013, -229.5268262511776527, 21.50000000000000000 ) ) ;
#21381 = CARTESIAN_POINT ( 'NONE',  ( -90.22201717344397309, -283.6891000058087116, -218.8085621058053505 ) ) ;
#21380 = CARTESIAN_POINT ( 'NONE',  ( -4.770303547612166462, -293.2062836189126074, -339.4964591033963757 ) ) ;
#21382 = CARTESIAN_POINT ( 'NONE',  ( -3.087005893952967206, -294.3701665050123211, -204.5015597877963671 ) ) ;
#21383 = CARTESIAN_POINT ( 'NONE',  ( 16.49407922800606840, -285.3147434412307462, -220.0193685667901491 ) ) ;
#21384 = CARTESIAN_POINT ( 'NONE',  ( 33.80511217668076540, -283.1094891608026387, -288.8334127336015626 ) ) ;
#21385 = CARTESIAN_POINT ( 'NONE',  ( -65.34996963061553288, -290.3505630567544813, -341.8900559315690657 ) ) ;
#21386 = CARTESIAN_POINT ( 'NONE',  ( -11.72744321366486275, -280.8870908776754050, -201.8832194128696074 ) ) ;
#21387 = CARTESIAN_POINT ( 'NONE',  ( 39.31428347453377370, -292.3466305283561155, -270.3255398957106195 ) ) ;
#21388 = CARTESIAN_POINT ( 'NONE',  ( 21.37225936225295442, -289.0241304790955610, -319.9275358679049077 ) ) ;
#21389 = CARTESIAN_POINT ( 'NONE',  ( -106.4554723598231334, -290.6086741439372645, -304.2877217913605818 ) ) ;
#21390 = CARTESIAN_POINT ( 'NONE',  ( -100.9923601050083590, -285.2091427361062301, -234.5140787532585023 ) ) ;
#21391 = ORIENTED_EDGE ( 'NONE', *, *, #11577, .F. ) ;
#21392 = CARTESIAN_POINT ( 'NONE',  ( 31.12414629204448602, -295.8365236657332389, -302.9293497766255427 ) ) ;
#21393 = CARTESIAN_POINT ( 'NONE',  ( -113.8159819983055598, -295.2825359508860856, -266.7417986598027255 ) ) ;
#21394 = CARTESIAN_POINT ( 'NONE',  ( -95.46705930252035444, -276.9861388340378880, -314.9127853999037256 ) ) ;
#21395 = CARTESIAN_POINT ( 'NONE',  ( -113.0066083995344997, -272.2378554502179213, -256.1359044117549502 ) ) ;
#21396 = CARTESIAN_POINT ( 'NONE',  ( -6.492130255045490017, -293.1193271474610356, -337.2865376154775845 ) ) ;
#21397 = CARTESIAN_POINT ( 'NONE',  ( 36.38553290198070300, -277.2204548159018600, -263.3021088964512160 ) ) ;
#21398 = CARTESIAN_POINT ( 'NONE',  ( -92.01650251236651457, -271.4006516052635902, -220.1274546884554013 ) ) ;
#21399 = CARTESIAN_POINT ( 'NONE',  ( 24.77142996404363018, -295.2955861353386240, -309.5601941021214429 ) ) ;
#21400 = CARTESIAN_POINT ( 'NONE',  ( -67.40947196203978820, -296.5357082085511138, -337.2340997557380433 ) ) ;
#21401 = CARTESIAN_POINT ( 'NONE',  ( 175.2296996224750103, 275.5000000000000568, 0.000000000000000000 ) ) ;
#21402 = CARTESIAN_POINT ( 'NONE',  ( -88.34516788969136769, -295.3398691568279446, -215.0758281356166322 ) ) ;
#21403 = CARTESIAN_POINT ( 'NONE',  ( -30.50418177803270936, -298.7870618871939996, -193.4623166349295502 ) ) ;
#21404 = CARTESIAN_POINT ( 'NONE',  ( 27.54148833797076890, -286.5976912020086615, -305.1905063281713524 ) ) ;
#21405 = CARTESIAN_POINT ( 'NONE',  ( 195.5881128153457098, -27.00396092263537540, 22.50000000000000000 ) ) ;
#21406 = CARTESIAN_POINT ( 'NONE',  ( -107.9494543833702807, -291.2351393495428056, -289.9889099853360790 ) ) ;
#21407 = CARTESIAN_POINT ( 'NONE',  ( -95.98485595537673021, -273.7166013571282406, -220.5361407569864696 ) ) ;
#21408 = CARTESIAN_POINT ( 'NONE',  ( -110.3955101695432433, -296.9068586695804584, -268.7366596028214758 ) ) ;
#21409 = CARTESIAN_POINT ( 'NONE',  ( -112.7387722004195609, -280.5161268319159831, -271.6069157584847744 ) ) ;
#21410 = CARTESIAN_POINT ( 'NONE',  ( 14.83732007160970845, -279.4536524782851075, -214.3364869631018053 ) ) ;
#21411 = ORIENTED_EDGE ( 'NONE', *, *, #60434, .T. ) ;
#21412 = CARTESIAN_POINT ( 'NONE',  ( -31.65211809747334826, -282.3307269029556892, -347.0616648443773897 ) ) ;
#21413 = CARTESIAN_POINT ( 'NONE',  ( 38.39316699270343491, -274.7329365952886633, -256.9613168756970936 ) ) ;
#21414 = CARTESIAN_POINT ( 'NONE',  ( 37.35723688023576727, -280.1422294028776605, -285.4113414819611307 ) ) ;
#21415 = CARTESIAN_POINT ( 'NONE',  ( -14.75381922397232870, -278.3438646986959384, -198.6140320828808683 ) ) ;
#21416 = ADVANCED_FACE ( 'NONE', ( #84037 ), #63240, .T. ) ;
#21417 = CARTESIAN_POINT ( 'NONE',  ( -70.67636136704722105, -296.2878382342544796, -204.8486874361631749 ) ) ;
#21418 = CARTESIAN_POINT ( 'NONE',  ( -32.17872436761616939, -276.1174149492999845, -195.5262770011973714 ) ) ;
#21419 = DIRECTION ( 'NONE',  ( 0.000000000000000000, 0.000000000000000000, 1.000000000000000000 ) ) ;
#21420 = CARTESIAN_POINT ( 'NONE',  ( -34.98601919685224004, -290.1016805967838081, -195.0298743235898371 ) ) ;
#21421 = AXIS2_PLACEMENT_3D ( 'NONE', #50587, #6104, #7042 ) ;
#21422 = CARTESIAN_POINT ( 'NONE',  ( -99.20459208274296259, -291.1618868005963350, -224.4916465671718129 ) ) ;
#21423 = CARTESIAN_POINT ( 'NONE',  ( -54.92994582530294423, -275.8266867040787247, -197.2811478351008248 ) ) ;
#21424 = CARTESIAN_POINT ( 'NONE',  ( -99.48648187488048222, -271.1211597239678213, -228.2800997367835407 ) ) ;
#21425 = CARTESIAN_POINT ( 'NONE',  ( -103.8954707845855125, -284.2508101692046694, -231.8528003569259681 ) ) ;
#21426 = CARTESIAN_POINT ( 'NONE',  ( 209.7912073884560300, 37.96760760058285200, 13.96055292456829378 ) ) ;
#21427 = TOROIDAL_SURFACE ( 'NONE', #12362, 1.500000000000000888, 0.5000000000000000000 ) ;
#21428 = CARTESIAN_POINT ( 'NONE',  ( -111.6166571419884406, -282.4138117147431899, -281.1228031932268436 ) ) ;
#21429 = DIRECTION ( 'NONE',  ( -1.000000000000000000, 0.000000000000000000, 0.000000000000000000 ) ) ;
#21430 = CARTESIAN_POINT ( 'NONE',  ( 33.69636507485748211, -292.1046990867142199, -251.9024127719551984 ) ) ;
#21431 = CARTESIAN_POINT ( 'NONE',  ( -30.39245392472972185, -284.2804099009798051, -196.4002347469137248 ) ) ;
#21432 = CARTESIAN_POINT ( 'NONE',  ( 195.2901672131851285, 26.10222097264500363, 14.91929003175754964 ) ) ;
#21433 = DIRECTION ( 'NONE',  ( 0.000000000000000000, 0.000000000000000000, -1.000000000000000000 ) ) ;
#21434 = CARTESIAN_POINT ( 'NONE',  ( 21.24041447881314681, -292.1961249494211188, -317.2125168805756630 ) ) ;
#21435 = CARTESIAN_POINT ( 'NONE',  ( -113.5175605608882989, -282.9652824982334209, -275.6502607883592191 ) ) ;
#21436 = CARTESIAN_POINT ( 'NONE',  ( -59.99839998567912147, -281.3538685891093678, -200.0710908577658529 ) ) ;
#21437 = CARTESIAN_POINT ( 'NONE',  ( -109.6077781263779514, -286.0794158120244788, -244.9520115678777756 ) ) ;
#21438 = CARTESIAN_POINT ( 'NONE',  ( -2.830081744852734005, -278.7417935764178196, -202.6492986790875932 ) ) ;
#21439 = CARTESIAN_POINT ( 'NONE',  ( 34.56739659606086690, -287.3825311905106332, -257.5029209381216901 ) ) ;
#21440 = CARTESIAN_POINT ( 'NONE',  ( -54.07037762220355859, -278.6963128482075831, -342.0762630842294811 ) ) ;
#21441 = CARTESIAN_POINT ( 'NONE',  ( -110.4410605348046772, -279.3153154961788687, -273.3752902739163346 ) ) ;
#21442 = ADVANCED_FACE ( 'NONE', ( #61808 ), #91056, .F. ) ;
#21443 = CARTESIAN_POINT ( 'NONE',  ( -8.007199267271198906, -288.4142652374155205, -200.8946324920737538 ) ) ;
#21444 = ORIENTED_EDGE ( 'NONE', *, *, #67159, .T. ) ;
#21445 = CARTESIAN_POINT ( 'NONE',  ( -20.50779345604741621, -298.0907843225825786, -193.3615769139673546 ) ) ;
#21446 = CARTESIAN_POINT ( 'NONE',  ( 35.90289766715125808, -289.7185447161817251, -284.8174295038053856 ) ) ;
#21447 = CARTESIAN_POINT ( 'NONE',  ( 180.6899167944524436, -12.49482340714361506, 10.00000000000000000 ) ) ;
#21448 = CARTESIAN_POINT ( 'NONE',  ( -115.3288506153726871, -280.8376638359844151, -288.1938231032136741 ) ) ;
#21449 = ORIENTED_EDGE ( 'NONE', *, *, #40622, .F. ) ;
#21450 = CARTESIAN_POINT ( 'NONE',  ( -66.79327125728174508, -271.6670034999890504, -201.2045319864713235 ) ) ;
#21451 = CARTESIAN_POINT ( 'NONE',  ( 36.98554331911887516, -291.7391773340946770, -253.5126277257724894 ) ) ;
#21452 = CARTESIAN_POINT ( 'NONE',  ( -41.38009691863028650, -287.5205441174657039, -196.7659005114314823 ) ) ;
#21453 = CARTESIAN_POINT ( 'NONE',  ( 27.33360214868353566, -282.8269776044406285, -234.3739079380453347 ) ) ;
#21454 = CARTESIAN_POINT ( 'NONE',  ( 37.44304227898425097, -288.7790141760688698, -254.6182756471966968 ) ) ;
#21455 = CARTESIAN_POINT ( 'NONE',  ( 31.25274891271851629, -289.3068945009376876, -304.3642733043050725 ) ) ;
#21456 = CARTESIAN_POINT ( 'NONE',  ( -112.3915647492318328, -286.5447593930720700, -270.9497396867755583 ) ) ;
#21457 = CARTESIAN_POINT ( 'NONE',  ( -108.6556342216229467, -278.3500133887044399, -299.4011387916142439 ) ) ;
#21458 = EDGE_LOOP ( 'NONE', ( #83410, #80515, #49232, #24152 ) ) ;
#21459 = CARTESIAN_POINT ( 'NONE',  ( -33.53235727059151827, -293.0844331167886594, -345.8379114322244732 ) ) ;
#21460 = CARTESIAN_POINT ( 'NONE',  ( -11.50735574411731399, -280.2127311159050578, -197.7683400477946520 ) ) ;
#21461 = CARTESIAN_POINT ( 'NONE',  ( -111.5777819524823684, -274.4482009412615753, -267.6148025881067269 ) ) ;
#21462 = CARTESIAN_POINT ( 'NONE',  ( -4.771743288812468897, -285.1233781216987495, -337.9199732462171255 ) ) ;
#21463 = CARTESIAN_POINT ( 'NONE',  ( -91.43179795749590255, -271.5349147600256856, -216.9922569333990623 ) ) ;
#21464 = FACE_OUTER_BOUND ( 'NONE', #2720, .T. ) ;
#21465 = CARTESIAN_POINT ( 'NONE',  ( -62.32410252672553241, -279.2260164632038482, -201.6501033849325495 ) ) ;
#21466 = CARTESIAN_POINT ( 'NONE',  ( 38.52877522146756917, -276.6243737987749682, -259.7932568615818241 ) ) ;
#21467 = CARTESIAN_POINT ( 'NONE',  ( -33.79447898179370924, -299.5226837574093111, -196.7710040749456653 ) ) ;
#21468 = CARTESIAN_POINT ( 'NONE',  ( -113.3680671762393075, -283.4729469363727503, -281.3582739984130399 ) ) ;
#21469 = CARTESIAN_POINT ( 'NONE',  ( -100.5890149847064237, -292.8344549044419409, -231.9195886729019662 ) ) ;
#21470 = CARTESIAN_POINT ( 'NONE',  ( -43.99344572504309525, -275.5696530276545673, -194.3992417064939673 ) ) ;
#21471 = CARTESIAN_POINT ( 'NONE',  ( 30.33659482775287586, -300.0868488860655816, -193.7446608145621951 ) ) ;
#21472 = CARTESIAN_POINT ( 'NONE',  ( -17.71576201847185317, -296.7985928871418082, -342.5750430728895708 ) ) ;
#21473 = CARTESIAN_POINT ( 'NONE',  ( -5.269760757205497193, -280.6290538853249359, -337.9874824674561751 ) ) ;
#21474 = CARTESIAN_POINT ( 'NONE',  ( -67.00337498109597334, -291.3405669656972918, -199.3264128274505538 ) ) ;
#21475 = CARTESIAN_POINT ( 'NONE',  ( -46.35289299348226422, -271.9573501466052790, -196.2622299715482654 ) ) ;
#21476 = CARTESIAN_POINT ( 'NONE',  ( -46.43050066141889687, -287.5387672241343466, -194.7050929796331786 ) ) ;
#21477 = CARTESIAN_POINT ( 'NONE',  ( -84.01530829273427514, -290.3132741877302578, -213.8297074788579550 ) ) ;
#21478 = ORIENTED_EDGE ( 'NONE', *, *, #26156, .F. ) ;
#21479 = CARTESIAN_POINT ( 'NONE',  ( -95.02550210999098113, -288.4443523301134178, -320.4728459797386790 ) ) ;
#21480 = CARTESIAN_POINT ( 'NONE',  ( -90.77176297467201493, -290.9345193009630748, -220.5699900472900481 ) ) ;
#21481 = EDGE_LOOP ( 'NONE', ( #73742, #54532, #408, #40993 ) ) ;
#21482 = CARTESIAN_POINT ( 'NONE',  ( -57.68721897056022385, -286.8752286527841306, -196.3630864068943254 ) ) ;
#21483 = CARTESIAN_POINT ( 'NONE',  ( -68.04244926072802002, -277.7999790617918734, -336.6285594747408254 ) ) ;
#21484 = CARTESIAN_POINT ( 'NONE',  ( 34.17955452696386942, -292.1187557242975004, -242.5339279771212091 ) ) ;
#21485 = CARTESIAN_POINT ( 'NONE',  ( -97.08794490109738717, -284.5531681626406453, -318.7935735132654713 ) ) ;
#21486 = CARTESIAN_POINT ( 'NONE',  ( -112.3400891012334171, -285.1024653158666524, -253.0121715273484426 ) ) ;
#21487 = CARTESIAN_POINT ( 'NONE',  ( -49.14950696976872280, -280.2308000225204978, -198.3009820939238921 ) ) ;
#21488 = CARTESIAN_POINT ( 'NONE',  ( 185.6829310669746462, 263.5356091243360765, -153.4021477105963243 ) ) ;
#21489 = AXIS2_PLACEMENT_3D ( 'NONE', #50509, #35380, #57171 ) ;
#21490 = CARTESIAN_POINT ( 'NONE',  ( 63.70159209483512797, 48.22975029174962458, -318.1369363225185793 ) ) ;
#21491 = CARTESIAN_POINT ( 'NONE',  ( -56.80084188927647659, -168.8182197709074046, -361.0463781639207923 ) ) ;
#21492 = AXIS2_PLACEMENT_3D ( 'NONE', #76742, #26069, #4766 ) ;
#21493 = CARTESIAN_POINT ( 'NONE',  ( -90.30646721055705939, -272.4757563819280790, -219.8716600230470419 ) ) ;
#21494 = CARTESIAN_POINT ( 'NONE',  ( -34.01294384033642615, -273.0153285925379691, -197.1276184363042603 ) ) ;
#21495 = CARTESIAN_POINT ( 'NONE',  ( -101.5803473206244973, -295.5015107232558194, -312.8004037482381818 ) ) ;
#21496 = CARTESIAN_POINT ( 'NONE',  ( -101.3485003382535723, -255.0465241227205979, -324.4801213465552792 ) ) ;
#21497 = CARTESIAN_POINT ( 'NONE',  ( -7.864996635055389262, -273.1150887667228062, -199.7044361416253082 ) ) ;
#21498 = CARTESIAN_POINT ( 'NONE',  ( -69.81895627968575013, -299.4802318397225349, -203.6071419447495430 ) ) ;
#21499 = CARTESIAN_POINT ( 'NONE',  ( 32.78922225733731466, -289.1586181643885993, -292.5055419561649614 ) ) ;
#21500 = ORIENTED_EDGE ( 'NONE', *, *, #50606, .F. ) ;
#21501 = CARTESIAN_POINT ( 'NONE',  ( -97.17052517212012219, -298.1399411993618287, -222.2640088382701151 ) ) ;
#21502 = AXIS2_PLACEMENT_3D ( 'NONE', #77215, #33184, #41680 ) ;
#21503 = CARTESIAN_POINT ( 'NONE',  ( 24.99996933245994057, -287.5200207195633766, -232.2625000227118335 ) ) ;
#21504 = CARTESIAN_POINT ( 'NONE',  ( -78.66338643976456524, -272.4297658651656207, -205.7545335686023122 ) ) ;
#21505 = CARTESIAN_POINT ( 'NONE',  ( 22.16807974827314709, -295.0090052377701113, -318.9898516642721802 ) ) ;
#21506 = CARTESIAN_POINT ( 'NONE',  ( -37.68240824331939365, -295.5486197407395821, -347.3118934514236571 ) ) ;
#21507 = CARTESIAN_POINT ( 'NONE',  ( 33.77590485901108508, -293.9367662397261824, -286.8869646159539002 ) ) ;
#21508 = EDGE_LOOP ( 'NONE', ( #30650, #10628, #37549, #77600 ) ) ;
#21509 = CARTESIAN_POINT ( 'NONE',  ( -68.27729901727558115, -275.5691788448407920, -201.4100406849607339 ) ) ;
#21510 = EDGE_CURVE ( 'NONE', #68845, #36747, #56113, .T. ) ;
#21511 = ORIENTED_EDGE ( 'NONE', *, *, #12254, .F. ) ;
#21512 = CARTESIAN_POINT ( 'NONE',  ( -112.4257248369146254, -277.8496532722548409, -287.1514764392074426 ) ) ;
#21513 = CARTESIAN_POINT ( 'NONE',  ( 35.41777855516782125, -273.7899004003899677, -257.9369021103371438 ) ) ;
#21514 = CARTESIAN_POINT ( 'NONE',  ( -37.16397723159514044, -299.2595114767989912, -196.9611406590407512 ) ) ;
#21515 = CARTESIAN_POINT ( 'NONE',  ( 34.12550975376370133, -276.7044817918813351, -286.4133811976718675 ) ) ;
#21516 = CARTESIAN_POINT ( 'NONE',  ( -64.55834345259904694, -275.4618401520278326, -199.4018682670943576 ) ) ;
#21517 = CARTESIAN_POINT ( 'NONE',  ( -17.80906853067696360, -274.8215773215832201, -343.1408067894699343 ) ) ;
#21518 = CARTESIAN_POINT ( 'NONE',  ( -106.9638098869072138, -296.9064867921208020, -292.8106757444147092 ) ) ;
#21519 = CARTESIAN_POINT ( 'NONE',  ( 8.581832049218400371, -292.9838561365360761, -327.9279346713149721 ) ) ;
#21520 = FACE_OUTER_BOUND ( 'NONE', #59218, .T. ) ;
#21521 = CARTESIAN_POINT ( 'NONE',  ( -109.5506113879550014, -279.3821693467757541, -243.6479029370459841 ) ) ;
#21522 = CARTESIAN_POINT ( 'NONE',  ( -37.80762893467147734, -277.2247927442888340, -343.3720839985188036 ) ) ;
#21523 = CARTESIAN_POINT ( 'NONE',  ( 38.30054579420336580, -286.0915161927486565, -258.8042906515589721 ) ) ;
#21524 = CARTESIAN_POINT ( 'NONE',  ( -85.20778782822631570, -297.7116797421144270, -328.3168430817167973 ) ) ;
#21525 = CARTESIAN_POINT ( 'NONE',  ( 82.65856464842170226, -298.7952694379614513, -197.7495342522536816 ) ) ;
#21526 = CARTESIAN_POINT ( 'NONE',  ( 17.94084266078888490, -287.4314508133875279, -318.3581640327193440 ) ) ;
#21527 = CARTESIAN_POINT ( 'NONE',  ( -93.51008306804587278, -276.1152376563603070, -318.5595284676081178 ) ) ;
#21528 = CARTESIAN_POINT ( 'NONE',  ( -110.7451143679794399, -277.1952637989844561, -265.1348675249990947 ) ) ;
#21529 = CARTESIAN_POINT ( 'NONE',  ( -78.37709724978498116, -285.6040486583280540, -333.2005340795712982 ) ) ;
#21530 = CARTESIAN_POINT ( 'NONE',  ( -91.24911084563214558, -279.0449886155982426, -320.2458855676034091 ) ) ;
#21531 = CARTESIAN_POINT ( 'NONE',  ( 175.2296996224750103, 133.0000000000000000, 0.000000000000000000 ) ) ;
#21532 = CARTESIAN_POINT ( 'NONE',  ( 38.13461029507453759, -273.8196222189280320, -259.8841441783870323 ) ) ;
#21533 = CARTESIAN_POINT ( 'NONE',  ( 33.93128985157731137, -275.9888409818506716, -254.0554553733323075 ) ) ;
#21534 = CARTESIAN_POINT ( 'NONE',  ( 15.90596991672398097, -282.8041539367392829, -217.2342810461550187 ) ) ;
#21535 = CARTESIAN_POINT ( 'NONE',  ( 202.9738562182569694, 293.9636489450776367, 3.999999999999991562 ) ) ;
#21536 = CARTESIAN_POINT ( 'NONE',  ( -18.06760574957008103, -290.7257349571830787, -343.4215277896019529 ) ) ;
#21537 = CARTESIAN_POINT ( 'NONE',  ( 35.80217473764341918, -291.3383509234745929, -253.7219851101134509 ) ) ;
#21538 = DIRECTION ( 'NONE',  ( -0.000000000000000000, -1.000000000000000000, -0.000000000000000000 ) ) ;
#21539 = CARTESIAN_POINT ( 'NONE',  ( -90.54211130835216181, -271.9634975908120964, -219.6380786202479953 ) ) ;
#21540 = CARTESIAN_POINT ( 'NONE',  ( 23.61552052922447942, -291.1108102924919763, -227.9702939864256450 ) ) ;
#21541 = CARTESIAN_POINT ( 'NONE',  ( 206.6943913402143096, 294.1769577359763161, -83.83314285352493300 ) ) ;
#21542 = CARTESIAN_POINT ( 'NONE',  ( 0.000000000000000000, -147.7221692137691775, 0.000000000000000000 ) ) ;
#21543 = CARTESIAN_POINT ( 'NONE',  ( -100.1212885157644052, -288.4540303298966819, -313.7365837998821689 ) ) ;
#21544 = CARTESIAN_POINT ( 'NONE',  ( -83.27691636625509375, -285.2933055698237013, -328.1882256796054094 ) ) ;
#21545 = CARTESIAN_POINT ( 'NONE',  ( -35.15464261151896608, -284.3190904410691928, -194.3929583529316290 ) ) ;
#21546 = CARTESIAN_POINT ( 'NONE',  ( -36.16605991260344410, -284.4624008067302725, -343.9409575375638610 ) ) ;
#21547 = CARTESIAN_POINT ( 'NONE',  ( -109.5822001631679967, -285.5083508857517813, -258.7096648739631632 ) ) ;
#21548 = CARTESIAN_POINT ( 'NONE',  ( -112.0392307135613095, -292.6638894053500053, -260.0440852111001391 ) ) ;
#21549 = VECTOR ( 'NONE', #57524, 1000.000000000000000 ) ;
#21550 = CARTESIAN_POINT ( 'NONE',  ( 13.94722594299829410, -275.0816345629415309, -212.8861406575224748 ) ) ;
#21551 = CIRCLE ( 'NONE', #7887, 1.000000000000000888 ) ;
#21552 = CARTESIAN_POINT ( 'NONE',  ( -90.60121189453791146, -287.8790595574993745, -324.0326797218828574 ) ) ;
#21553 = CARTESIAN_POINT ( 'NONE',  ( -59.66501024252430341, -277.3335391814662785, -344.0541965282037040 ) ) ;
#21554 = CARTESIAN_POINT ( 'NONE',  ( 32.12532965656419037, -295.8909301638625493, -297.8189301995707865 ) ) ;
#21555 = DIRECTION ( 'NONE',  ( 0.000000000000000000, 1.000000000000000000, 0.000000000000000000 ) ) ;
#21556 = CARTESIAN_POINT ( 'NONE',  ( -20.25526795762937127, -294.7662352645559167, -195.3538533559490702 ) ) ;
#21557 = CARTESIAN_POINT ( 'NONE',  ( -103.9252033361590435, -283.6557015111425812, -239.1297574213755297 ) ) ;
#21558 = CARTESIAN_POINT ( 'NONE',  ( -78.78388096887881886, -277.4940363649671440, -207.7884632752493133 ) ) ;
#21559 = CARTESIAN_POINT ( 'NONE',  ( -104.9852800969474771, -271.4930346039406004, -234.9333220023199260 ) ) ;
#21560 = CARTESIAN_POINT ( 'NONE',  ( 35.12264531535633694, -274.7738262835058549, -260.7272554324752036 ) ) ;
#21561 = AXIS2_PLACEMENT_3D ( 'NONE', #62397, #92648, #20235 ) ;
#21562 = CARTESIAN_POINT ( 'NONE',  ( 0.2461993104067672911, -294.0827168792916382, -206.9745455221475936 ) ) ;
#21563 = CARTESIAN_POINT ( 'NONE',  ( -5.951614167666416044, -293.4164558207309597, -204.1803000874634506 ) ) ;
#21564 = ADVANCED_FACE ( 'NONE', ( #18716 ), #90640, .T. ) ;
#21565 = CARTESIAN_POINT ( 'NONE',  ( 25.32043023167499385, -295.4517254781991369, -314.2788136781078947 ) ) ;
#21566 = CARTESIAN_POINT ( 'NONE',  ( -93.08376905849242178, -295.7153849568382498, -317.5166878978336626 ) ) ;
#21567 = CARTESIAN_POINT ( 'NONE',  ( -105.8649150796414631, -292.1513018780649418, -300.9781217295776514 ) ) ;
#21568 = CARTESIAN_POINT ( 'NONE',  ( -70.46819411277715517, -283.6434715493737713, -339.8855456207680277 ) ) ;
#21569 = CARTESIAN_POINT ( 'NONE',  ( -68.31704371975510526, -271.7892202014795657, -201.2033839585289456 ) ) ;
#21570 = CARTESIAN_POINT ( 'NONE',  ( -43.66415077770040654, -285.8078088627343618, -193.5678651683101350 ) ) ;
#21571 = CARTESIAN_POINT ( 'NONE',  ( -110.6540620784711706, -280.3500343965315551, -284.4693485422583308 ) ) ;
#21572 = EDGE_CURVE ( 'NONE', #46575, #87978, #80475, .T. ) ;
#21573 = CARTESIAN_POINT ( 'NONE',  ( -46.74323606647199369, -284.9887471177253246, -197.6808494438146511 ) ) ;
#21574 = CARTESIAN_POINT ( 'NONE',  ( -108.8820235597720796, -288.2595304863650654, -293.0472499839460170 ) ) ;
#21575 = CARTESIAN_POINT ( 'NONE',  ( 79.80194596570532894, 84.98805272827966917, -300.3302785054510196 ) ) ;
#21576 = CARTESIAN_POINT ( 'NONE',  ( -57.40527084919665413, -285.2938994737045277, -200.0557638606933040 ) ) ;
#21577 = CARTESIAN_POINT ( 'NONE',  ( 34.94784481344460403, -282.4341265075883030, -244.8605167064576165 ) ) ;
#21578 = CARTESIAN_POINT ( 'NONE',  ( -23.36657542224108397, -287.9365528975321809, -345.8969585413705090 ) ) ;
#21579 = CARTESIAN_POINT ( 'NONE',  ( -112.2751674014556187, -279.9765246838028361, -284.2680182883651128 ) ) ;
#21580 = CARTESIAN_POINT ( 'NONE',  ( -110.1919046225565779, -279.5696502051916355, -293.9013367939087402 ) ) ;
#21581 = CARTESIAN_POINT ( 'NONE',  ( -104.4412340725470330, -278.7717087096538080, -241.6095519570272927 ) ) ;
#21582 = CARTESIAN_POINT ( 'NONE',  ( -51.90653774012873356, -275.8448939105290947, -197.0981018425740672 ) ) ;
#21583 = CARTESIAN_POINT ( 'NONE',  ( 23.97522895132989618, -292.9312602574916582, -223.7643822824878441 ) ) ;
#21584 = AXIS2_PLACEMENT_3D ( 'NONE', #8531, #53494, #51610 ) ;
#21585 = CARTESIAN_POINT ( 'NONE',  ( 2.161127084883642357, -286.5404046667965758, -333.6965223306931989 ) ) ;
#21586 = CARTESIAN_POINT ( 'NONE',  ( -47.65549479289109769, -293.5233823838627814, -194.8090988526867307 ) ) ;
#21587 = PRODUCT_DEFINITION ( 'UNKNOWN', '', #46159, #29566 ) ;
#21588 = AXIS2_PLACEMENT_3D ( 'NONE', #46917, #90463, #90923 ) ;
#21589 = CARTESIAN_POINT ( 'NONE',  ( -102.8021862705189875, -295.9198773675413463, -237.2458457095668507 ) ) ;
#21590 = CARTESIAN_POINT ( 'NONE',  ( -29.26457252396425801, -284.8693241671346641, -344.4131197844662324 ) ) ;
#21591 = CARTESIAN_POINT ( 'NONE',  ( -72.13839101902910045, -295.1925262915897861, -334.5725704725780361 ) ) ;
#21592 = CARTESIAN_POINT ( 'NONE',  ( 20.13785987141878664, -293.9413351344625198, -219.5712840788302742 ) ) ;
#21593 = CARTESIAN_POINT ( 'NONE',  ( 18.03632735017891520, -281.5246799537732159, -222.6222371292827518 ) ) ;
#21594 = CARTESIAN_POINT ( 'NONE',  ( 37.40854832670542862, -274.3910895064950637, -252.8333351820176063 ) ) ;
#21595 = CARTESIAN_POINT ( 'NONE',  ( -108.7007811131989001, -290.8393973437330260, -299.0176067291662889 ) ) ;
#21596 = CARTESIAN_POINT ( 'NONE',  ( -55.43060388946867079, -281.4220826753064557, -343.9348703573852504 ) ) ;
#21597 = CARTESIAN_POINT ( 'NONE',  ( -114.0910319812618638, -290.8029316756999947, -276.9560068633767287 ) ) ;
#21598 = CARTESIAN_POINT ( 'NONE',  ( -14.56343679039542671, -286.6888367987467063, -200.9305803135136159 ) ) ;
#21599 = CARTESIAN_POINT ( 'NONE',  ( 164.2231345125756263, 300.2961574867697436, -7.500000000000000000 ) ) ;
#21600 = CARTESIAN_POINT ( 'NONE',  ( 201.2091503359040132, 294.9048254156658118, -54.00000000001405454 ) ) ;
#21601 = CARTESIAN_POINT ( 'NONE',  ( 201.9872660792514125, 292.2036060437295646, -68.21650457366665421 ) ) ;
#21602 = CARTESIAN_POINT ( 'NONE',  ( -102.0044027273109890, -277.2841595008096078, -304.5859133658730116 ) ) ;
#21603 = CARTESIAN_POINT ( 'NONE',  ( -66.17868379056844219, -278.5859360690672020, -202.9482055685049033 ) ) ;
#21604 = CARTESIAN_POINT ( 'NONE',  ( -44.03668832469244876, -273.6365553024820088, -193.6206584673421389 ) ) ;
#21605 = CARTESIAN_POINT ( 'NONE',  ( 204.3872521652993157, 292.5237103994863332, -68.38542364661543616 ) ) ;
#21606 = CARTESIAN_POINT ( 'NONE',  ( -104.2686865475563565, -277.6081331592102401, -233.4912823404381186 ) ) ;
#21607 = CARTESIAN_POINT ( 'NONE',  ( -33.43479398991843965, -281.0228628273752634, -344.9164644161824071 ) ) ;
#21608 = CARTESIAN_POINT ( 'NONE',  ( -107.9553395524242347, -298.6746570177957096, -242.1538334752297317 ) ) ;
#21609 = CARTESIAN_POINT ( 'NONE',  ( -101.1804965051250917, -291.5311892881917970, -234.7241560361980817 ) ) ;
#21610 = CARTESIAN_POINT ( 'NONE',  ( 20.73693582700091298, -286.8672207463941959, -315.4160909995291036 ) ) ;
#21611 = CARTESIAN_POINT ( 'NONE',  ( 26.84090953594390427, -275.6458511372166527, -228.0065975243298908 ) ) ;
#21612 = CARTESIAN_POINT ( 'NONE',  ( -91.12253635318792533, -273.2607672393718303, -220.9804657552562333 ) ) ;
#21613 = VERTEX_POINT ( 'NONE', #36193 ) ;
#21614 = DIRECTION ( 'NONE',  ( -0.000000000000000000, -0.000000000000000000, -1.000000000000000000 ) ) ;
#21615 = DIRECTION ( 'NONE',  ( 0.000000000000000000, 0.000000000000000000, -1.000000000000000000 ) ) ;
#21616 = VECTOR ( 'NONE', #55650, 1000.000000000000000 ) ;
#21617 = CARTESIAN_POINT ( 'NONE',  ( -93.90046042582240204, -281.1640195211295463, -220.2570180196736089 ) ) ;
#21618 = CIRCLE ( 'NONE', #66969, 26.04691768583017364 ) ;
#21619 = LINE ( 'NONE', #51766, #71526 ) ;
#21620 = AXIS2_PLACEMENT_3D ( 'NONE', #42450, #56218, #78003 ) ;
#21621 = CARTESIAN_POINT ( 'NONE',  ( -24.83712607667366612, -281.2951122896281504, -198.1263500339461530 ) ) ;
#21622 = CARTESIAN_POINT ( 'NONE',  ( 20.28280433913066361, -282.6345698065748024, -220.8096281756893973 ) ) ;
#21623 = CARTESIAN_POINT ( 'NONE',  ( -65.41694875149451605, -282.4871414713202853, -338.0149038646231361 ) ) ;
#21624 = CARTESIAN_POINT ( 'NONE',  ( -102.9374943536818563, -279.9469793518366600, -305.1182360674529264 ) ) ;
#21625 = CARTESIAN_POINT ( 'NONE',  ( -91.62022936201221057, -271.7408906481244912, -220.4971930892697287 ) ) ;
#21626 = EDGE_CURVE ( 'NONE', #61882, #14772, #29574, .T. ) ;
#21628 = CARTESIAN_POINT ( 'NONE',  ( 209.1333812278717517, 27.85066937593108705, 13.99694255476963889 ) ) ;
#21627 = VECTOR ( 'NONE', #85369, 1000.000000000000000 ) ;
#21629 = EDGE_CURVE ( 'NONE', #18301, #32853, #92567, .T. ) ;
#21630 = CARTESIAN_POINT ( 'NONE',  ( 9.339199855150265961, -232.1443419142230766, 22.50000000000000000 ) ) ;
#21631 = VECTOR ( 'NONE', #90132, 1000.000000000000000 ) ;
#21632 = CARTESIAN_POINT ( 'NONE',  ( -98.66835631091346670, -278.7369042413498619, -316.6774179278179986 ) ) ;
#21633 = LINE ( 'NONE', #50512, #74654 ) ;
#21634 = CARTESIAN_POINT ( 'NONE',  ( -48.42658574098470581, -275.7651966918988933, -346.0170591924380687 ) ) ;
#21635 = EDGE_LOOP ( 'NONE', ( #52239, #23343, #38946, #51175, #34146 ) ) ;
#21636 = DIRECTION ( 'NONE',  ( -0.000000000000000000, -1.000000000000000000, -0.000000000000000000 ) ) ;
#21637 = CARTESIAN_POINT ( 'NONE',  ( -111.3869487363219264, -286.7142499958719668, -256.0995608770604122 ) ) ;
#21638 = CIRCLE ( 'NONE', #50361, 5.000000000000004441 ) ;
#21639 = CARTESIAN_POINT ( 'NONE',  ( 31.95727912934837178, -292.4364572166456924, -246.7458711093032662 ) ) ;
#21640 = CARTESIAN_POINT ( 'NONE',  ( 25.76329977371850433, -287.4832734677033841, -314.3964932657501663 ) ) ;
#21641 = CARTESIAN_POINT ( 'NONE',  ( -105.5224159068926753, -283.1748125050613680, -241.4308018029734342 ) ) ;
#21643 = CARTESIAN_POINT ( 'NONE',  ( -7.834832642210999509, -286.9001114519323323, -338.2931316660093444 ) ) ;
#21642 = CARTESIAN_POINT ( 'NONE',  ( -95.41091995294009109, -283.7589359383159717, -225.1373372570798495 ) ) ;
#21644 = CARTESIAN_POINT ( 'NONE',  ( -51.07723978435029011, -284.4365651535318307, -342.5133578590064758 ) ) ;
#21645 = CARTESIAN_POINT ( 'NONE',  ( -57.55739002344556354, -271.7911514768463235, -198.0829970067160275 ) ) ;
#21646 = CARTESIAN_POINT ( 'NONE',  ( -98.68793262238550312, -283.5598688821616520, -225.0738840330492394 ) ) ;
#21647 = CARTESIAN_POINT ( 'NONE',  ( -63.54299156843381979, -297.3938025511578189, -340.6355299356363275 ) ) ;
#21648 = CARTESIAN_POINT ( 'NONE',  ( -37.94163254081603753, -284.0444955546336132, -195.1968411470654132 ) ) ;
#21649 = VECTOR ( 'NONE', #25477, 1000.000000000000000 ) ;
#21650 = CARTESIAN_POINT ( 'NONE',  ( -71.06063647708360520, -280.5370070859619318, -205.3358944144751490 ) ) ;
#21651 = CARTESIAN_POINT ( 'NONE',  ( -3.081797100774910980, -288.5037884121805405, -203.4416555286214816 ) ) ;
#21652 = CARTESIAN_POINT ( 'NONE',  ( 197.8594331107396727, 290.2795092986285113, -7.113038391050248599 ) ) ;
#21653 = CYLINDRICAL_SURFACE ( 'NONE', #70087, 0.5000000000000004441 ) ;
#21654 = CARTESIAN_POINT ( 'NONE',  ( 36.38437959071472250, -295.6839235819234091, -286.9658801958458412 ) ) ;
#21655 = AXIS2_PLACEMENT_3D ( 'NONE', #78179, #13317, #43574 ) ;
#21656 = CARTESIAN_POINT ( 'NONE',  ( -111.4726614747209226, -276.4058186460673596, -281.7453711091009154 ) ) ;
#21657 = CARTESIAN_POINT ( 'NONE',  ( -103.6642287301438472, -289.2420868535085106, -309.2669111937612456 ) ) ;
#21658 = CARTESIAN_POINT ( 'NONE',  ( -80.64042831410260703, -294.0503834968018282, -330.1244892959138610 ) ) ;
#21659 = CARTESIAN_POINT ( 'NONE',  ( -24.77571488164446123, -278.9006523987242190, -197.9502107130680315 ) ) ;
#21660 = CARTESIAN_POINT ( 'NONE',  ( -86.23798008150411931, -271.4478677781171427, -214.1634056662846035 ) ) ;
#21661 = CARTESIAN_POINT ( 'NONE',  ( -19.97174117925349179, -293.5951458085277181, -198.8975187062117129 ) ) ;
#21662 = CARTESIAN_POINT ( 'NONE',  ( -54.49178911615188525, -276.3376638359844719, -195.3683826091709363 ) ) ;
#21663 = CARTESIAN_POINT ( 'NONE',  ( 8.474283869770276922, -292.9172637434522812, -331.3824532780968752 ) ) ;
#21664 = CARTESIAN_POINT ( 'NONE',  ( -0.5753915663916416845, -290.1554236723253553, -334.4096276911703853 ) ) ;
#21665 = CARTESIAN_POINT ( 'NONE',  ( -5.014621696398503303, -290.7117910480880028, -201.5938727460895734 ) ) ;
#21666 = CARTESIAN_POINT ( 'NONE',  ( 26.21402754858381812, -289.4836882163552332, -307.5569713674225341 ) ) ;
#21667 = DIRECTION ( 'NONE',  ( 0.000000000000000000, 0.000000000000000000, 1.000000000000000000 ) ) ;
#21668 = CARTESIAN_POINT ( 'NONE',  ( -104.1911113380295717, -290.9541666594027447, -300.2142578689294510 ) ) ;
#21669 = DIRECTION ( 'NONE',  ( 1.000000000000000000, 0.000000000000000000, 0.000000000000000000 ) ) ;
#21670 = CARTESIAN_POINT ( 'NONE',  ( -23.36922114259783001, -290.0825351749548418, -345.7328052492806592 ) ) ;
#21672 = CARTESIAN_POINT ( 'NONE',  ( -110.3678007572729030, -290.5772078642548877, -268.4617592813915508 ) ) ;
#21671 = CARTESIAN_POINT ( 'NONE',  ( 22.45777935031969363, -278.9470893438970052, -224.4877774330086595 ) ) ;
#21673 = CARTESIAN_POINT ( 'NONE',  ( -94.94878642804771118, -279.5774029742238440, -219.3006841850539956 ) ) ;
#21674 = CARTESIAN_POINT ( 'NONE',  ( 37.52681219251520162, -281.4434688679618262, -288.3184521114259837 ) ) ;
#21675 = CARTESIAN_POINT ( 'NONE',  ( 35.95588706133857215, -285.3479802348275598, -254.4719907163343748 ) ) ;
#21676 = CARTESIAN_POINT ( 'NONE',  ( 196.4656634449348473, 42.34360782803825174, 11.30484575918238299 ) ) ;
#21677 = CARTESIAN_POINT ( 'NONE',  ( 34.96886250822412734, -279.4738751420048857, -253.5668327880892718 ) ) ;
#21678 = CARTESIAN_POINT ( 'NONE',  ( -95.99983296993552528, -283.1944355236548745, -223.6254345568210908 ) ) ;
#21679 = CARTESIAN_POINT ( 'NONE',  ( 206.6166011988532887, 1.019566348684629364, 7.291626467228960351 ) ) ;
#21680 = CARTESIAN_POINT ( 'NONE',  ( -90.56061837288628169, -277.7949446385939609, -215.6024258239367555 ) ) ;
#21681 = CARTESIAN_POINT ( 'NONE',  ( -85.30882903859010469, -284.3271952661763180, -210.5226098715470471 ) ) ;
#21682 = CARTESIAN_POINT ( 'NONE',  ( -93.90973673680072409, -274.0109500682585804, -223.9447701593392992 ) ) ;
#21683 = LINE ( 'NONE', #50080, #44320 ) ;
#21684 = CARTESIAN_POINT ( 'NONE',  ( -111.1049168002749070, -292.1052211301469583, -273.9681564387738604 ) ) ;
#21685 = CARTESIAN_POINT ( 'NONE',  ( 34.16391560519255677, -276.6340024219124984, -243.4250230463540845 ) ) ;
#21686 = CARTESIAN_POINT ( 'NONE',  ( 17.44828432164722543, -275.9081584519254875, -318.6515565660632774 ) ) ;
#21687 = CARTESIAN_POINT ( 'NONE',  ( -58.96106121763084218, -297.3320423909741521, -342.1775776033581451 ) ) ;
#21688 = CARTESIAN_POINT ( 'NONE',  ( -26.14246142706570453, -289.0800028626284757, -346.5423299511843993 ) ) ;
#21689 = CARTESIAN_POINT ( 'NONE',  ( 23.08845653405152021, -280.2472594782648798, -315.7209059740592352 ) ) ;
#21690 = CARTESIAN_POINT ( 'NONE',  ( 19.41709738036474064, -292.6775777614255958, -218.3280620478390972 ) ) ;
#21691 = CARTESIAN_POINT ( 'NONE',  ( -70.31595892442398110, -290.6651600909797253, -204.9691711874021678 ) ) ;
#21692 = AXIS2_PLACEMENT_3D ( 'NONE', #47005, #75909, #3008 ) ;
#21693 = CARTESIAN_POINT ( 'NONE',  ( -47.38951087331584944, -293.1796984727084237, -344.6850182177905708 ) ) ;
#21694 = ORIENTED_EDGE ( 'NONE', *, *, #85093, .F. ) ;
#21695 = CARTESIAN_POINT ( 'NONE',  ( 196.8803347170859865, 73.40565171261611965, 12.50000000000000711 ) ) ;
#21696 = TOROIDAL_SURFACE ( 'NONE', #17151, 1.000000000000000000, 0.5000000000000000000 ) ;
#21697 = CARTESIAN_POINT ( 'NONE',  ( -55.02118321038742010, -291.3262505632821444, -199.4708907336494121 ) ) ;
#21698 = CYLINDRICAL_SURFACE ( 'NONE', #42939, 3.000000000000002665 ) ;
#21699 = CARTESIAN_POINT ( 'NONE',  ( -80.81485487069150508, -286.4195236320518347, -207.0284344941582049 ) ) ;
#21700 = CARTESIAN_POINT ( 'NONE',  ( -53.28691492658257545, -271.3380690714491266, -200.3538533559491555 ) ) ;
#21701 = CARTESIAN_POINT ( 'NONE',  ( -19.35408185640407197, -293.8850963931893148, -345.0433476254814309 ) ) ;
#21702 = CARTESIAN_POINT ( 'NONE',  ( -67.67035877338909700, -284.7570530858516804, -340.5997878055861179 ) ) ;
#21703 = CARTESIAN_POINT ( 'NONE',  ( -104.5967266486639460, -284.7680172284426021, -241.8452622724917660 ) ) ;
#21704 = VECTOR ( 'NONE', #54708, 1000.000000000000114 ) ;
#21705 = CARTESIAN_POINT ( 'NONE',  ( 16.11401278437593731, -277.7965801984698828, -321.0877826620890687 ) ) ;
#21706 = CARTESIAN_POINT ( 'NONE',  ( 36.53923402363708561, -291.4348426970789774, -259.7096217587803721 ) ) ;
#21707 = CARTESIAN_POINT ( 'NONE',  ( 35.71054697486245288, -295.1565824653816321, -258.3932275606181861 ) ) ;
#21708 = ADVANCED_FACE ( 'NONE', ( #7771, #44210 ), #50398, .F. ) ;
#21709 = CARTESIAN_POINT ( 'NONE',  ( -32.40912050689573931, -275.7836397569085420, -343.6424984516066843 ) ) ;
#21710 = ORIENTED_EDGE ( 'NONE', *, *, #44275, .T. ) ;
#21711 = CARTESIAN_POINT ( 'NONE',  ( 195.2722580762363123, 41.12091610201859027, 13.20958711401371133 ) ) ;
#21712 = CARTESIAN_POINT ( 'NONE',  ( 26.49183720988387947, -293.7858838100850676, -313.3846441332607355 ) ) ;
#21713 = CARTESIAN_POINT ( 'NONE',  ( 37.07056929121656452, -289.5168318378418917, -273.8024871024016988 ) ) ;
#21714 = CARTESIAN_POINT ( 'NONE',  ( 201.6526253774845543, 295.4708909185295056, -54.00000000003612399 ) ) ;
#21715 = AXIS2_PLACEMENT_3D ( 'NONE', #55900, #26059, #26546 ) ;
#21716 = CARTESIAN_POINT ( 'NONE',  ( 53.12040451806458918, -300.2394943505627225, -193.6540424337711670 ) ) ;
#21717 = CARTESIAN_POINT ( 'NONE',  ( -54.78869651922693862, -286.4734590947068114, -199.3193451868030763 ) ) ;
#21718 = ORIENTED_EDGE ( 'NONE', *, *, #85032, .F. ) ;
#21719 = CARTESIAN_POINT ( 'NONE',  ( -56.48635047578894586, -278.8701409524386463, -195.9671829698715442 ) ) ;
#21720 = CARTESIAN_POINT ( 'NONE',  ( -44.77749932147799683, -295.7952024755983871, -346.9521676764430254 ) ) ;
#21721 = CARTESIAN_POINT ( 'NONE',  ( -38.91860484509828666, -287.2113282747291692, -346.1095097492282093 ) ) ;
#21722 = CARTESIAN_POINT ( 'NONE',  ( -113.1823023974315277, -296.7166740914675529, -283.8511490800067349 ) ) ;
#21723 = CARTESIAN_POINT ( 'NONE',  ( 14.88766405255949543, -293.1466135064929404, -219.2575238806394680 ) ) ;
#21724 = DIRECTION ( 'NONE',  ( 0.000000000000000000, 1.000000000000000000, 0.000000000000000000 ) ) ;
#21725 = AXIS2_PLACEMENT_3D ( 'NONE', #18990, #69175, #83354 ) ;
#21726 = LINE ( 'NONE', #87480, #79584 ) ;
#21727 = CARTESIAN_POINT ( 'NONE',  ( 140.6539576904058606, 130.0000000000000568, -12.50000000000000000 ) ) ;
#21728 = CARTESIAN_POINT ( 'NONE',  ( -18.37326389616899647, -287.8122263031095827, -196.3950398920317753 ) ) ;
#21729 = CARTESIAN_POINT ( 'NONE',  ( 36.57525178469694538, -291.4809262143062369, -305.9938812882205070 ) ) ;
#21730 = ORIENTED_EDGE ( 'NONE', *, *, #29582, .T. ) ;
#21731 = CARTESIAN_POINT ( 'NONE',  ( -106.0807342157223729, -278.3460858061934005, -235.7714311475588715 ) ) ;
#21732 = CARTESIAN_POINT ( 'NONE',  ( -31.98978832152237572, -284.9846209702211013, -345.0028319717018803 ) ) ;
#21733 = CARTESIAN_POINT ( 'NONE',  ( -80.58964352083211224, -284.0533803937519224, -207.3034389648248066 ) ) ;
#21734 = ADVANCED_FACE ( 'NONE', ( #29095 ), #35261, .F. ) ;
#21735 = CARTESIAN_POINT ( 'NONE',  ( -15.45107799362714296, -286.8465849420167046, -341.5635195849741308 ) ) ;
#21736 = CARTESIAN_POINT ( 'NONE',  ( -20.37922041317234090, -278.6970899088186684, -344.2565487930448285 ) ) ;
#21737 = CARTESIAN_POINT ( 'NONE',  ( -66.84993899834188369, -298.1471030697205151, -203.5099194421589459 ) ) ;
#21738 = VERTEX_POINT ( 'NONE', #80210 ) ;
#21739 = CARTESIAN_POINT ( 'NONE',  ( 33.21898569042035376, -292.5075653531688999, -290.9594915361004723 ) ) ;
#21741 = CARTESIAN_POINT ( 'NONE',  ( -93.16267359623789446, -278.5708008655215622, -223.1411073630389126 ) ) ;
#21740 = CARTESIAN_POINT ( 'NONE',  ( -85.10524184118780511, -277.7330176942925277, -325.6335496229921773 ) ) ;
#21742 = CARTESIAN_POINT ( 'NONE',  ( -21.43238691046070699, -275.3312447751002310, -195.3385463002959739 ) ) ;
#21743 = CARTESIAN_POINT ( 'NONE',  ( -109.2282164417697032, -277.6850198581814197, -243.7441700496726185 ) ) ;
#21744 = CARTESIAN_POINT ( 'NONE',  ( 199.7491719457015620, 292.1072351560490006, -82.63401296664939366 ) ) ;
#21745 = CARTESIAN_POINT ( 'NONE',  ( -104.0793581943162422, -297.4900294610848164, -307.6806784570537729 ) ) ;
#21746 = CARTESIAN_POINT ( 'NONE',  ( -37.30987171927208124, -279.5519495502701943, -345.3611179825600175 ) ) ;
#21747 = CARTESIAN_POINT ( 'NONE',  ( 82.68081405346485724, -297.0478052522023518, -195.0828515018483529 ) ) ;
#21748 = CARTESIAN_POINT ( 'NONE',  ( -11.92766018874138290, -287.4705866327009858, -201.5980999603520729 ) ) ;
#21749 = AXIS2_PLACEMENT_3D ( 'NONE', #57625, #86468, #65682 ) ;
#21750 = CARTESIAN_POINT ( 'NONE',  ( -113.1427923795099844, -286.3884599297053910, -264.3510049481332658 ) ) ;
#21751 = CARTESIAN_POINT ( 'NONE',  ( 17.89711178524258983, -287.5828457132016638, -318.3176477992096807 ) ) ;
#21752 = CARTESIAN_POINT ( 'NONE',  ( -97.99977793551259708, -283.4269155914028033, -317.6910715030023198 ) ) ;
#21753 = CARTESIAN_POINT ( 'NONE',  ( -41.07145826836466540, -278.4042980647125773, -196.6554240337372335 ) ) ;
#21754 = CARTESIAN_POINT ( 'NONE',  ( -94.35577204744396340, -285.7491435983187102, -317.9033211951823432 ) ) ;
#21755 = CARTESIAN_POINT ( 'NONE',  ( 33.98978738806516020, -280.2746516633096689, -288.9188051615073505 ) ) ;
#21756 = EDGE_CURVE ( 'NONE', #93354, #36970, #78821, .T. ) ;
#21757 = CARTESIAN_POINT ( 'NONE',  ( -40.51037746368601233, -278.4079712347958093, -343.7984783205209851 ) ) ;
#21758 = CARTESIAN_POINT ( 'NONE',  ( 20.07471269429220584, -276.6814959992061631, -315.5625027960275588 ) ) ;
#21759 = CARTESIAN_POINT ( 'NONE',  ( 7.688634765473509880, -287.2478717357618621, -332.3964949390118022 ) ) ;
#21760 = CARTESIAN_POINT ( 'NONE',  ( -52.87495473942416169, -284.0490481734789796, -345.6675826657482844 ) ) ;
#21761 = CARTESIAN_POINT ( 'NONE',  ( 33.51170862437711406, -282.4280025500357851, -300.4858884375234993 ) ) ;
#21762 = ORIENTED_EDGE ( 'NONE', *, *, #17448, .T. ) ;
#21763 = ORIENTED_EDGE ( 'NONE', *, *, #80495, .T. ) ;
#21764 = FACE_OUTER_BOUND ( 'NONE', #30880, .T. ) ;
#21765 = CARTESIAN_POINT ( 'NONE',  ( -54.20329078882887330, -291.1267332211077132, -344.2796373406740713 ) ) ;
#21766 = CARTESIAN_POINT ( 'NONE',  ( -97.06800996909851165, -289.8815949450092262, -222.5482934687692875 ) ) ;
#21767 = CARTESIAN_POINT ( 'NONE',  ( -81.20237167259689670, -272.4984748850349092, -211.6489631753028391 ) ) ;
#21768 = CARTESIAN_POINT ( 'NONE',  ( 37.32496265445777084, -292.6703791436969482, -251.9708418573292192 ) ) ;
#21769 = CARTESIAN_POINT ( 'NONE',  ( -89.16223791121014131, -288.2774164101108454, -322.7571065274370881 ) ) ;
#21770 = CARTESIAN_POINT ( 'NONE',  ( 7.305105622832725132, -290.9101547363768532, -211.3303061364287032 ) ) ;
#21771 = CARTESIAN_POINT ( 'NONE',  ( 36.02762337789592095, -288.8018686036191411, -273.7630125538476022 ) ) ;
#21772 = CARTESIAN_POINT ( 'NONE',  ( -110.4542110544635705, -292.8376638359844719, -287.0812184334320705 ) ) ;
#21773 = VECTOR ( 'NONE', #37231, 1000.000000000000000 ) ;
#21774 = CARTESIAN_POINT ( 'NONE',  ( -43.00518548740925695, -291.1238205171648588, -345.1469828421396642 ) ) ;
#21775 = CARTESIAN_POINT ( 'NONE',  ( -109.7821149103507707, -288.2945442640377678, -290.4213955173162844 ) ) ;
#21776 = CARTESIAN_POINT ( 'NONE',  ( -97.03941445755313566, -293.1737498562713427, -224.9401512154376803 ) ) ;
#21777 = CARTESIAN_POINT ( 'NONE',  ( -90.90540367049743509, -284.7774704727244170, -320.3044669999755456 ) ) ;
#21778 = CARTESIAN_POINT ( 'NONE',  ( -5.406741242633555267, -294.4714841033494963, -202.3156417773798523 ) ) ;
#21779 = CARTESIAN_POINT ( 'NONE',  ( 200.6103193995254230, 249.5000000000000568, -2.464576988612307229 ) ) ;
#21780 = DIRECTION ( 'NONE',  ( 0.000000000000000000, 1.000000000000000000, 0.000000000000000000 ) ) ;
#21781 = AXIS2_PLACEMENT_3D ( 'NONE', #78153, #13757, #14233 ) ;
#21782 = CARTESIAN_POINT ( 'NONE',  ( -65.63358930329401630, -275.6639188389321475, -200.5047410037102509 ) ) ;
#21783 = CARTESIAN_POINT ( 'NONE',  ( -40.25099234621683308, -282.2868198995290072, -343.4647276480588403 ) ) ;
#21784 = CARTESIAN_POINT ( 'NONE',  ( -64.81096724150229704, -281.4107401070241963, -340.1496558204850089 ) ) ;
#21785 = CARTESIAN_POINT ( 'NONE',  ( -114.2049636948820819, -295.7230768984458678, -272.4551688669206442 ) ) ;
#21786 = CARTESIAN_POINT ( 'NONE',  ( -59.76155105279463697, -271.9976995216208024, -199.7714892471298640 ) ) ;
#21787 = CARTESIAN_POINT ( 'NONE',  ( -71.12780261895926515, -275.5815619626100670, -336.6922078231229420 ) ) ;
#21788 = CARTESIAN_POINT ( 'NONE',  ( -88.48084421931424970, -298.6323826213073858, -217.5071803188237993 ) ) ;
#21789 = VECTOR ( 'NONE', #30275, 1000.000000000000000 ) ;
#21790 = CARTESIAN_POINT ( 'NONE',  ( 6.427858286978637814, -295.8699494810848591, -329.5820562702344318 ) ) ;
#21791 = DIRECTION ( 'NONE',  ( 0.000000000000000000, 1.000000000000000000, 0.000000000000000000 ) ) ;
#21792 = CARTESIAN_POINT ( 'NONE',  ( -0.6681704988668493161, -295.3547369127751949, -333.7249769427886008 ) ) ;
#21793 = DIRECTION ( 'NONE',  ( -1.000000000000000000, 0.000000000000000000, 0.000000000000000000 ) ) ;
#21795 = CARTESIAN_POINT ( 'NONE',  ( -109.7362330339659025, -296.6809605365436937, -260.5967397307236979 ) ) ;
#21794 = CARTESIAN_POINT ( 'NONE',  ( 32.34812088404733998, -285.1984743357985508, -241.5587551745245207 ) ) ;
#21796 = TOROIDAL_SURFACE ( 'NONE', #39927, 4.499999999999990230, 0.5000000000000000000 ) ;
#21797 = CARTESIAN_POINT ( 'NONE',  ( -97.17239457006462544, -283.9018604790301197, -318.8512924680750871 ) ) ;
#21798 = CARTESIAN_POINT ( 'NONE',  ( 27.12237205103609128, -286.6659975600267103, -228.2882325385497779 ) ) ;
#21799 = CARTESIAN_POINT ( 'NONE',  ( 22.47419734123972646, -290.9360399087347560, -225.3934980815385813 ) ) ;
#21800 = CARTESIAN_POINT ( 'NONE',  ( -73.68023496432654440, -278.7795507255493135, -202.6433952533539582 ) ) ;
#21801 = CARTESIAN_POINT ( 'NONE',  ( -37.30987171927208834, -277.5523547857346784, -195.3611179825600175 ) ) ;
#21802 = DIRECTION ( 'NONE',  ( -0.000000000000000000, -0.000000000000000000, -1.000000000000000000 ) ) ;
#21803 = CIRCLE ( 'NONE', #18742, 4.999999999999976907 ) ;
#21804 = CARTESIAN_POINT ( 'NONE',  ( 33.46087754133158398, -286.6034603034618158, -289.8918952704985941 ) ) ;
#21806 = CARTESIAN_POINT ( 'NONE',  ( 200.5815643859950228, 65.97596549932491428, -9.780880230328993008 ) ) ;
#21805 = CARTESIAN_POINT ( 'NONE',  ( -113.8784774835396689, -289.5335016852888543, -265.5016714038294481 ) ) ;
#21807 = FACE_OUTER_BOUND ( 'NONE', #12067, .T. ) ;
#21808 = CARTESIAN_POINT ( 'NONE',  ( -104.6580641169477133, -297.7477578156853610, -300.7340600901302992 ) ) ;
#21810 = CARTESIAN_POINT ( 'NONE',  ( -1.952115106104068909, -280.2014284063606055, -206.4888645481774176 ) ) ;
#21809 = CARTESIAN_POINT ( 'NONE',  ( -96.14021537502127046, -293.9268482520018893, -317.5105341253381539 ) ) ;
#21811 = CARTESIAN_POINT ( 'NONE',  ( -68.22423139129976732, -295.6133665174211274, -340.8967066403378681 ) ) ;
#21812 = CARTESIAN_POINT ( 'NONE',  ( -110.2254087330158399, -280.3244697979502007, -288.1056715706646969 ) ) ;
#21813 = CARTESIAN_POINT ( 'NONE',  ( -106.0223267440893551, -295.9505583568613361, -244.7909038657860776 ) ) ;
#21814 = ORIENTED_EDGE ( 'NONE', *, *, #7026, .T. ) ;
#21815 = CARTESIAN_POINT ( 'NONE',  ( 197.3133474189782248, 42.36571313990103960, 12.74999999999998757 ) ) ;
#21816 = CARTESIAN_POINT ( 'NONE',  ( -36.14237516623786206, -285.0169309673198654, -344.9962868110795853 ) ) ;
#21817 = CARTESIAN_POINT ( 'NONE',  ( 156.4851178187871312, 0.000000000000000000, 10.00000000000000000 ) ) ;
#21818 = CARTESIAN_POINT ( 'NONE',  ( -95.99890600148557951, -287.4094976428776249, -317.0979686699210447 ) ) ;
#21819 = CARTESIAN_POINT ( 'NONE',  ( -2.806864703871376321, -275.8045490108797821, -339.0161603780088058 ) ) ;
#21820 = CARTESIAN_POINT ( 'NONE',  ( -17.43055719457050401, -292.1495172258112234, -200.0764356445261569 ) ) ;
#21821 = CARTESIAN_POINT ( 'NONE',  ( 29.59441305995499150, -282.6588529956806042, -239.4125356282316375 ) ) ;
#21822 = CARTESIAN_POINT ( 'NONE',  ( -51.73724255811971062, -275.4651912250458849, -197.9263790437122168 ) ) ;
#21823 = CARTESIAN_POINT ( 'NONE',  ( -34.48831178038967238, -284.6169690265235204, -346.5076779307435686 ) ) ;
#21824 = CARTESIAN_POINT ( 'NONE',  ( 21.31805035291759864, -280.9634454126324385, -314.4972323636638976 ) ) ;
#21825 = CARTESIAN_POINT ( 'NONE',  ( -106.0948902248394461, -280.1586023692168510, -300.4577895527651208 ) ) ;
#21826 = CARTESIAN_POINT ( 'NONE',  ( 53.58753502002358715, -299.1611516537437296, -193.3610657143116782 ) ) ;
#21827 = CARTESIAN_POINT ( 'NONE',  ( 39.38032164253318967, -275.4672258268549285, -276.8980423297837206 ) ) ;
#21828 = CARTESIAN_POINT ( 'NONE',  ( 33.72876223152904629, -295.7600498889233904, -292.5039176749680223 ) ) ;
#21829 = CARTESIAN_POINT ( 'NONE',  ( 199.4392256788250677, 65.82574266882505754, -7.741079165001061746 ) ) ;
#21830 = CARTESIAN_POINT ( 'NONE',  ( 0.000000000000000000, 0.000000000000000000, 7.500000000000000000 ) ) ;
#21831 = CARTESIAN_POINT ( 'NONE',  ( 12.56411675703698272, -292.5052596951728674, -327.4369296289947897 ) ) ;
#21832 = CARTESIAN_POINT ( 'NONE',  ( -38.07669348961997002, -273.5503480781993062, -197.3032763320682932 ) ) ;
#21833 = AXIS2_PLACEMENT_3D ( 'NONE', #14450, #49006, #72202 ) ;
#21834 = CARTESIAN_POINT ( 'NONE',  ( -53.26371836535142990, -293.3718100777188056, -195.6800550602520730 ) ) ;
#21836 = CARTESIAN_POINT ( 'NONE',  ( -27.91326286185599059, -293.3742606311471377, -194.2872419503543426 ) ) ;
#21835 = CARTESIAN_POINT ( 'NONE',  ( 31.98288692825981272, -278.4805209788417528, -303.7098442033569654 ) ) ;
#21837 = CARTESIAN_POINT ( 'NONE',  ( -56.51124884301842854, -291.2998115444024734, -342.7514043404716517 ) ) ;
#21838 = CARTESIAN_POINT ( 'NONE',  ( -108.8765098679053551, -276.2660599907086976, -292.5075319989022660 ) ) ;
#21839 = CARTESIAN_POINT ( 'NONE',  ( -79.42635005625847100, -279.5450601268025252, -331.8257965372164335 ) ) ;
#21840 = CARTESIAN_POINT ( 'NONE',  ( 33.17283793648693546, -291.3193158478521241, -246.3464828689928936 ) ) ;
#21841 = CARTESIAN_POINT ( 'NONE',  ( 35.30128606378762157, -283.6890844606402311, -292.0662504952661038 ) ) ;
#21842 = EDGE_LOOP ( 'NONE', ( #28374, #48829, #8511, #62270 ) ) ;
#21843 = CARTESIAN_POINT ( 'NONE',  ( 11.92782979010978650, -282.0111553900312629, -324.2554674854873724 ) ) ;
#21844 = CARTESIAN_POINT ( 'NONE',  ( -61.96146498611592079, -280.8192414426507071, -197.6734361564319897 ) ) ;
#21845 = VECTOR ( 'NONE', #28775, 1000.000000000000000 ) ;
#21846 = CARTESIAN_POINT ( 'NONE',  ( -95.04578693486982388, -282.6621991725297676, -320.7421370779891276 ) ) ;
#21847 = CARTESIAN_POINT ( 'NONE',  ( -113.9964095188055921, -279.4418686648850780, -274.4691273028197429 ) ) ;
#21848 = EDGE_CURVE ( 'NONE', #35960, #64853, #49924, .T. ) ;
#21849 =( NAMED_UNIT ( * ) PLANE_ANGLE_UNIT ( ) SI_UNIT ( $, .RADIAN. ) );
#21850 = CARTESIAN_POINT ( 'NONE',  ( 12.26866339178549836, -277.8961259548783005, -328.3397311290792118 ) ) ;
#21851 = CARTESIAN_POINT ( 'NONE',  ( -67.74223827176244583, -282.1233781216987495, -207.3071070584150277 ) ) ;
#21852 = VERTEX_POINT ( 'NONE', #78361 ) ;
#21853 = ORIENTED_EDGE ( 'NONE', *, *, #61799, .T. ) ;
#21854 = CARTESIAN_POINT ( 'NONE',  ( -73.84190424486551763, -299.5675580659681145, -204.8421455432032587 ) ) ;
#21855 = CIRCLE ( 'NONE', #17101, 2.186979415864515275 ) ;
#21856 = CARTESIAN_POINT ( 'NONE',  ( -67.48958005552772477, -275.4697008299434060, -338.6469301346039060 ) ) ;
#21857 = CARTESIAN_POINT ( 'NONE',  ( -42.01434047100565294, -293.7541517698392113, -194.5182511676785566 ) ) ;
#21858 = CARTESIAN_POINT ( 'NONE',  ( 27.58086407627208203, -292.4444518529926427, -236.7612173134350826 ) ) ;
#21859 = CARTESIAN_POINT ( 'NONE',  ( -109.8097070444448349, -289.7315620404317542, -296.3631503910306151 ) ) ;
#21860 = DIRECTION ( 'NONE',  ( 2.220446049250312686E-15, 0.000000000000000000, 1.000000000000000000 ) ) ;
#21862 = CARTESIAN_POINT ( 'NONE',  ( -96.39396084986779556, -283.5666449385989836, -226.0974656190506948 ) ) ;
#21861 = CARTESIAN_POINT ( 'NONE',  ( -6.055683107054672831, -293.2236937891813113, -340.0733223194781658 ) ) ;
#21863 = CARTESIAN_POINT ( 'NONE',  ( -11.85806695174627379, -294.2477261964335753, -200.5822373150134581 ) ) ;
#21864 = CARTESIAN_POINT ( 'NONE',  ( -33.45349800470193458, -284.3173967799020829, -343.7640020148577378 ) ) ;
#21865 = CARTESIAN_POINT ( 'NONE',  ( -108.5756480587519519, -291.1291894498090187, -298.9713412359251379 ) ) ;
#21866 = CARTESIAN_POINT ( 'NONE',  ( 33.81890197185039426, -281.8262572961833143, -253.8034263965678292 ) ) ;
#21867 = CARTESIAN_POINT ( 'NONE',  ( 38.46126848937843334, -292.2037924384628127, -258.9630470732304843 ) ) ;
#21868 = VECTOR ( 'NONE', #57358, 1000.000000000000000 ) ;
#21869 = CARTESIAN_POINT ( 'NONE',  ( -65.37855612990146881, -290.2121659811692211, -341.9581913109369680 ) ) ;
#21870 = CARTESIAN_POINT ( 'NONE',  ( 20.53075473645706595, -288.7311126993523658, -321.0791517388142893 ) ) ;
#21871 = CARTESIAN_POINT ( 'NONE',  ( -19.81791149459072443, -286.4504710328173473, -199.4956338847855477 ) ) ;
#21872 = ORIENTED_EDGE ( 'NONE', *, *, #74020, .F. ) ;
#21873 = DIRECTION ( 'NONE',  ( 0.000000000000000000, 0.000000000000000000, -1.000000000000000000 ) ) ;
#21875 = AXIS2_PLACEMENT_3D ( 'NONE', #78090, #49657, #93211 ) ;
#21874 = CARTESIAN_POINT ( 'NONE',  ( 5.928315720354267349, -296.3330965711999170, -332.6183948048196157 ) ) ;
#21876 = CARTESIAN_POINT ( 'NONE',  ( -97.03326717451039940, -294.5914587491922134, -318.2380484803269383 ) ) ;
#21877 = EDGE_CURVE ( 'NONE', #33695, #78809, #50871, .T. ) ;
#21878 = CARTESIAN_POINT ( 'NONE',  ( -108.5155169900114913, -277.8378125780733967, -253.1072418331954452 ) ) ;
#21879 = CARTESIAN_POINT ( 'NONE',  ( -106.7849836629186342, -272.4847827561006852, -237.2377534953233180 ) ) ;
#21880 = CARTESIAN_POINT ( 'NONE',  ( -45.18357789638266553, -293.6329974703625112, -343.6869863054122902 ) ) ;
#21881 = CARTESIAN_POINT ( 'NONE',  ( 34.81675088510943539, -277.0973894392573129, -253.8384461560079899 ) ) ;
#21882 = CARTESIAN_POINT ( 'NONE',  ( -86.10397844571753012, -271.5075962882691556, -214.3184720172129119 ) ) ;
#21883 = CARTESIAN_POINT ( 'NONE',  ( 35.10340015363704680, -294.6016065963480060, -258.4996747531023402 ) ) ;
#21884 = CARTESIAN_POINT ( 'NONE',  ( -39.68520223580119932, -296.1619122369672255, -343.6452470055027106 ) ) ;
#21885 = CARTESIAN_POINT ( 'NONE',  ( 222.8344101925596306, 6.488953147413177264E-16, 8.757359312880714342 ) ) ;
#21886 = CARTESIAN_POINT ( 'NONE',  ( -92.30437754061871658, -295.2687883221487368, -219.0101579970234127 ) ) ;
#21887 = CARTESIAN_POINT ( 'NONE',  ( -35.83896356287420559, -298.7219130958772553, -193.4628888928136519 ) ) ;
#21888 = CARTESIAN_POINT ( 'NONE',  ( -57.42091067607932331, -275.7932986017389680, -198.0447492931461397 ) ) ;
#21889 = CARTESIAN_POINT ( 'NONE',  ( -97.53549015575222825, -290.9137989181900821, -312.0978437768437743 ) ) ;
#21890 = CARTESIAN_POINT ( 'NONE',  ( 10.30852592983934635, -294.7062326978360716, -325.6923337952869701 ) ) ;
#21891 = CARTESIAN_POINT ( 'NONE',  ( -98.30395453017600005, -279.9312396835658774, -314.6776356712832126 ) ) ;
#21892 = CARTESIAN_POINT ( 'NONE',  ( -111.2502540149691868, -277.4866846746982674, -250.5413148976952016 ) ) ;
#21893 = CARTESIAN_POINT ( 'NONE',  ( -34.49106612597262966, -282.3657913624235221, -347.2063304075936117 ) ) ;
#21894 = CARTESIAN_POINT ( 'NONE',  ( 34.62927384755150229, -274.5576514632986118, -243.2780662459047676 ) ) ;
#21895 = CARTESIAN_POINT ( 'NONE',  ( -67.03176417578455926, -278.0692872619824811, -200.1831975705065361 ) ) ;
#21896 = CARTESIAN_POINT ( 'NONE',  ( -66.62418970945078911, -277.6693198032149894, -201.1327695089344445 ) ) ;
#21897 = CARTESIAN_POINT ( 'NONE',  ( -95.67031176573394191, -295.8620059351299574, -225.6302553106916662 ) ) ;
#21898 = CARTESIAN_POINT ( 'NONE',  ( 35.37472182365043238, -277.3157794448280811, -251.9432563880057501 ) ) ;
#21899 = CARTESIAN_POINT ( 'NONE',  ( 197.1513938986460062, -142.7221692137691775, 1.978481845683761620 ) ) ;
#21900 = CARTESIAN_POINT ( 'NONE',  ( -68.91059120213252243, -289.6592936070547921, -201.9233172620456287 ) ) ;
#21901 = CARTESIAN_POINT ( 'NONE',  ( -73.17386796344683830, -289.5138142485358799, -338.5305202638644460 ) ) ;
#21902 = CARTESIAN_POINT ( 'NONE',  ( 24.61856256205270910, -276.9766916708151143, -227.7830066726236851 ) ) ;
#21903 = CARTESIAN_POINT ( 'NONE',  ( -93.49924585855379178, -271.2433656042375674, -220.6486375772183806 ) ) ;
#21904 = CARTESIAN_POINT ( 'NONE',  ( -87.63651115912733758, -284.5681281219980292, -212.1994581078369890 ) ) ;
#21905 = CARTESIAN_POINT ( 'NONE',  ( 209.5564680870925258, 38.04208312189877006, 12.07105558346621343 ) ) ;
#21906 = CARTESIAN_POINT ( 'NONE',  ( -46.98109279403942651, -283.9296925360795854, -195.9317964296643879 ) ) ;
#21907 = LINE ( 'NONE', #28544, #30080 ) ;
#21908 = CARTESIAN_POINT ( 'NONE',  ( -1.047045556708394054, -291.3402470497297259, -206.5513545429250826 ) ) ;
#21909 = CARTESIAN_POINT ( 'NONE',  ( -97.56320844032468642, -283.2889362272579206, -226.9316606630473245 ) ) ;
#21910 = CARTESIAN_POINT ( 'NONE',  ( 209.3407208048348878, 35.73852361108345121, 14.26380412667040432 ) ) ;
#21911 = CARTESIAN_POINT ( 'NONE',  ( 208.6208076322478746, 32.98517505407394168, 13.99999999999999822 ) ) ;
#21912 = CARTESIAN_POINT ( 'NONE',  ( -6.423100804331541624, -290.4580877275811304, -202.0307377113255143 ) ) ;
#21913 = CARTESIAN_POINT ( 'NONE',  ( -81.17921619897602170, -282.1154690976378561, -332.8832359042157236 ) ) ;
#21914 = CARTESIAN_POINT ( 'NONE',  ( -13.50796996540874062, -278.3377598353536655, -340.2603431134395464 ) ) ;
#21915 = CARTESIAN_POINT ( 'NONE',  ( -70.90616520926563737, -286.8241850355483962, -201.5030363627239467 ) ) ;
#21916 = CARTESIAN_POINT ( 'NONE',  ( 21.96169243167951279, -288.1472345162380861, -312.9299755066104467 ) ) ;
#21917 = CARTESIAN_POINT ( 'NONE',  ( -110.7547565814043509, -279.9017681422110400, -276.1431078962623928 ) ) ;
#21918 = CARTESIAN_POINT ( 'NONE',  ( -85.20317312053103365, -278.5357210789944133, -325.7624850049226666 ) ) ;
#21919 = CARTESIAN_POINT ( 'NONE',  ( -111.0379955077829521, -286.7345149892592531, -256.1671586330120931 ) ) ;
#21920 = ORIENTED_EDGE ( 'NONE', *, *, #58044, .T. ) ;
#21921 = CARTESIAN_POINT ( 'NONE',  ( -111.6215059007110710, -296.6417751110072345, -249.8783965832315630 ) ) ;
#21922 = CARTESIAN_POINT ( 'NONE',  ( 36.76002388333314030, -289.6479998257419197, -279.3489597991003848 ) ) ;
#21923 = CARTESIAN_POINT ( 'NONE',  ( 197.5281361355225442, 24.90961411280150983, 12.19683234139332839 ) ) ;
#21924 = AXIS2_PLACEMENT_3D ( 'NONE', #54537, #82496, #31843 ) ;
#21925 = CARTESIAN_POINT ( 'NONE',  ( -2.659677404128715672, -288.9805209788416391, -198.2697987213421698 ) ) ;
#21926 = VERTEX_POINT ( 'NONE', #15350 ) ;
#21927 = CARTESIAN_POINT ( 'NONE',  ( 34.70298730845203039, -291.6340781659510526, -245.3818534925929953 ) ) ;
#21928 = CARTESIAN_POINT ( 'NONE',  ( 34.66943075076979852, -288.8676928704126112, -254.7052952924910301 ) ) ;
#21929 = VECTOR ( 'NONE', #92173, 1000.000000000000000 ) ;
#21930 = CARTESIAN_POINT ( 'NONE',  ( -14.01040691084398127, -282.1190220573713532, -200.0671765169583125 ) ) ;
#21931 = CARTESIAN_POINT ( 'NONE',  ( 35.39248464043736675, -289.2741619049751876, -293.7778781920334836 ) ) ;
#21932 = CARTESIAN_POINT ( 'NONE',  ( 37.62841742264924960, -289.0593618526050363, -285.6182392299298272 ) ) ;
#21933 = CARTESIAN_POINT ( 'NONE',  ( -97.51144499442702340, -285.9409997001773149, -315.1339049659738407 ) ) ;
#21934 = CARTESIAN_POINT ( 'NONE',  ( -107.5752326963193468, -278.3142554721811166, -302.0542940243235535 ) ) ;
#21935 = ORIENTED_EDGE ( 'NONE', *, *, #28991, .F. ) ;
#21936 = CARTESIAN_POINT ( 'NONE',  ( 3.429328500152924786, -292.5888866159577333, -334.0390385296740305 ) ) ;
#21937 = CARTESIAN_POINT ( 'NONE',  ( 37.98511011499103773, -281.1850234610770940, -254.3333312591005608 ) ) ;
#21938 = CARTESIAN_POINT ( 'NONE',  ( -18.98878012808116011, -276.1511814444486959, -198.3770370581977147 ) ) ;
#21939 = CARTESIAN_POINT ( 'NONE',  ( 196.6877655503061533, 293.9636489450775230, -7.999911143031724237 ) ) ;
#21940 = CARTESIAN_POINT ( 'NONE',  ( -110.4683760289727132, -287.2662352645559167, -253.7030783399848985 ) ) ;
#21941 = CARTESIAN_POINT ( 'NONE',  ( -69.67987507718078177, -271.8721873071249320, -201.5848681080314577 ) ) ;
#21942 = CARTESIAN_POINT ( 'NONE',  ( 175.2296996224750103, 275.0000000000000568, 0.000000000000000000 ) ) ;
#21943 = CARTESIAN_POINT ( 'NONE',  ( -107.6758518614634994, -278.3215429566780017, -250.5386277043601808 ) ) ;
#21944 = CARTESIAN_POINT ( 'NONE',  ( -6.719263047997801941, -277.8640867952962594, -340.5912196087805910 ) ) ;
#21945 = CARTESIAN_POINT ( 'NONE',  ( -37.16628714595570671, -299.4796723730357257, -196.7689696390240215 ) ) ;
#21946 = CARTESIAN_POINT ( 'NONE',  ( -111.6502332804678872, -283.3684833516811068, -289.6762363067020374 ) ) ;
#21947 = CARTESIAN_POINT ( 'NONE',  ( -98.16910604117829564, -291.7325559568712379, -312.5497204895880827 ) ) ;
#21948 = CARTESIAN_POINT ( 'NONE',  ( -96.81822016697913114, -298.7187174500181186, -222.5568156675638249 ) ) ;
#21949 = CARTESIAN_POINT ( 'NONE',  ( -112.9998085514543362, -297.9090507434886490, -258.2837793831055819 ) ) ;
#21950 = CARTESIAN_POINT ( 'NONE',  ( 32.30085678040687469, -295.9111951916754606, -297.8881008007910509 ) ) ;
#21951 = CARTESIAN_POINT ( 'NONE',  ( -56.82003616209836849, -281.3037452256640449, -342.6149957259304983 ) ) ;
#21952 = CARTESIAN_POINT ( 'NONE',  ( -114.3690162180213434, -290.2080735928898321, -271.2242829903925099 ) ) ;
#21953 = CARTESIAN_POINT ( 'NONE',  ( -35.32108957620051370, -272.0977164895359124, -195.7308805423097056 ) ) ;
#21954 = CARTESIAN_POINT ( 'NONE',  ( -64.28360000871253987, -287.3065295211272314, -199.0689474654559206 ) ) ;
#21955 = CARTESIAN_POINT ( 'NONE',  ( -92.65396864172502944, -288.7887316762374326, -318.5491472107341338 ) ) ;
#21956 = CARTESIAN_POINT ( 'NONE',  ( -62.24311029045266253, -183.5800764965874521, -362.2538417114638492 ) ) ;
#21957 = VERTEX_POINT ( 'NONE', #28177 ) ;
#21958 = CARTESIAN_POINT ( 'NONE',  ( -92.37500651719146560, -289.8588878371484157, -217.2769819469097001 ) ) ;
#21959 = CARTESIAN_POINT ( 'NONE',  ( -13.28491122373756639, -288.3976034221225291, -339.3057217913893737 ) ) ;
#21960 = ORIENTED_EDGE ( 'NONE', *, *, #54119, .F. ) ;
#21961 = CARTESIAN_POINT ( 'NONE',  ( -95.59082690957457373, -286.3083017322741739, -220.3962678645182223 ) ) ;
#21962 = CARTESIAN_POINT ( 'NONE',  ( -3.853989628314376858, -276.9308503817231326, -335.2507221756457625 ) ) ;
#21963 = CARTESIAN_POINT ( 'NONE',  ( 38.02402953234110328, -292.2942411240479714, -256.1660729583650777 ) ) ;
#21964 = CARTESIAN_POINT ( 'NONE',  ( -33.05612389545042618, -283.6509437124044553, -347.1527912793576434 ) ) ;
#21965 = ADVANCED_FACE ( 'NONE', ( #21520 ), #73117, .F. ) ;
#21966 = CARTESIAN_POINT ( 'NONE',  ( -33.07795995679678214, -284.5195121670786307, -346.5615894048157202 ) ) ;
#21967 = CARTESIAN_POINT ( 'NONE',  ( -101.3991883220381709, -284.3223244763121329, -313.1461265848306539 ) ) ;
#21968 = CARTESIAN_POINT ( 'NONE',  ( 35.54070384599518917, -281.8261008851792440, -265.8619316496205442 ) ) ;
#21969 = CARTESIAN_POINT ( 'NONE',  ( 190.0322693938271925, 271.3142028313234277, -139.6664869709919969 ) ) ;
#21970 = CARTESIAN_POINT ( 'NONE',  ( -114.3576356501603613, -272.6364962766734834, -270.3621918850458883 ) ) ;
#21971 = CARTESIAN_POINT ( 'NONE',  ( 4.795094255471728850, -58.70174775560354874, -351.2244798983953160 ) ) ;
#21972 = CARTESIAN_POINT ( 'NONE',  ( -36.72445948530067739, -273.2572677171451687, -197.1898020014760391 ) ) ;
#21973 = CARTESIAN_POINT ( 'NONE',  ( -32.02302797092954023, -294.4944296402143209, -347.1287665616297318 ) ) ;
#21974 = CARTESIAN_POINT ( 'NONE',  ( -38.10613583871115395, -140.5925546180554306, -361.3186870867007201 ) ) ;
#21975 = CARTESIAN_POINT ( 'NONE',  ( -41.15134768539596166, -272.6901124389207212, -193.8972504864477457 ) ) ;
#21976 = CARTESIAN_POINT ( 'NONE',  ( -111.6105399639294262, -298.4337476957007311, -268.7289868583806083 ) ) ;
#21977 = CARTESIAN_POINT ( 'NONE',  ( -15.69048711159072518, -290.0813920908785235, -340.6458390684238111 ) ) ;
#21978 = EDGE_LOOP ( 'NONE', ( #78101, #67174, #65868 ) ) ;
#21979 = CARTESIAN_POINT ( 'NONE',  ( -65.50597995382588579, -296.3527593804980711, -341.7867340172563786 ) ) ;
#21980 = CARTESIAN_POINT ( 'NONE',  ( -17.16089001868551378, -286.8120092155866701, -200.0891174969902124 ) ) ;
#21981 = CARTESIAN_POINT ( 'NONE',  ( -66.09850452020098999, -272.6048492024476104, -199.2517268216630555 ) ) ;
#21982 = CARTESIAN_POINT ( 'NONE',  ( 30.76395526835187155, -294.8149432394591827, -305.9388992938806382 ) ) ;
#21983 = CARTESIAN_POINT ( 'NONE',  ( 17.52206569711325201, -294.7862885207600812, -324.3766276341613093 ) ) ;
#21984 = CARTESIAN_POINT ( 'NONE',  ( -109.4187653402672566, -290.5651503373185847, -282.0111010213127543 ) ) ;
#21985 = EDGE_LOOP ( 'NONE', ( #35558, #87329, #78928, #11679, #84705 ) ) ;
#21986 = CARTESIAN_POINT ( 'NONE',  ( -98.41780915115799644, -275.0749542572610835, -225.7881107299815540 ) ) ;
#21987 = CARTESIAN_POINT ( 'NONE',  ( 36.90418193689895077, -274.1099094640603084, -251.5048798565963182 ) ) ;
#21988 = EDGE_CURVE ( 'NONE', #76803, #59473, #41112, .T. ) ;
#21989 = EDGE_LOOP ( 'NONE', ( #4904, #67175, #12001, #84021 ) ) ;
#21990 = CARTESIAN_POINT ( 'NONE',  ( -110.6099939170696729, -277.7624205208140893, -294.0121355127848801 ) ) ;
#21991 = CARTESIAN_POINT ( 'NONE',  ( 29.82248366146323093, -273.5426821367229309, -239.6529016023408474 ) ) ;
#21992 = CARTESIAN_POINT ( 'NONE',  ( -109.8907022209534432, -273.7747057093094440, -259.4843535055481425 ) ) ;
#21993 = CARTESIAN_POINT ( 'NONE',  ( 9.626830515565528046, -275.6579096443498429, -214.1042775299272023 ) ) ;
#21994 = CARTESIAN_POINT ( 'NONE',  ( -104.7209098712788062, -274.7727698912561891, -235.1187653583429267 ) ) ;
#21995 = EDGE_CURVE ( 'NONE', #35701, #42443, #74828, .T. ) ;
#21996 = CARTESIAN_POINT ( 'NONE',  ( 34.48702409058480356, -273.8648720569635771, -293.1435932646288052 ) ) ;
#21997 = CARTESIAN_POINT ( 'NONE',  ( -53.16336738562419129, -295.9116935886879673, -341.7824076697121995 ) ) ;
#21998 = CARTESIAN_POINT ( 'NONE',  ( -28.10036709552414891, -294.1692172851983287, -195.7123010753824417 ) ) ;
#21999 = CARTESIAN_POINT ( 'NONE',  ( 35.06618330939426187, -291.9541002186154515, -257.1580441115829672 ) ) ;
#22000 = CARTESIAN_POINT ( 'NONE',  ( 169.2494399300530290, 8.542400036368780647, 10.00000000000000000 ) ) ;
#22001 = CARTESIAN_POINT ( 'NONE',  ( -107.3657186184687049, -279.4537168240839264, -238.3555003850097762 ) ) ;
#22002 = CARTESIAN_POINT ( 'NONE',  ( 35.58685022111462359, -275.6631082466149110, -266.1368552448271316 ) ) ;
#22003 = CIRCLE ( 'NONE', #56760, 4.025000000000000355 ) ;
#22004 = CARTESIAN_POINT ( 'NONE',  ( -98.93717572235878777, -283.8447771984256747, -224.8945107096624554 ) ) ;
#22005 = CARTESIAN_POINT ( 'NONE',  ( -109.0714872958044452, -298.8435117787939248, -247.7191634588921545 ) ) ;
#22006 = CARTESIAN_POINT ( 'NONE',  ( 73.43068321062709458, -178.2391364535880882, 0.000000000000000000 ) ) ;
#22007 = CARTESIAN_POINT ( 'NONE',  ( 7.032963811566120604, -285.8709348744963563, -212.1293195123068642 ) ) ;
#22008 = CARTESIAN_POINT ( 'NONE',  ( -111.1810247554213618, -276.7168675514026859, -276.1359333804008998 ) ) ;
#22009 = CARTESIAN_POINT ( 'NONE',  ( -97.37683044680099442, -276.5371545943185652, -312.9407125811584365 ) ) ;
#22010 = CARTESIAN_POINT ( 'NONE',  ( -111.9026023280103743, -286.6622385385496727, -261.8000237563322798 ) ) ;
#22011 = CARTESIAN_POINT ( 'NONE',  ( -13.64274970330133385, -277.9427708373137307, -339.8802981559256864 ) ) ;
#22012 = CARTESIAN_POINT ( 'NONE',  ( 156.1711927057164644, 20.00000000000000000, 14.66327707481057629 ) ) ;
#22013 = CARTESIAN_POINT ( 'NONE',  ( 27.82902674743269955, -273.4300503527801425, -230.7732843994919278 ) ) ;
#22014 = CARTESIAN_POINT ( 'NONE',  ( -5.270814052453546950, -275.1371349643871440, -204.6559447509872598 ) ) ;
#22015 = CARTESIAN_POINT ( 'NONE',  ( -25.70513905364731500, -282.2002419138664209, -196.1006381123897881 ) ) ;
#22016 = DIRECTION ( 'NONE',  ( 0.000000000000000000, 0.000000000000000000, -1.000000000000000000 ) ) ;
#22017 = CARTESIAN_POINT ( 'NONE',  ( 7.107540306442703404, -290.3725985241591729, -331.5286751730623109 ) ) ;
#22018 = CARTESIAN_POINT ( 'NONE',  ( -15.38973508845747418, -290.3360127033584490, -198.5919381762314799 ) ) ;
#22019 = CARTESIAN_POINT ( 'NONE',  ( 82.17294390126060932, -297.6627425910190823, -196.0436438549623972 ) ) ;
#22020 = CARTESIAN_POINT ( 'NONE',  ( -92.37641378831345662, -271.9282414246493431, -221.6535849807605416 ) ) ;
#22021 = CARTESIAN_POINT ( 'NONE',  ( -109.6248522415808111, -288.9118388446353265, -253.3938847739868265 ) ) ;
#22022 = CARTESIAN_POINT ( 'NONE',  ( -96.12512592106646991, -239.9971452530988358, -342.0757611934672582 ) ) ;
#22023 = CARTESIAN_POINT ( 'NONE',  ( -63.76076227538455754, -295.7076995178259722, -200.1133488993579306 ) ) ;
#22024 = CARTESIAN_POINT ( 'NONE',  ( -95.87181665151224763, -288.3670067755102195, -319.3398762303747276 ) ) ;
#22025 = CARTESIAN_POINT ( 'NONE',  ( 14.50101288419562451, -283.9084437342924616, -322.9571185482197961 ) ) ;
#22026 = CARTESIAN_POINT ( 'NONE',  ( -75.57718084624754340, -283.7896530176758461, -204.6345468768586215 ) ) ;
#22027 = CARTESIAN_POINT ( 'NONE',  ( -69.24835110941772598, -284.9056381947443697, -336.6874766743412692 ) ) ;
#22028 = CARTESIAN_POINT ( 'NONE',  ( -91.77836989261311373, -284.6567485394690493, -319.2599281127729682 ) ) ;
#22029 = CARTESIAN_POINT ( 'NONE',  ( -87.57225847614320458, -293.3348882185210869, -214.1890803815650486 ) ) ;
#22030 = CARTESIAN_POINT ( 'NONE',  ( 26.12473061240615735, -275.3100814072876688, -226.7745094584619778 ) ) ;
#22031 = CARTESIAN_POINT ( 'NONE',  ( -96.32387468291227606, -289.2767128729589672, -223.1338240985211598 ) ) ;
#22032 = CARTESIAN_POINT ( 'NONE',  ( -42.80616938195925059, -277.1193197404836042, -347.1669743723785473 ) ) ;
#22033 = CARTESIAN_POINT ( 'NONE',  ( -3.570450188973522287, -296.5841228840620261, -336.9438156009522913 ) ) ;
#22034 = CARTESIAN_POINT ( 'NONE',  ( -48.18343439339133027, -276.2535042660555860, -436.4286699060131696 ) ) ;
#22035 = CARTESIAN_POINT ( 'NONE',  ( -110.4542110544635705, -292.8376638359844719, -287.0812184334320705 ) ) ;
#22036 = CARTESIAN_POINT ( 'NONE',  ( -3.408475872029683273, -281.2791896537789285, -335.5655513260788894 ) ) ;
#22037 = CARTESIAN_POINT ( 'NONE',  ( -110.6088843885063966, -276.7671167839473583, -253.5698064723128198 ) ) ;
#22038 = CARTESIAN_POINT ( 'NONE',  ( -107.4329089919810087, -271.4213121827540931, -240.0625193506001267 ) ) ;
#22039 = CARTESIAN_POINT ( 'NONE',  ( 19.25525026875159185, -275.5551475449715895, -316.6483004899915272 ) ) ;
#22040 = CARTESIAN_POINT ( 'NONE',  ( -47.10530543855251295, -293.4460041974173237, -197.3174340477686428 ) ) ;
#22041 = CARTESIAN_POINT ( 'NONE',  ( 35.13889872392667968, -294.3555155387959417, -259.8744007521112280 ) ) ;
#22042 = CARTESIAN_POINT ( 'NONE',  ( 38.65307184076674218, -295.0839210904373431, -278.8115329236394473 ) ) ;
#22043 = CARTESIAN_POINT ( 'NONE',  ( 33.99688223763389061, -294.5132154905840025, -242.5723492517441002 ) ) ;
#22044 = CARTESIAN_POINT ( 'NONE',  ( -70.93268884922579787, -295.3415863591967536, -335.1874892885591066 ) ) ;
#22045 = CARTESIAN_POINT ( 'NONE',  ( -45.55689817865564351, -291.1564417862485925, -344.9098347303642527 ) ) ;
#22046 = CARTESIAN_POINT ( 'NONE',  ( -21.72391478033941681, -283.0239529526014053, -345.7606192097987901 ) ) ;
#22047 = CARTESIAN_POINT ( 'NONE',  ( -29.93567114496962134, -272.2845364145052258, -194.9591537205789109 ) ) ;
#22048 = CARTESIAN_POINT ( 'NONE',  ( 30.13258433355151666, -286.9037822666161901, -233.1530278623632739 ) ) ;
#22049 = CARTESIAN_POINT ( 'NONE',  ( -69.94762602334739654, -279.4635573971074223, -337.5221219412450182 ) ) ;
#22050 = EDGE_CURVE ( 'NONE', #13346, #59473, #9429, .T. ) ;
#22051 = CARTESIAN_POINT ( 'NONE',  ( -74.91024307277865546, -284.3346417672588586, -207.3076875773342351 ) ) ;
#22052 = CARTESIAN_POINT ( 'NONE',  ( -37.52300738869169550, -287.0542291604591014, -345.3736350570965215 ) ) ;
#22053 = CARTESIAN_POINT ( 'NONE',  ( -74.38302801447568413, -277.7045581109323962, -204.2684140755524425 ) ) ;
#22054 = CARTESIAN_POINT ( 'NONE',  ( 24.80950920047307307, -22.49099280560490399, -345.4124233396505019 ) ) ;
#22055 = CARTESIAN_POINT ( 'NONE',  ( -99.65853333932143698, -284.5860523897389953, -232.1255109798987348 ) ) ;
#22056 = CARTESIAN_POINT ( 'NONE',  ( 22.55518240935465712, -282.1143248949463782, -222.5870271099866500 ) ) ;
#22057 = CARTESIAN_POINT ( 'NONE',  ( 7.786474974902612978, -287.5116530156381032, -332.5255180798272931 ) ) ;
#22058 = CARTESIAN_POINT ( 'NONE',  ( -112.2139773211968929, -280.3321424147909511, -256.1285220388277253 ) ) ;
#22059 = CARTESIAN_POINT ( 'NONE',  ( -95.76171409509073840, -279.1972377115771451, -319.7817401263760075 ) ) ;
#22060 = CARTESIAN_POINT ( 'NONE',  ( -27.55627358187902942, -280.0131043519170930, -197.9687530606426833 ) ) ;
#22061 = CARTESIAN_POINT ( 'NONE',  ( -90.42928514432774989, -275.2758126436453949, -217.8867897925246098 ) ) ;
#22062 = CARTESIAN_POINT ( 'NONE',  ( 28.05235832175989330, -293.0192288351423713, -229.6079759649919367 ) ) ;
#22063 = CARTESIAN_POINT ( 'NONE',  ( 29.69408463706439250, -286.0072294040658107, -303.1947952131019406 ) ) ;
#22064 = TOROIDAL_SURFACE ( 'NONE', #56829, 24.50000000000000000, 0.5000000000000000000 ) ;
#22065 = CARTESIAN_POINT ( 'NONE',  ( -44.83882950444907323, -293.5590148283880580, -194.4784513648361894 ) ) ;
#22066 = CARTESIAN_POINT ( 'NONE',  ( -82.56124162891731544, -294.6066306310773371, -328.1269677451817302 ) ) ;
#22067 = CARTESIAN_POINT ( 'NONE',  ( 35.72912095381111186, -293.2241855123219807, -270.7642741458744808 ) ) ;
#22068 = CARTESIAN_POINT ( 'NONE',  ( -99.78737868035983638, -292.2238421941131605, -225.8411253914347583 ) ) ;
#22069 = CARTESIAN_POINT ( 'NONE',  ( 33.42427542132536900, -282.4458356901552634, -288.7431960585911952 ) ) ;
#22070 = CARTESIAN_POINT ( 'NONE',  ( -35.82189367916155476, -296.9910956121629511, -193.6704985816411408 ) ) ;
#22071 = CARTESIAN_POINT ( 'NONE',  ( -5.660901615161487044, -289.2977413021542930, -340.4299398119526359 ) ) ;
#22072 = CARTESIAN_POINT ( 'NONE',  ( -49.91227963785794230, -281.3503251986054465, -345.1288282643165530 ) ) ;
#22073 = CARTESIAN_POINT ( 'NONE',  ( 5.549062532552957450, -288.8216608659247981, -334.2839368334825281 ) ) ;
#22074 = CARTESIAN_POINT ( 'NONE',  ( -38.62953629823759627, -286.3688797193307209, -197.3388459742041050 ) ) ;
#22075 = DIRECTION ( 'NONE',  ( 0.8571673007021122226, 0.000000000000000000, 0.5150380749100541555 ) ) ;
#22076 = CARTESIAN_POINT ( 'NONE',  ( -108.0872568736431276, -260.2256227728311160, -316.3845286481523544 ) ) ;
#22077 = CARTESIAN_POINT ( 'NONE',  ( -105.4589550887750988, -260.1083542854994448, -315.4719013409242052 ) ) ;
#22078 = CARTESIAN_POINT ( 'NONE',  ( -57.14712512772582897, -278.9871598176096086, -199.9313879881560183 ) ) ;
#22079 = CARTESIAN_POINT ( 'NONE',  ( -79.22023687147216719, -278.3923204521280468, -210.1912398614051085 ) ) ;
#22080 = CARTESIAN_POINT ( 'NONE',  ( 7.226205466581010484, -274.3075671297090139, -207.5306920235136658 ) ) ;
#22081 = CARTESIAN_POINT ( 'NONE',  ( -104.6257879195275109, -262.2290025098591855, -316.4541994228543444 ) ) ;
#22082 = CARTESIAN_POINT ( 'NONE',  ( -110.7659831213586301, -277.3941555624001012, -249.2073722050611195 ) ) ;
#22083 = CARTESIAN_POINT ( 'NONE',  ( -38.94513464922362544, -281.0924407706675083, -345.0014707077602907 ) ) ;
#22084 = CARTESIAN_POINT ( 'NONE',  ( -41.86256625807790499, -296.8683808095737504, -346.2648876686359358 ) ) ;
#22085 = CARTESIAN_POINT ( 'NONE',  ( -95.16693801237609307, -291.6726911288322412, -225.7043121688516010 ) ) ;
#22086 = CARTESIAN_POINT ( 'NONE',  ( -96.17309108007361829, -288.6226318876221626, -314.4288160037789339 ) ) ;
#22087 = CARTESIAN_POINT ( 'NONE',  ( 11.71427823649671573, -275.3638067033971311, -211.0734894895038565 ) ) ;
#22088 = CARTESIAN_POINT ( 'NONE',  ( -98.73215289570036646, -296.1710757018130380, -309.9532392955114233 ) ) ;
#22089 = ORIENTED_EDGE ( 'NONE', *, *, #83847, .T. ) ;
#22090 = CARTESIAN_POINT ( 'NONE',  ( 193.9646936176702070, 20.00000000000000000, 15.00000000000000000 ) ) ;
#22091 = CARTESIAN_POINT ( 'NONE',  ( 196.9879731654527006, 24.91455852016545691, 12.95191548363261447 ) ) ;
#22092 = CARTESIAN_POINT ( 'NONE',  ( -108.2632307133195297, -280.8097462131869406, -244.1436519893845229 ) ) ;
#22093 = CARTESIAN_POINT ( 'NONE',  ( -43.79193168206481346, -281.0485387096636600, -197.2858770015112668 ) ) ;
#22094 = CARTESIAN_POINT ( 'NONE',  ( -88.26912268362117686, -281.1104411273269648, -213.9663341499709190 ) ) ;
#22095 = CARTESIAN_POINT ( 'NONE',  ( 17.77405764104748798, -281.2967919033375779, -318.5862327476772862 ) ) ;
#22096 = CARTESIAN_POINT ( 'NONE',  ( -35.35239066189981827, -272.5574123695898834, -196.6820132493316464 ) ) ;
#22097 = DIRECTION ( 'NONE',  ( -1.000000000000000000, 0.000000000000000000, -0.000000000000000000 ) ) ;
#22098 = CARTESIAN_POINT ( 'NONE',  ( 203.5977283565847813, 62.01285785379744198, -7.000000000000000888 ) ) ;
#22099 = CARTESIAN_POINT ( 'NONE',  ( 38.05831960672234970, -276.1695162504791483, -255.5626097816515596 ) ) ;
#22100 = ADVANCED_FACE ( 'NONE', ( #86369 ), #71262, .T. ) ;
#22101 = DIRECTION ( 'NONE',  ( -0.000000000000000000, 1.000000000000000000, -0.000000000000000000 ) ) ;
#22102 = CARTESIAN_POINT ( 'NONE',  ( 22.85890001193301657, -276.9416516776275898, -225.6298269853682825 ) ) ;
#22103 = CARTESIAN_POINT ( 'NONE',  ( -75.06125039791029963, -276.1192420736601889, -336.8129187151195083 ) ) ;
#22104 = DIRECTION ( 'NONE',  ( 0.000000000000000000, 0.000000000000000000, -1.000000000000000000 ) ) ;
#22105 = CARTESIAN_POINT ( 'NONE',  ( -87.21367931486913960, -285.7225291876022766, -326.9214104897814650 ) ) ;
#22106 = CARTESIAN_POINT ( 'NONE',  ( 16.86468766532961183, -292.0461569398232768, -221.1515885977380549 ) ) ;
#22107 = EDGE_CURVE ( 'NONE', #6460, #25984, #88030, .T. ) ;
#22108 = CARTESIAN_POINT ( 'NONE',  ( 2.695029425714173144, -285.9229736202519234, -204.7076864414023873 ) ) ;
#22109 = CARTESIAN_POINT ( 'NONE',  ( -89.62578124426643456, -282.0411623410666948, -322.8196108243830622 ) ) ;
#22110 = CARTESIAN_POINT ( 'NONE',  ( -26.67516214311025280, -281.4886774185390550, -343.2249162273571415 ) ) ;
#22111 = CARTESIAN_POINT ( 'NONE',  ( -23.97822540288576576, -284.0827161764458424, -342.5313891958876980 ) ) ;
#22112 = CARTESIAN_POINT ( 'NONE',  ( -32.77816706851746176, -272.1094782177806337, -195.4872723704287978 ) ) ;
#22113 = CARTESIAN_POINT ( 'NONE',  ( -110.9431073469294802, -283.2039273498729699, -250.4329958359720649 ) ) ;
#22114 = CARTESIAN_POINT ( 'NONE',  ( -30.74092480879376765, -296.9688542094201580, -345.0700894240405319 ) ) ;
#22115 = CARTESIAN_POINT ( 'NONE',  ( -89.65000708968557319, -280.2336095024909355, -219.0325341674079596 ) ) ;
#22116 = CARTESIAN_POINT ( 'NONE',  ( -13.31443234037744183, -288.3636626828387648, -199.1380962288147884 ) ) ;
#22117 = CARTESIAN_POINT ( 'NONE',  ( 198.9668273763369370, 289.1149190245543537, -6.365503232778033649 ) ) ;
#22118 = DIRECTION ( 'NONE',  ( -0.000000000000000000, 0.000000000000000000, -1.000000000000000000 ) ) ;
#22119 = CARTESIAN_POINT ( 'NONE',  ( 21.18703404804402979, -296.1261458901512924, -318.1695276976710147 ) ) ;
#22120=STYLED_ITEM('',(#93766),#91539);
#22121 = CARTESIAN_POINT ( 'NONE',  ( -109.7578302270225663, -276.3010762859791498, -289.8778992926926890 ) ) ;
#22122 = CARTESIAN_POINT ( 'NONE',  ( 20.44469823219483118, -287.4361421746965561, -321.0256893788560433 ) ) ;
#22123 = CARTESIAN_POINT ( 'NONE',  ( 32.28813893876350960, -292.2756925488212119, -294.9706231266723080 ) ) ;
#22124 = CARTESIAN_POINT ( 'NONE',  ( -41.90381846841076197, -275.7956293297857542, -343.7252176699694246 ) ) ;
#22125 = CARTESIAN_POINT ( 'NONE',  ( -94.04089835848893131, -294.0219229490073189, -318.2981056590870708 ) ) ;
#22126 = CARTESIAN_POINT ( 'NONE',  ( -100.1416392193741558, -292.3895593927554160, -232.1850636094812046 ) ) ;
#22127 = CARTESIAN_POINT ( 'NONE',  ( -37.30987171927208124, -285.5519495502701943, -345.3611179825600175 ) ) ;
#22128 = CARTESIAN_POINT ( 'NONE',  ( -2.303234979380001768, -293.0768387492785223, -338.1476484627474406 ) ) ;
#22129 = CARTESIAN_POINT ( 'NONE',  ( -99.50476808335670853, -291.6080240857183981, -310.1379126885870505 ) ) ;
#22130 = CARTESIAN_POINT ( 'NONE',  ( -111.3254551891057247, -289.0116684509216611, -253.0297012861432790 ) ) ;
#22131 = CARTESIAN_POINT ( 'NONE',  ( -26.36925067790773625, -290.3352001329694190, -343.1791956797229091 ) ) ;
#22132 = DIRECTION ( 'NONE',  ( -0.000000000000000000, -1.000000000000000000, -0.000000000000000000 ) ) ;
#22133 = CARTESIAN_POINT ( 'NONE',  ( -95.07168560295637860, -290.7229380147977054, -315.3241013266531922 ) ) ;
#22134 = FACE_OUTER_BOUND ( 'NONE', #27505, .T. ) ;
#22135 = CARTESIAN_POINT ( 'NONE',  ( -51.59629486533960119, -290.4356736415537625, -345.6260849087109364 ) ) ;
#22136 = CARTESIAN_POINT ( 'NONE',  ( -110.1354556039400592, -276.8220739507396502, -250.8312221900138468 ) ) ;
#22137 = CARTESIAN_POINT ( 'NONE',  ( -103.3956343133897917, -279.4021852757245483, -230.7274491460136687 ) ) ;
#22138 = CARTESIAN_POINT ( 'NONE',  ( 35.30914228429821122, -280.8960175089619611, -244.7539119773361165 ) ) ;
#22139 = CARTESIAN_POINT ( 'NONE',  ( 30.63307416003257089, -285.1354721084101698, -238.6683631933582035 ) ) ;
#22140 = CARTESIAN_POINT ( 'NONE',  ( 196.3782803251243649, 41.22862212338403509, 11.42719184255257225 ) ) ;
#22141 = CARTESIAN_POINT ( 'NONE',  ( -3.071879666528419595, -280.7340358851059250, -336.2270467589209488 ) ) ;
#22142 = CARTESIAN_POINT ( 'NONE',  ( -106.0825702173391818, -282.9460941949111543, -240.2364737273184119 ) ) ;
#22143 = CARTESIAN_POINT ( 'NONE',  ( 206.1702601134498991, 0.9999999999999995559, 7.166232077703399206 ) ) ;
#22144 = CARTESIAN_POINT ( 'NONE',  ( -104.3758221352403126, -276.5559851423716964, -306.8184113241194382 ) ) ;
#22145 = CARTESIAN_POINT ( 'NONE',  ( -111.9217889233537875, -283.2474106860418601, -288.2857971699683048 ) ) ;
#22146 = CARTESIAN_POINT ( 'NONE',  ( -103.3551642575919516, -273.7806015108240558, -238.8202828630230101 ) ) ;
#22147 = CARTESIAN_POINT ( 'NONE',  ( -106.4670620156734060, -292.4950863085143737, -244.3678915975998507 ) ) ;
#22148 = CARTESIAN_POINT ( 'NONE',  ( -93.72285049825497083, -274.6844223999264614, -218.7688147723552277 ) ) ;
#22149 = CARTESIAN_POINT ( 'NONE',  ( 34.14291645092834671, -275.0215539068581734, -255.3991503462194146 ) ) ;
#22150 = CARTESIAN_POINT ( 'NONE',  ( -96.33113357565775914, -297.9165606087130413, -316.6779334472983578 ) ) ;
#22151 = CARTESIAN_POINT ( 'NONE',  ( -9.561351126600849071, -288.8656785706443202, -342.1751292468177326 ) ) ;
#22152 = CARTESIAN_POINT ( 'NONE',  ( 36.58107147869814213, -279.4318331750414472, -254.6550208814402652 ) ) ;
#22153 = CARTESIAN_POINT ( 'NONE',  ( 30.89990797362019848, -292.9240255349965310, -234.5800561597016838 ) ) ;
#22154 = CARTESIAN_POINT ( 'NONE',  ( -38.89057644368904221, -291.0909937490118295, -197.1422035480904640 ) ) ;
#22155 = CARTESIAN_POINT ( 'NONE',  ( 9.917788682466211370, -292.4014632694477882, -328.6649678520193447 ) ) ;
#22156 = ORIENTED_EDGE ( 'NONE', *, *, #57669, .T. ) ;
#22157 = CARTESIAN_POINT ( 'NONE',  ( 198.7993789751180316, 65.26489576793395031, 10.60649040369606944 ) ) ;
#22158 = CARTESIAN_POINT ( 'NONE',  ( -107.8095829145748326, -290.3145046411170256, -251.0669235867877944 ) ) ;
#22159 = CARTESIAN_POINT ( 'NONE',  ( 208.3931580544659710, 28.69469092964787293, 12.02378101520651299 ) ) ;
#22160 = CARTESIAN_POINT ( 'NONE',  ( -35.16695040813171147, -287.0200468475034654, -193.6141193639876974 ) ) ;
#22161 = CARTESIAN_POINT ( 'NONE',  ( -82.08285599513421005, -276.9094976428775681, -214.2051214447836571 ) ) ;
#22162 = CARTESIAN_POINT ( 'NONE',  ( 19.34779862607356193, -293.3174921773381811, -322.1987546065767560 ) ) ;
#22163 = CARTESIAN_POINT ( 'NONE',  ( -90.08595395822472085, -285.0937366283082497, -325.8534319123103842 ) ) ;
#22164 = CARTESIAN_POINT ( 'NONE',  ( -46.72276634727607103, -285.7631942962228777, -197.9156218335947415 ) ) ;
#22165 = CARTESIAN_POINT ( 'NONE',  ( 18.84951794254120117, -277.7437967066101692, -318.0397795173426516 ) ) ;
#22166 = CARTESIAN_POINT ( 'NONE',  ( 35.37206869002721987, -291.7905415748623454, -287.2860912335888202 ) ) ;
#22167 = CARTESIAN_POINT ( 'NONE',  ( -36.96823175198149869, -296.8075223592193197, -344.3861095276251945 ) ) ;
#22168 = CARTESIAN_POINT ( 'NONE',  ( 24.30962165790098695, -274.8965906410148818, -310.2824929164183914 ) ) ;
#22169 = ORIENTED_EDGE ( 'NONE', *, *, #54639, .T. ) ;
#22170 = CARTESIAN_POINT ( 'NONE',  ( 188.7399167944524550, -12.49482340714361506, 10.00000000000000000 ) ) ;
#22171 = CARTESIAN_POINT ( 'NONE',  ( -37.69314251029897633, -294.7231250274949161, -347.3522466207692219 ) ) ;
#22172 = CARTESIAN_POINT ( 'NONE',  ( 35.98156636610907810, -289.3023750589509291, -257.2251602155025125 ) ) ;
#22173 = CARTESIAN_POINT ( 'NONE',  ( -83.98625600570882455, -296.7554854291993820, -331.3031652977419981 ) ) ;
#22174 = CARTESIAN_POINT ( 'NONE',  ( -17.15167285799614660, -286.9710496297568625, -200.0497078762374201 ) ) ;
#22175 = CARTESIAN_POINT ( 'NONE',  ( -89.06245291972591360, -276.8173499521330427, -327.0866320221732622 ) ) ;
#22176 = CARTESIAN_POINT ( 'NONE',  ( -69.47775345365398891, -296.1154793590793588, -340.2367282493395919 ) ) ;
#22177 = CARTESIAN_POINT ( 'NONE',  ( -37.52280776917235983, -287.1939510637074022, -346.1385669946510006 ) ) ;
#22178 = CARTESIAN_POINT ( 'NONE',  ( -112.5835933026689304, -296.6820164107526807, -286.6215547280542637 ) ) ;
#22179 = CARTESIAN_POINT ( 'NONE',  ( -49.69647704797255017, -292.2236489684635785, -198.3414022905857905 ) ) ;
#22180 = CARTESIAN_POINT ( 'NONE',  ( 157.7374095173865385, 14.19731191252289015, 13.00000000000000178 ) ) ;
#22181 = CARTESIAN_POINT ( 'NONE',  ( -47.80257052418233599, -229.5268262511776527, 25.50000000000000000 ) ) ;
#22182 = CARTESIAN_POINT ( 'NONE',  ( -88.01845085740878005, -229.9137135291813365, -344.5856900491873489 ) ) ;
#22183 = CARTESIAN_POINT ( 'NONE',  ( -33.77923857464701740, -287.6163341169957448, -194.1376529509589659 ) ) ;
#22184 = CARTESIAN_POINT ( 'NONE',  ( 40.65961533371913106, -284.8380690714489560, -252.5904736702033802 ) ) ;
#22185 = ORIENTED_EDGE ( 'NONE', *, *, #83488, .T. ) ;
#22186 = CARTESIAN_POINT ( 'NONE',  ( -113.1346158339228651, -278.0634180704651612, -257.3708633454112373 ) ) ;
#22187 = CARTESIAN_POINT ( 'NONE',  ( -93.92916999590963201, -285.8714485896629185, -319.3488311274430203 ) ) ;
#22188 = CARTESIAN_POINT ( 'NONE',  ( -110.1298315720598566, -282.8318573188327036, -293.6528307703787277 ) ) ;
#22189 = CARTESIAN_POINT ( 'NONE',  ( -45.54495075267553261, -287.2367591935550877, -344.3477443156335767 ) ) ;
#22190 = CARTESIAN_POINT ( 'NONE',  ( 37.27147938519131998, -277.2443599666023601, -257.1273687462525572 ) ) ;
#22191 = CARTESIAN_POINT ( 'NONE',  ( -109.8647781493528583, -296.9224666840913187, -279.6198576391023494 ) ) ;
#22192 = CARTESIAN_POINT ( 'NONE',  ( -26.14871156161469301, -293.5914854915856154, -342.9969251574776763 ) ) ;
#22193 = CARTESIAN_POINT ( 'NONE',  ( -93.00570585509343857, -279.9305526717643602, -217.2300448862810640 ) ) ;
#22195 = CARTESIAN_POINT ( 'NONE',  ( -108.0690998730582919, -278.1449764571256651, -251.8315056525128739 ) ) ;
#22194 = CARTESIAN_POINT ( 'NONE',  ( 15.59787931475365674, -276.2767034632022387, -320.6244339139205408 ) ) ;
#22196 = CARTESIAN_POINT ( 'NONE',  ( -44.02956050058333659, -275.0492799886968101, -193.9092992939274041 ) ) ;
#22197 = CARTESIAN_POINT ( 'NONE',  ( -20.20859208524191075, -275.7574756614356488, -345.1682007661023022 ) ) ;
#22198 = CARTESIAN_POINT ( 'NONE',  ( 84.21812867662228541, 83.45443861164879706, -302.1763853416691745 ) ) ;
#22199 = CARTESIAN_POINT ( 'NONE',  ( 30.74250727900928126, -273.9665778163246159, -301.9402080428728254 ) ) ;
#22200 = CARTESIAN_POINT ( 'NONE',  ( -103.3500167102587710, -298.4832830842162252, -231.7664360560755199 ) ) ;
#22201 = CARTESIAN_POINT ( 'NONE',  ( 156.8041522122653930, 250.5000000000000568, 16.89672165344857646 ) ) ;
#22202 = LINE ( 'NONE', #79960, #68394 ) ;
#22203 = CARTESIAN_POINT ( 'NONE',  ( -14.48261541762676430, -287.4351067973700538, -200.6538171777995387 ) ) ;
#22204 = CARTESIAN_POINT ( 'NONE',  ( -60.22637820178681523, -287.5197486980457597, -197.8475513429349917 ) ) ;
#22205 = CARTESIAN_POINT ( 'NONE',  ( 17.85860097880830466, -286.2184885290956231, -222.4359739960347042 ) ) ;
#22206 = CARTESIAN_POINT ( 'NONE',  ( -96.23801573427232370, -277.5702114631654354, -225.8692096821175426 ) ) ;
#22207 = CARTESIAN_POINT ( 'NONE',  ( -96.76874868663158225, -287.0266296698727047, -225.8718902713021350 ) ) ;
#22208 = CARTESIAN_POINT ( 'NONE',  ( -108.6384978430881461, -277.2764081619799299, -251.6709374264213182 ) ) ;
#22209 = CARTESIAN_POINT ( 'NONE',  ( 3.421456510655424221, -277.8064741970088107, -331.5134567606641554 ) ) ;
#22210 = CARTESIAN_POINT ( 'NONE',  ( -2.890174278974634969, -275.0129076687061342, -205.9322361944807085 ) ) ;
#22211 = CARTESIAN_POINT ( 'NONE',  ( 37.11482357245765940, -286.5741085521617038, -288.4230053044920510 ) ) ;
#22212 = CARTESIAN_POINT ( 'NONE',  ( 36.82645904412814275, -282.1024078412224299, -250.2303356975590987 ) ) ;
#22213 = CARTESIAN_POINT ( 'NONE',  ( -8.056497279534728051, -283.1711699926710253, -341.5646719540514482 ) ) ;
#22214 = VERTEX_POINT ( 'NONE', #37125 ) ;
#22215 = EDGE_LOOP ( 'NONE', ( #69686, #82964, #67372, #46849, #21336 ) ) ;
#22216 = LINE ( 'NONE', #58223, #67039 ) ;
#22217 = CARTESIAN_POINT ( 'NONE',  ( 17.76297131009744490, -290.1341867999327064, -322.3590089598238819 ) ) ;
#22218 = CARTESIAN_POINT ( 'NONE',  ( -77.88933870526683734, -288.2692228764158813, -335.3011739738267352 ) ) ;
#22219 = CARTESIAN_POINT ( 'NONE',  ( -4.825223653120814582, -296.2311946048604909, -339.2892929830470052 ) ) ;
#22220 = CARTESIAN_POINT ( 'NONE',  ( -102.2333929932004537, -272.0727295929950742, -236.3031684576393729 ) ) ;
#22221 = EDGE_CURVE ( 'NONE', #69835, #14641, #66033, .T. ) ;
#22222 = CARTESIAN_POINT ( 'NONE',  ( 8.796404474466545054, -292.0144727706777417, -208.7756489966121478 ) ) ;
#22223 = CARTESIAN_POINT ( 'NONE',  ( 29.44641053649024443, -285.6154333585424752, -239.2153955738508841 ) ) ;
#22224 = CARTESIAN_POINT ( 'NONE',  ( -44.37448219349185052, -290.2019754038470865, -196.6311454344262870 ) ) ;
#22225 = CARTESIAN_POINT ( 'NONE',  ( 35.66780817446930740, -288.6584019714782698, -262.8283759998219580 ) ) ;
#22226 = CARTESIAN_POINT ( 'NONE',  ( 35.77081079830085031, -289.8376638359844719, -253.6410175316879361 ) ) ;
#22227 = CARTESIAN_POINT ( 'NONE',  ( 37.70171403041528890, -289.5668755362885918, -271.4949553583992383 ) ) ;
#22228 = CARTESIAN_POINT ( 'NONE',  ( -108.6826151180768392, -288.8591520862484572, -246.5234751746968129 ) ) ;
#22229 = CARTESIAN_POINT ( 'NONE',  ( -109.9721806977819227, -292.3114130144335263, -289.1150650117858731 ) ) ;
#22230 = CARTESIAN_POINT ( 'NONE',  ( -110.5534734773341938, -285.4500233752038412, -273.6606515812145517 ) ) ;
#22231 = CARTESIAN_POINT ( 'NONE',  ( -30.88085797615934780, -294.1336568521236927, -195.4211257457027102 ) ) ;
#22232 = CARTESIAN_POINT ( 'NONE',  ( 161.2494399300530290, -11.64849832608277325, 9.974999999999996092 ) ) ;
#22233 = LINE ( 'NONE', #79990, #88158 ) ;
#22234 = CARTESIAN_POINT ( 'NONE',  ( -64.33495462278260391, -275.6815556624387682, -199.9926242070763180 ) ) ;
#22235 = CARTESIAN_POINT ( 'NONE',  ( 33.47724435056878178, -280.9918250630988723, -288.7761442953181472 ) ) ;
#22236 = CARTESIAN_POINT ( 'NONE',  ( -108.9015518976414398, -282.2623234398820387, -292.8152548785163276 ) ) ;
#22237 = CARTESIAN_POINT ( 'NONE',  ( -112.4494906573325608, -295.5460865157887724, -286.5777336305656036 ) ) ;
#22238 = CARTESIAN_POINT ( 'NONE',  ( -13.72111821650113228, -272.6028334364460193, -200.2181060536160544 ) ) ;
#22239 = CARTESIAN_POINT ( 'NONE',  ( -59.64936969553718171, -275.4231879672407786, -341.3800033185805773 ) ) ;
#22240 = CARTESIAN_POINT ( 'NONE',  ( -109.0695403192397777, -297.6575303897711819, -286.3723771831532758 ) ) ;
#22241 = CARTESIAN_POINT ( 'NONE',  ( -57.23711263161519724, -285.8906705383787994, 52.50000000000000711 ) ) ;
#22242 = CARTESIAN_POINT ( 'NONE',  ( -52.41151477871648723, -272.4376632742024071, -195.3971037112025897 ) ) ;
#22243 = CARTESIAN_POINT ( 'NONE',  ( -111.6053022474380185, -294.9966496422327964, -254.2103682178892825 ) ) ;
#22244 = CARTESIAN_POINT ( 'NONE',  ( 14.74607274401700963, -295.7263747231954767, -322.4158481592006069 ) ) ;
#22245 = CARTESIAN_POINT ( 'NONE',  ( 151.9709352735115147, -299.5541904835127980, -195.3611179825600175 ) ) ;
#22246 = CARTESIAN_POINT ( 'NONE',  ( -53.17438228851172255, -296.0630885945287787, -341.8409971645655219 ) ) ;
#22247 = CARTESIAN_POINT ( 'NONE',  ( 201.8074164583845800, 62.71404347882092623, 8.782170572792690422 ) ) ;
#22249 = CARTESIAN_POINT ( 'NONE',  ( -110.2416699368873196, -296.5017565662486163, -274.1813799991211908 ) ) ;
#22248 = CARTESIAN_POINT ( 'NONE',  ( -110.9245596023432938, -282.3646367271575173, -286.6082592393852337 ) ) ;
#22250 = CARTESIAN_POINT ( 'NONE',  ( -107.0056437063501278, -284.1319971480290860, -303.1625655896975218 ) ) ;
#22251 = CARTESIAN_POINT ( 'NONE',  ( -31.71858921361257799, -284.9018791663603452, -345.7246177489112142 ) ) ;
#22252 = CARTESIAN_POINT ( 'NONE',  ( 26.34225995688074562, -286.6482913586738164, -227.0929448413731109 ) ) ;
#22253 = CARTESIAN_POINT ( 'NONE',  ( 32.54952155606841302, -291.2035751591625399, -243.6170428255205422 ) ) ;
#22254 = CARTESIAN_POINT ( 'NONE',  ( -50.90107174682299984, -279.0802838820051193, -194.7284381322464810 ) ) ;
#22255 = CARTESIAN_POINT ( 'NONE',  ( -37.37352853689063181, -274.5523547857346784, -345.3611179825600175 ) ) ;
#22256 = CARTESIAN_POINT ( 'NONE',  ( -48.18343439339133027, -263.2803689378613399, -495.2320347593685597 ) ) ;
#22257 = CARTESIAN_POINT ( 'NONE',  ( 30.84842715446182027, -286.7100404913146008, -297.6502300408513975 ) ) ;
#22259 = DIRECTION ( 'NONE',  ( 0.000000000000000000, 0.000000000000000000, 1.000000000000000000 ) ) ;
#22258 = CARTESIAN_POINT ( 'NONE',  ( -112.5674954545477533, -289.2843161470996165, -285.3465955838249215 ) ) ;
#22260 = DIRECTION ( 'NONE',  ( -0.000000000000000000, 0.000000000000000000, -1.000000000000000000 ) ) ;
#22261 = CARTESIAN_POINT ( 'NONE',  ( -109.9951378517421148, -280.2793432260988311, -246.5269591809231997 ) ) ;
#22263 = CARTESIAN_POINT ( 'NONE',  ( 21.34849923393327131, -280.6096557665269984, -226.8941514325418609 ) ) ;
#22262 = CARTESIAN_POINT ( 'NONE',  ( -100.1642185272913821, -295.1319036797182207, -228.7234769323524688 ) ) ;
#22264 = CARTESIAN_POINT ( 'NONE',  ( -50.46543365354227717, -295.3818323735723652, -346.2884284626431963 ) ) ;
#22265 = CARTESIAN_POINT ( 'NONE',  ( -112.0836304866057134, -280.4648215115045673, -277.1753842732701969 ) ) ;
#22266 = CARTESIAN_POINT ( 'NONE',  ( -108.5305625601052952, -295.3841446237775017, -287.6057295929663269 ) ) ;
#22267 = ORIENTED_EDGE ( 'NONE', *, *, #25637, .F. ) ;
#22268 = DIRECTION ( 'NONE',  ( 1.000000000000000000, 0.000000000000000000, 0.000000000000000000 ) ) ;
#22269 = CARTESIAN_POINT ( 'NONE',  ( 17.04110970482810217, -284.2525407641870174, -321.5665002404175539 ) ) ;
#22270 = DIRECTION ( 'NONE',  ( 1.000000000000000000, 0.000000000000000000, 0.000000000000000000 ) ) ;
#22271 = CARTESIAN_POINT ( 'NONE',  ( -54.42813229853333468, -295.3380690714489560, -195.3538533559490702 ) ) ;
#22272 = CARTESIAN_POINT ( 'NONE',  ( -32.68215819214907469, -273.3066127776787084, -193.6508797292545694 ) ) ;
#22273 = EDGE_CURVE ( 'NONE', #36583, #19033, #43300, .T. ) ;
#22274 = EDGE_CURVE ( 'NONE', #3784, #82379, #72922, .T. ) ;
#22275 = CARTESIAN_POINT ( 'NONE',  ( -109.4194431664759435, -290.2318440797944845, -282.0069061936464436 ) ) ;
#22276 = CARTESIAN_POINT ( 'NONE',  ( 13.80248491921587117, -282.3048035628567050, -217.2336380784568348 ) ) ;
#22277 = CARTESIAN_POINT ( 'NONE',  ( -13.82964972427402195, -275.9625615892384758, -200.4066763793818495 ) ) ;
#22278 = CARTESIAN_POINT ( 'NONE',  ( -0.7416024824666248572, -284.1745283448616419, -337.2105748063932538 ) ) ;
#22279 = CARTESIAN_POINT ( 'NONE',  ( 28.14255930824677066, -279.8980774887751295, -237.0980804190692766 ) ) ;
#22280 = CARTESIAN_POINT ( 'NONE',  ( -111.0028955777129482, -280.3702994175069989, -284.5366186649951601 ) ) ;
#22281 = CARTESIAN_POINT ( 'NONE',  ( -111.8188285338560348, -272.9658686250723463, -250.6081887865874194 ) ) ;
#22282 = CARTESIAN_POINT ( 'NONE',  ( -10.34562563149279768, -274.2280746691117770, -198.1918986989856251 ) ) ;
#22283 = CARTESIAN_POINT ( 'NONE',  ( 11.24962205036979235, -296.2928501598140656, -326.7543587482267071 ) ) ;
#22284 = CARTESIAN_POINT ( 'NONE',  ( 200.3424981855932003, 61.71662552180350758, -9.000000000000000000 ) ) ;
#22285 = DIRECTION ( 'NONE',  ( 0.000000000000000000, 0.000000000000000000, -1.000000000000000000 ) ) ;
#22286 = CARTESIAN_POINT ( 'NONE',  ( -3.797320701080445726, -292.7540198581447726, -338.3098666641859040 ) ) ;
#22287 = CARTESIAN_POINT ( 'NONE',  ( -89.28151697533074582, -272.8039718208664794, -218.9778145903534323 ) ) ;
#22288 = CARTESIAN_POINT ( 'NONE',  ( -81.54464272965081761, -292.9826929803199960, -208.1613783008386633 ) ) ;
#22290 = CARTESIAN_POINT ( 'NONE',  ( -56.10645004155875881, -293.0208695947184765, -196.0373928719101855 ) ) ;
#22289 = CARTESIAN_POINT ( 'NONE',  ( -54.42813229853333468, -285.7662352645560873, -345.3683826091709648 ) ) ;
#22291 = CARTESIAN_POINT ( 'NONE',  ( 25.79854838069763190, -290.0940410220385388, -310.5274900358434707 ) ) ;
#22292 = CARTESIAN_POINT ( 'NONE',  ( -32.32241159011101672, -274.9886833397418400, -345.0771585028429058 ) ) ;
#22293 = CARTESIAN_POINT ( 'NONE',  ( -90.08927113953996013, -279.7244101909936376, -322.9605495156383768 ) ) ;
#22294 = CARTESIAN_POINT ( 'NONE',  ( 34.50014185757092378, -291.8851133859548668, -289.9047516695094941 ) ) ;
#22295 = CARTESIAN_POINT ( 'NONE',  ( 37.45234936239019419, -283.5672578894449316, -282.5317990292687682 ) ) ;
#22296 = EDGE_LOOP ( 'NONE', ( #19386, #22406, #65534, #57974 ) ) ;
#22297 = CARTESIAN_POINT ( 'NONE',  ( -37.54484287652233121, -282.7215177141004574, -343.3944125572135704 ) ) ;
#22298 = CARTESIAN_POINT ( 'NONE',  ( -88.73452847818180089, -280.4300808660009920, -213.4377510479040723 ) ) ;
#22299 = CARTESIAN_POINT ( 'NONE',  ( -30.26692014408772025, -281.7594550964741416, -346.6366462109099871 ) ) ;
#22300 = CARTESIAN_POINT ( 'NONE',  ( -5.371805337394278013, -277.5829339913037188, -340.1518483192255644 ) ) ;
#22301 = DIRECTION ( 'NONE',  ( 0.000000000000000000, 0.000000000000000000, 1.000000000000000000 ) ) ;
#22302 = CARTESIAN_POINT ( 'NONE',  ( 22.98194438822590868, -277.7021111441856647, -317.1130944794555830 ) ) ;
#22303 = CARTESIAN_POINT ( 'NONE',  ( -92.05005921254146983, -292.4090924074130839, -314.0302885647153062 ) ) ;
#22304 = EDGE_LOOP ( 'NONE', ( #47280, #28968, #11942, #31716 ) ) ;
#22305 = CARTESIAN_POINT ( 'NONE',  ( -36.47938060747782174, -300.0631032878335418, -195.3608152725264517 ) ) ;
#22306 = CARTESIAN_POINT ( 'NONE',  ( -48.88656166690392268, -275.2198881082672983, -344.1602806372961254 ) ) ;
#22307 = CARTESIAN_POINT ( 'NONE',  ( -103.7356006400929829, -292.7977659446831353, -233.4040620059906530 ) ) ;
#22308 = CARTESIAN_POINT ( 'NONE',  ( 32.84572263011548188, -293.1712189689705497, -290.8418044885499967 ) ) ;
#22309 = CARTESIAN_POINT ( 'NONE',  ( 38.91511078874229668, -286.9319030931991392, -260.1422290020757373 ) ) ;
#22310 = DIRECTION ( 'NONE',  ( 0.000000000000000000, 0.000000000000000000, -1.000000000000000000 ) ) ;
#22312 = CARTESIAN_POINT ( 'NONE',  ( -95.76208709428401278, -282.3238120102021185, -315.4760857406908485 ) ) ;
#22311 = CARTESIAN_POINT ( 'NONE',  ( -39.11251653925135230, -293.6487009939369273, -346.7513693497926965 ) ) ;
#22313 = CARTESIAN_POINT ( 'NONE',  ( -48.21895197020887025, -291.0523013719660526, -343.8469917341868154 ) ) ;
#22314 = CARTESIAN_POINT ( 'NONE',  ( -67.81691342459275518, -284.1245942245611786, -203.2644032435040060 ) ) ;
#22315 = CARTESIAN_POINT ( 'NONE',  ( 5.895644465780362609, -283.7670468648700535, -329.7898611057781864 ) ) ;
#22316 = CARTESIAN_POINT ( 'NONE',  ( -34.66299147064142971, -289.9605083478569441, -347.0790737262552170 ) ) ;
#22317 = CARTESIAN_POINT ( 'NONE',  ( 29.02595968325211118, -281.6312435963162670, -239.6895749831276135 ) ) ;
#22318 = CARTESIAN_POINT ( 'NONE',  ( 13.12265352643423810, -293.1604944259094623, -328.0626570769148884 ) ) ;
#22319 = CARTESIAN_POINT ( 'NONE',  ( -3.123438277038188549, -289.4145448140963595, -339.1744766487718152 ) ) ;
#22320 = CARTESIAN_POINT ( 'NONE',  ( 39.51579178095167322, -287.9876071046599009, -265.8157772788455873 ) ) ;
#22321 = CARTESIAN_POINT ( 'NONE',  ( -68.77685911055181123, -285.7937025303721725, -204.4623467902760865 ) ) ;
#22322 = ORIENTED_EDGE ( 'NONE', *, *, #58173, .F. ) ;
#22323 = DIRECTION ( 'NONE',  ( 0.000000000000000000, 0.000000000000000000, -1.000000000000000000 ) ) ;
#22324 = CARTESIAN_POINT ( 'NONE',  ( 23.05883952269570614, -296.0318247268497203, -316.1003822238880616 ) ) ;
#22325 = CARTESIAN_POINT ( 'NONE',  ( -44.76455706899341891, -293.8289323358789602, -346.5600922345200274 ) ) ;
#22326 = CARTESIAN_POINT ( 'NONE',  ( -89.63321428752651343, -278.3514089874425963, -219.0154283612944823 ) ) ;
#22327 = CARTESIAN_POINT ( 'NONE',  ( -29.83864214927978509, -273.6523845387918641, -193.7893802188771701 ) ) ;
#22328 = CARTESIAN_POINT ( 'NONE',  ( 8.645876542566494294, -292.8890217288209215, -328.0101088517621974 ) ) ;
#22329 = CARTESIAN_POINT ( 'NONE',  ( -11.15234293644558150, -276.1582111396244272, -201.0813940974743730 ) ) ;
#22330 = CARTESIAN_POINT ( 'NONE',  ( -36.44590794135725531, -296.3033739193555789, -196.3480507826911037 ) ) ;
#22331 = CARTESIAN_POINT ( 'NONE',  ( 32.73043291896075857, -295.0450869513113616, -292.2020583301730881 ) ) ;
#22332 = CARTESIAN_POINT ( 'NONE',  ( 35.73365375063811200, -294.7086709965415139, -276.2107956239953523 ) ) ;
#22333 = CYLINDRICAL_SURFACE ( 'NONE', #32391, 1.000000000000000888 ) ;
#22334 = CARTESIAN_POINT ( 'NONE',  ( -110.8031928773977057, -294.7566692924618224, -254.3814173703576955 ) ) ;
#22335 = CARTESIAN_POINT ( 'NONE',  ( 195.0023263777187879, -26.41817448500847121, 22.50000000000000000 ) ) ;
#22336 = CARTESIAN_POINT ( 'NONE',  ( -95.12885168234814159, -290.8613349915656840, -315.3708569196908229 ) ) ;
#22337 = CARTESIAN_POINT ( 'NONE',  ( -84.48851848982423007, -296.0553699304056181, -326.1882872526021515 ) ) ;
#22338 = CARTESIAN_POINT ( 'NONE',  ( -92.12060795084411779, -279.8093137243464525, -322.1822510230011858 ) ) ;
#22339 = CARTESIAN_POINT ( 'NONE',  ( -109.1375609850789346, -277.5749393122844140, -243.7762220551738039 ) ) ;
#22340 = CARTESIAN_POINT ( 'NONE',  ( 31.16325489794870762, -274.4502378675480259, -235.4271241777282455 ) ) ;
#22341 = CARTESIAN_POINT ( 'NONE',  ( -106.5618152735892608, -282.2711395297761783, -297.8856666084632820 ) ) ;
#22342 = CARTESIAN_POINT ( 'NONE',  ( -108.8483245638731489, -277.2900308443312269, -243.8793838174509574 ) ) ;
#22343 = CARTESIAN_POINT ( 'NONE',  ( -70.40466981549792536, -277.6171799058535612, -202.8565369035687809 ) ) ;
#22344 = CARTESIAN_POINT ( 'NONE',  ( -101.2202995325930033, -271.6247274893585768, -233.7224140011582847 ) ) ;
#22345 = CARTESIAN_POINT ( 'NONE',  ( -9.296786044609506305, -276.4187681308271181, -200.7475779080155007 ) ) ;
#22346 = CARTESIAN_POINT ( 'NONE',  ( 154.0367246112803628, 19.37030481724588427, 11.97322993578355721 ) ) ;
#22347 = CARTESIAN_POINT ( 'NONE',  ( -39.14647332109479549, -290.0497528034670154, -195.0147720683553700 ) ) ;
#22348 = CARTESIAN_POINT ( 'NONE',  ( -40.33875888029890433, -289.0888207388034061, -347.3158505621821632 ) ) ;
#22349 = CARTESIAN_POINT ( 'NONE',  ( 21.31140853968247484, -276.9069961180372843, -223.3317675410465881 ) ) ;
#22350 = CARTESIAN_POINT ( 'NONE',  ( -63.70200024966509034, -295.7076995178623520, -200.2694351082888886 ) ) ;
#22351 = CARTESIAN_POINT ( 'NONE',  ( -70.98628420594914701, -284.8166017956409632, -201.2800005653851372 ) ) ;
#22352 = DIRECTION ( 'NONE',  ( 0.000000000000000000, 0.000000000000000000, 1.000000000000000000 ) ) ;
#22353 = CARTESIAN_POINT ( 'NONE',  ( -49.72969589316242889, -283.8941206946745979, -196.3391989962462674 ) ) ;
#22354 = CARTESIAN_POINT ( 'NONE',  ( 17.06571399127465583, -89.54582641780471874, -22.50000000000000000 ) ) ;
#22355 = CARTESIAN_POINT ( 'NONE',  ( -47.03177989159605232, -290.7212455281394341, -197.6065108542599376 ) ) ;
#22356 = CARTESIAN_POINT ( 'NONE',  ( -102.0566968475360454, -283.1823730890629349, -233.8850359393497627 ) ) ;
#22357 = DIRECTION ( 'NONE',  ( -0.4646852846009911220, 0.2294442726657859866, 0.8552326654286331875 ) ) ;
#22358 = CYLINDRICAL_SURFACE ( 'NONE', #77592, 2.000000000000000000 ) ;
#22359 = CARTESIAN_POINT ( 'NONE',  ( 35.71804855944505874, -291.7702765558707938, -287.3667638010959422 ) ) ;
#22360 = CARTESIAN_POINT ( 'NONE',  ( -93.89840380726263902, -282.3297033735481705, -321.6059562243296455 ) ) ;
#22361 = CARTESIAN_POINT ( 'NONE',  ( -85.61328699062455883, -279.3328885731034461, -326.2525741948314817 ) ) ;
#22362 = CARTESIAN_POINT ( 'NONE',  ( -83.05130602156704356, -286.6474361096244934, -208.8243127904968901 ) ) ;
#22363 = CARTESIAN_POINT ( 'NONE',  ( -77.04906447840134831, -285.5040844853835438, -209.0449159922380602 ) ) ;
#22364 = CARTESIAN_POINT ( 'NONE',  ( -21.50869651191968401, -278.2705697538941081, -342.2793170866628429 ) ) ;
#22365 = CARTESIAN_POINT ( 'NONE',  ( -101.9948571213621875, -278.8895662267206603, -304.6039423004845617 ) ) ;
#22366 = CARTESIAN_POINT ( 'NONE',  ( -103.6754142631424003, -287.0174945349962172, -235.2521479287557611 ) ) ;
#22367 = EDGE_LOOP ( 'NONE', ( #75508, #11117, #70015, #54411 ) ) ;
#22368 = CARTESIAN_POINT ( 'NONE',  ( 201.2104617360081704, 60.19600395700752671, -6.999999999999999112 ) ) ;
#22369 = CARTESIAN_POINT ( 'NONE',  ( -112.2738668969146829, -296.6071601269771350, -252.6362657162317191 ) ) ;
#22370 = CARTESIAN_POINT ( 'NONE',  ( 32.95671788147570425, -289.8588623768545176, -295.4605049624124149 ) ) ;
#22371 = CARTESIAN_POINT ( 'NONE',  ( 115.2940338803257703, -299.5541904835127980, -192.9701481807315986 ) ) ;
#22372 = CARTESIAN_POINT ( 'NONE',  ( -19.11405058567862625, -282.7662352645559167, -190.3538533559490702 ) ) ;
#22373 = CARTESIAN_POINT ( 'NONE',  ( -108.3753195911104399, -277.1038626329275871, -299.2698954556213380 ) ) ;
#22374 = EDGE_CURVE ( 'NONE', #14651, #75846, #1876, .T. ) ;
#22375 = CARTESIAN_POINT ( 'NONE',  ( 6.140605363105556158, -292.8731093898400673, -333.0011896450453719 ) ) ;
#22376 = CARTESIAN_POINT ( 'NONE',  ( 17.39272361777657139, -288.3721519867979168, -220.9980796664841591 ) ) ;
#22377 = CARTESIAN_POINT ( 'NONE',  ( -109.8848725510550537, -280.5041089334150115, -255.6187524875688837 ) ) ;
#22378 = CARTESIAN_POINT ( 'NONE',  ( 21.05056746609663421, -289.6464695405196608, -319.6454905534583304 ) ) ;
#22379 = CARTESIAN_POINT ( 'NONE',  ( -112.0869438188197904, -286.4730103280032267, -276.5376212275803027 ) ) ;
#22380 = CARTESIAN_POINT ( 'NONE',  ( -112.9965772427299129, -278.8989257709359890, -255.9609180133413133 ) ) ;
#22381 = ORIENTED_EDGE ( 'NONE', *, *, #90122, .T. ) ;
#22382 = CARTESIAN_POINT ( 'NONE',  ( -37.80804921678049624, -296.0663921191614349, -195.7177704858326308 ) ) ;
#22383 = CARTESIAN_POINT ( 'NONE',  ( 36.91470676653590743, -291.4538943213717630, -256.3861319210874399 ) ) ;
#22384 = CARTESIAN_POINT ( 'NONE',  ( -84.56525879359641351, -279.2556363533514059, -209.4747704247852766 ) ) ;
#22385 = CARTESIAN_POINT ( 'NONE',  ( -24.40406663599654280, -276.0793243424434422, -197.2095273029512725 ) ) ;
#22386 = CARTESIAN_POINT ( 'NONE',  ( 153.9445672679061374, 19.37982107814384847, 11.06488088131597713 ) ) ;
#22387 = CARTESIAN_POINT ( 'NONE',  ( 21.31550574532285580, -296.6948066931273615, -317.0979686699210447 ) ) ;
#22388 = CARTESIAN_POINT ( 'NONE',  ( -60.54014508124423344, -271.9953094507193896, -197.9473554753666633 ) ) ;
#22389 = CARTESIAN_POINT ( 'NONE',  ( 197.2116943569230045, 249.5000000000000568, -12.92446933126075592 ) ) ;
#22390 = CARTESIAN_POINT ( 'NONE',  ( -51.83343822743881901, -279.3694759279116511, -198.6994432783881450 ) ) ;
#22391 = CARTESIAN_POINT ( 'NONE',  ( 33.82111179947592916, -277.1203923759173904, -298.8566777769632381 ) ) ;
#22392 = CARTESIAN_POINT ( 'NONE',  ( -77.85136105650438765, -298.9218706697556058, -208.8641990159432282 ) ) ;
#22393 = CARTESIAN_POINT ( 'NONE',  ( -104.2179396335195207, -283.1191518854671472, -308.1568553186463078 ) ) ;
#22394 = CARTESIAN_POINT ( 'NONE',  ( -48.18763493631013972, -290.9520428080189163, -343.6271877368289438 ) ) ;
#22395 = CARTESIAN_POINT ( 'NONE',  ( -105.8989597768701572, -298.5064153037426991, -236.8557467664184060 ) ) ;
#22396 = CARTESIAN_POINT ( 'NONE',  ( -109.4821066213579286, -298.0841180943501172, -244.5973746796761077 ) ) ;
#22397 = CARTESIAN_POINT ( 'NONE',  ( 30.05655093047798587, -295.9829947587128913, -302.9999946361118646 ) ) ;
#22398 = CARTESIAN_POINT ( 'NONE',  ( -15.62417824309960857, -280.7703005196200934, -341.9738100654732307 ) ) ;
#22399 = CARTESIAN_POINT ( 'NONE',  ( -43.59533959331694319, -271.9929972876396391, -195.9268828857573226 ) ) ;
#22400 = CARTESIAN_POINT ( 'NONE',  ( -70.73422973412071713, -287.2191737242491172, -201.8674731295454876 ) ) ;
#22401 = CARTESIAN_POINT ( 'NONE',  ( -26.44245367431672378, -287.8306597628556460, -342.9067445073270619 ) ) ;
#22402 = CARTESIAN_POINT ( 'NONE',  ( 140.3257785139489044, 179.6804926070224155, -241.2945171362309225 ) ) ;
#22403 = ORIENTED_EDGE ( 'NONE', *, *, #58734, .T. ) ;
#22404 = CARTESIAN_POINT ( 'NONE',  ( -74.15945537472130411, -288.1062803915087898, -337.3317089384698306 ) ) ;
#22405 = CARTESIAN_POINT ( 'NONE',  ( 21.18788884857454136, -287.8315694605126396, -314.0440985156255351 ) ) ;
#22406 = ORIENTED_EDGE ( 'NONE', *, *, #43878, .F. ) ;
#22407 = CARTESIAN_POINT ( 'NONE',  ( -93.70195066783594484, -286.3434533262437753, -218.2735178149416697 ) ) ;
#22408 = CARTESIAN_POINT ( 'NONE',  ( 9.680902497258630390, -276.7170976854366700, -326.2266917200656167 ) ) ;
#22409 = CARTESIAN_POINT ( 'NONE',  ( 38.54807015514720803, -292.3291765352909692, -258.9483610207844322 ) ) ;
#22410 = CARTESIAN_POINT ( 'NONE',  ( -99.70094065985946941, -284.6051363360588766, -315.4460690264696154 ) ) ;
#22412 = CARTESIAN_POINT ( 'NONE',  ( 38.71905078978815595, -282.9950219252702368, -264.2398500435169240 ) ) ;
#22411 = B_SPLINE_CURVE_WITH_KNOTS ( 'NONE', 3,
 ( #71971, #85675, #20823, #49693, #78588, #35961 ),
 .UNSPECIFIED., .F., .F.,
 ( 4, 2, 4 ),
 ( 0.000000000000000000, 0.0009570384287224865559, 0.001914076857444973112 ),
 .UNSPECIFIED. ) ;
#22413 = CARTESIAN_POINT ( 'NONE',  ( -0.3818607462137903474, -282.9078857694941007, -337.9017119002714367 ) ) ;
#22414 = CARTESIAN_POINT ( 'NONE',  ( -32.96598651701893345, -280.4420792808553529, -197.4711967505822372 ) ) ;
#22415 = CARTESIAN_POINT ( 'NONE',  ( -70.86830917777322725, -196.3883269678753152, -360.5550801755780981 ) ) ;
#22416 = CARTESIAN_POINT ( 'NONE',  ( -109.5836222876633315, -280.3007506750664675, -289.8837487389042735 ) ) ;
#22417 = CARTESIAN_POINT ( 'NONE',  ( 160.1180839598566195, 220.5390337495420283, -204.7865604871097105 ) ) ;
#22418 = CARTESIAN_POINT ( 'NONE',  ( 178.1438528349047203, 252.3106890361019907, -164.5180092551200630 ) ) ;
#22419 = CARTESIAN_POINT ( 'NONE',  ( -93.03006199293928091, -272.4229359308798166, -222.8927779124822450 ) ) ;
#22420 = CARTESIAN_POINT ( 'NONE',  ( -13.80683339856973824, -294.2623488004030037, -343.6116261796562981 ) ) ;
#22421 = CARTESIAN_POINT ( 'NONE',  ( 103.8198587862023459, 114.2352195572753573, -279.7816234916556937 ) ) ;
#22423 = CARTESIAN_POINT ( 'NONE',  ( -108.5026076409199334, -288.6941695497823162, -290.1089206472752835 ) ) ;
#22422 = CARTESIAN_POINT ( 'NONE',  ( -106.3909035283975868, -271.6620883614435797, -237.4141032285587869 ) ) ;
#22424 = CARTESIAN_POINT ( 'NONE',  ( -97.39390445610423797, -297.8116808824607915, -314.0245089040078597 ) ) ;
#22425 = CARTESIAN_POINT ( 'NONE',  ( 36.17319654799493378, -288.8400893544101109, -268.2819100810057762 ) ) ;
#22426 = VERTEX_POINT ( 'NONE', #74982 ) ;
#22427 = CARTESIAN_POINT ( 'NONE',  ( -97.21635824852825181, -296.8475193097922897, -318.4219584456608345 ) ) ;
#22428 = CARTESIAN_POINT ( 'NONE',  ( 20.38542466001556619, -287.4142440313824522, -225.5775550876500972 ) ) ;
#22429 = CARTESIAN_POINT ( 'NONE',  ( -63.43893346195628169, -272.6402136818743998, -198.2471323640708363 ) ) ;
#22430 = CARTESIAN_POINT ( 'NONE',  ( 19.41732322056124005, -295.0612952465291414, -322.2321828044285894 ) ) ;
#22431 = CARTESIAN_POINT ( 'NONE',  ( -3.354190619114073346, -292.9812325736764933, -201.3221324680027919 ) ) ;
#22432 = CARTESIAN_POINT ( 'NONE',  ( -103.5572096936009530, -291.1336785839383765, -239.6282968061431120 ) ) ;
#22433 = ORIENTED_EDGE ( 'NONE', *, *, #46209, .F. ) ;
#22434 = CARTESIAN_POINT ( 'NONE',  ( -105.5539529197887703, -274.8968957535345794, -237.8587678488131303 ) ) ;
#22435 = CARTESIAN_POINT ( 'NONE',  ( 1.009986396717812207, -273.3470126578176291, -204.0348487712289511 ) ) ;
#22436 = VERTEX_POINT ( 'NONE', #66936 ) ;
#22437 = CARTESIAN_POINT ( 'NONE',  ( -104.7366608798621144, -278.5409080611475474, -233.2471560768232166 ) ) ;
#22438 = CARTESIAN_POINT ( 'NONE',  ( -6.172774650221306558, -272.8685870005797938, -203.4661368404431983 ) ) ;
#22439 = CARTESIAN_POINT ( 'NONE',  ( -96.53908632886891894, -274.2357801045013730, -227.0344700584482212 ) ) ;
#22440 = CARTESIAN_POINT ( 'NONE',  ( 26.83696552098341570, -276.0118057899703672, -234.9778805313569308 ) ) ;
#22441 = CARTESIAN_POINT ( 'NONE',  ( -3.868772761384751124, -300.0647303613785652, -194.1521717235641518 ) ) ;
#22442 = CARTESIAN_POINT ( 'NONE',  ( -4.729988934791962585, -274.6448911267726771, -338.3082351913516277 ) ) ;
#22443 = CARTESIAN_POINT ( 'NONE',  ( -72.16584159823331390, -296.1770615841671770, -334.6495987859615866 ) ) ;
#22444 = CARTESIAN_POINT ( 'NONE',  ( 19.27489436450392901, -292.7883262167277962, -317.3710759365084755 ) ) ;
#22445 = DIRECTION ( 'NONE',  ( 0.000000000000000000, 0.000000000000000000, 1.000000000000000000 ) ) ;
#22446 = CARTESIAN_POINT ( 'NONE',  ( -70.26898557065474904, -277.9668062097417760, -339.9120142852159461 ) ) ;
#22447 = CARTESIAN_POINT ( 'NONE',  ( 23.05113954428155765, -275.1482639459219399, -229.3301015376934799 ) ) ;
#22448 = EDGE_CURVE ( 'NONE', #63080, #8882, #74495, .T. ) ;
#22449 = CARTESIAN_POINT ( 'NONE',  ( -104.9881786169803206, -283.7026935975775928, -234.5090665878209393 ) ) ;
#22450 = CARTESIAN_POINT ( 'NONE',  ( -102.9890394261793602, -298.0648251094286252, -307.0796874485572516 ) ) ;
#22451 = CYLINDRICAL_SURFACE ( 'NONE', #79297, 2.000000000000001776 ) ;
#22452 = CARTESIAN_POINT ( 'NONE',  ( -81.56808382118443035, -284.6296206617756184, -212.0805147610245456 ) ) ;
#22453 = CARTESIAN_POINT ( 'NONE',  ( -109.2692225733536588, -277.0190558710642676, -252.9138966800696835 ) ) ;
#22454 = CARTESIAN_POINT ( 'NONE',  ( -76.68606469585640184, -276.1643811171157381, -332.6094468953904197 ) ) ;
#22455 = CARTESIAN_POINT ( 'NONE',  ( -110.8647083862474574, -286.3613181809882349, -285.2360512963271049 ) ) ;
#22456 = CARTESIAN_POINT ( 'NONE',  ( -2.739948351401155335, -275.7255210193334847, -205.6320728821359580 ) ) ;
#22457 = CARTESIAN_POINT ( 'NONE',  ( 197.8563597697584839, 42.27872732282708057, 12.00000000000000355 ) ) ;
#22458 = CARTESIAN_POINT ( 'NONE',  ( 38.90666704328149450, -273.9624179993852522, -271.1835598520960389 ) ) ;
#22459 = CARTESIAN_POINT ( 'NONE',  ( -69.20887382580913538, -281.6341555470060598, -202.2698216998622058 ) ) ;
#22460 = CARTESIAN_POINT ( 'NONE',  ( 222.2216768131362130, 37.54180348216212337, 7.000000000000000000 ) ) ;
#22461 = CARTESIAN_POINT ( 'NONE',  ( -49.14437751031390178, -287.8231763335015216, -195.6758789415342790 ) ) ;
#22462 = B_SPLINE_CURVE_WITH_KNOTS ( 'NONE', 3,
 ( #76881, #32855, #12008, #89654, #53707, #82574, #17722, #46577, #61744, #90576, #5401, #92003 ),
 .UNSPECIFIED., .F., .F.,
 ( 4, 2, 2, 2, 2, 4 ),
 ( 0.000000000000000000, 0.002326201313189183318, 0.004652402626378366636, 0.006978603939567550388, 0.008141704596162134891, 0.009304805252756721129 ),
 .UNSPECIFIED. ) ;
#22463 = FILL_AREA_STYLE_COLOUR ( '', #44045 ) ;
#22464 = CARTESIAN_POINT ( 'NONE',  ( 20.78113675958304896, -290.8987050903985505, -222.9414242994105564 ) ) ;
#22465 = CARTESIAN_POINT ( 'NONE',  ( 82.16127410785169616, -298.5792860220823854, -197.1167434283082969 ) ) ;
#22466 = CARTESIAN_POINT ( 'NONE',  ( -73.02658463023458069, -296.3628394684810701, -206.2228336009708300 ) ) ;
#22467 = CARTESIAN_POINT ( 'NONE',  ( -95.23962990857572208, -289.3376935585451974, -223.8791649500989536 ) ) ;
#22468 = CARTESIAN_POINT ( 'NONE',  ( -84.42323508662160236, -232.9070939334762329, -346.4289530206739300 ) ) ;
#22469 = CARTESIAN_POINT ( 'NONE',  ( -61.12666982825986395, -295.7433451171331171, -199.1776039324604142 ) ) ;
#22470 = CARTESIAN_POINT ( 'NONE',  ( -103.2098144371225317, -288.5249129832526478, -308.9896842094865406 ) ) ;
#22471 = CARTESIAN_POINT ( 'NONE',  ( 10.44202075880268943, -283.9800635391399624, -326.6702840655408409 ) ) ;
#22472 = CARTESIAN_POINT ( 'NONE',  ( -110.1436449404158964, -282.5146899080751837, -292.1744620578613194 ) ) ;
#22473 = CARTESIAN_POINT ( 'NONE',  ( -4.548414203436010439, -284.0365622864845818, -336.2396070149167144 ) ) ;
#22474 = CARTESIAN_POINT ( 'NONE',  ( -67.84238802978804017, -284.2658978095436169, -336.8615673419376435 ) ) ;
#22475 = EDGE_CURVE ( 'NONE', #78431, #59355, #9149, .T. ) ;
#22476 = CARTESIAN_POINT ( 'NONE',  ( -105.0248430746607511, -292.0959797869946328, -303.6066591384906701 ) ) ;
#22477 = CARTESIAN_POINT ( 'NONE',  ( -18.55924196096452050, -274.6208300385341659, -195.6538195044522581 ) ) ;
#22478 = CARTESIAN_POINT ( 'NONE',  ( -54.20449545069922692, -287.3467715438604273, -344.0691402898726210 ) ) ;
#22479 = CARTESIAN_POINT ( 'NONE',  ( 38.92417607413189273, -275.4194924690856965, -259.7537560528111271 ) ) ;
#22480 = CARTESIAN_POINT ( 'NONE',  ( 9.274592697482173520, -296.3884727372923749, -328.7265195592930240 ) ) ;
#22481 = CARTESIAN_POINT ( 'NONE',  ( 139.6925840978351516, -0.9999999999999859002, -22.50000000000000000 ) ) ;
#22482 = CARTESIAN_POINT ( 'NONE',  ( 99.44099354567467230, -302.2645883696979467, -195.3030568020281521 ) ) ;
#22483 = CARTESIAN_POINT ( 'NONE',  ( -45.71215689695105766, -281.8451461596557124, -343.4273801591559732 ) ) ;
#22484 = CARTESIAN_POINT ( 'NONE',  ( -111.4948372707474675, -276.3943856883842045, -282.6631779616280937 ) ) ;
#22485 = ORIENTED_EDGE ( 'NONE', *, *, #4102, .T. ) ;
#22486 = CARTESIAN_POINT ( 'NONE',  ( -31.95916909530536998, -296.5183538027648638, -194.1625494488639561 ) ) ;
#22487 = CARTESIAN_POINT ( 'NONE',  ( 33.61011650764340430, -274.6688226728804807, -252.7619025280739606 ) ) ;
#22488 = CARTESIAN_POINT ( 'NONE',  ( -25.31482904837751136, -293.7282247890242388, -197.6038423582666894 ) ) ;
#22489 = CARTESIAN_POINT ( 'NONE',  ( 19.88511512992895192, -295.1370610797394534, -316.0812238694236953 ) ) ;
#22490 = CARTESIAN_POINT ( 'NONE',  ( -90.40478407308286535, -287.0488278596349687, -218.6902306258596127 ) ) ;
#22491 = CARTESIAN_POINT ( 'NONE',  ( 37.49718685151719200, -295.1717421387989475, -285.7801740642635764 ) ) ;
#22492 = CARTESIAN_POINT ( 'NONE',  ( 26.11215191008017200, -295.4340730176405714, -313.1034498590222483 ) ) ;
#22493 = CARTESIAN_POINT ( 'NONE',  ( -110.2121603534482119, -296.4428146462902305, -266.0141614575670133 ) ) ;
#22494 = CARTESIAN_POINT ( 'NONE',  ( -102.0160429505700677, -292.0435366280884182, -308.4400537465915022 ) ) ;
#22495 = CARTESIAN_POINT ( 'NONE',  ( -81.55982012790093449, -283.8019995466293039, -333.4637324805561889 ) ) ;
#22496 = CARTESIAN_POINT ( 'NONE',  ( -96.82829257484100083, -271.3295856147320251, -223.4393660561182458 ) ) ;
#22497 = CARTESIAN_POINT ( 'NONE',  ( -18.17997500119582455, -286.1256957482785310, -195.7283489597987227 ) ) ;
#22498 = CARTESIAN_POINT ( 'NONE',  ( -62.31692380987604452, -279.3583674818408440, -340.7586879571641703 ) ) ;
#22499 = EDGE_CURVE ( 'NONE', #31059, #10831, #51780, .T. ) ;
#22500 = CARTESIAN_POINT ( 'NONE',  ( -38.61649543187973421, -284.8307717300806985, -196.9625654323137098 ) ) ;
#22501 = AXIS2_PLACEMENT_3D ( 'NONE', #35283, #65132, #13985 ) ;
#22502 = CARTESIAN_POINT ( 'NONE',  ( 21.69691511056095123, -286.1869833321935630, -316.6358973213487502 ) ) ;
#22503 = CARTESIAN_POINT ( 'NONE',  ( -103.7001496316577516, -277.1730595717525603, -233.7979991656895606 ) ) ;
#22504 = CARTESIAN_POINT ( 'NONE',  ( -108.4555765497910471, -262.4588243622614527, -317.8183916042563055 ) ) ;
#22505 = CARTESIAN_POINT ( 'NONE',  ( -65.11080558841855748, -285.1870441594747945, -202.7286816938384959 ) ) ;
#22506 = CARTESIAN_POINT ( 'NONE',  ( 35.23783331925652362, -283.0692704806687061, -295.0254507566252187 ) ) ;
#22507 = CARTESIAN_POINT ( 'NONE',  ( -73.07500556531870473, -288.5727144053486199, -338.3166214257569209 ) ) ;
#22508 = CARTESIAN_POINT ( 'NONE',  ( -39.91530906589232330, -278.6840701793875041, -346.5305779452963293 ) ) ;
#22509 = CARTESIAN_POINT ( 'NONE',  ( -86.76377785003018062, -279.0376679027629052, -328.8321039229232383 ) ) ;
#22510 = CARTESIAN_POINT ( 'NONE',  ( -43.74897457045302218, -279.8023882867135512, -197.5926137027811649 ) ) ;
#22511 = CARTESIAN_POINT ( 'NONE',  ( -32.61143097120459089, -276.0919350915609698, -195.8535353109436983 ) ) ;
#22512 = CARTESIAN_POINT ( 'NONE',  ( 38.07058928899563455, -293.7467003975645525, -285.9170366270830641 ) ) ;
#22513 = CARTESIAN_POINT ( 'NONE',  ( -85.77091236000565289, -287.7461447193713866, -327.2312823814820604 ) ) ;
#22514 = CARTESIAN_POINT ( 'NONE',  ( -105.2999646326113918, -292.6020122703067159, -235.7756756215604526 ) ) ;
#22515 = CARTESIAN_POINT ( 'NONE',  ( 33.41143883832940276, -292.7254602204116054, -289.5978569015352377 ) ) ;
#22516 = CARTESIAN_POINT ( 'NONE',  ( 28.41174480821354820, -293.6499285505595935, -302.2357345633083128 ) ) ;
#22517 = CARTESIAN_POINT ( 'NONE',  ( -112.3405887715641143, -291.8337275631249668, -254.2785198051710722 ) ) ;
#22518 = CARTESIAN_POINT ( 'NONE',  ( 34.58723590186753682, -282.3763117907469109, -283.4743403701189095 ) ) ;
#22519 = CARTESIAN_POINT ( 'NONE',  ( -89.99273195207298670, -272.3891525716839510, -214.4254113431359485 ) ) ;
#22520 = CARTESIAN_POINT ( 'NONE',  ( -68.00559948550848333, -290.0957112385090682, -340.8808887071532467 ) ) ;
#22521 = CARTESIAN_POINT ( 'NONE',  ( -95.34029919066875891, -282.0244653891793973, -319.1302302714141774 ) ) ;
#22522 = CARTESIAN_POINT ( 'NONE',  ( -65.43535045956707563, -289.7426903436191310, -342.0867616799149005 ) ) ;
#22523 = CARTESIAN_POINT ( 'NONE',  ( 11.14492882572142030, -287.0787179588227787, -215.6934204259425485 ) ) ;
#22524 = CARTESIAN_POINT ( 'NONE',  ( 82.64890176555634582, -299.5541904835127980, -195.3611179825600175 ) ) ;
#22525 = CARTESIAN_POINT ( 'NONE',  ( 178.0079900246404350, 253.3980089039855557, -165.2740606419443736 ) ) ;
#22526 = CARTESIAN_POINT ( 'NONE',  ( 153.0936500521454775, 204.7395457004011234, -214.2756457972470230 ) ) ;
#22527 = CARTESIAN_POINT ( 'NONE',  ( -62.35456707728842218, -278.9155811341140634, -201.5547681482764517 ) ) ;
#22528 = CARTESIAN_POINT ( 'NONE',  ( -27.50333598972031979, -279.1002600405496992, -197.6637688007097040 ) ) ;
#22529 = CARTESIAN_POINT ( 'NONE',  ( 20.02295116130064301, -274.5217958678194918, -218.9501269829323746 ) ) ;
#22530 = CARTESIAN_POINT ( 'NONE',  ( -68.78722892216374873, -196.9352846320093136, -357.8051255537320685 ) ) ;
#22531 = CARTESIAN_POINT ( 'NONE',  ( -112.4138460204593599, -277.3072307530179614, -256.0511723597472269 ) ) ;
#22532 = CARTESIAN_POINT ( 'NONE',  ( -7.867465775643090353, -280.6841339257362051, -338.9403882776479691 ) ) ;
#22533 = CARTESIAN_POINT ( 'NONE',  ( -25.04935531457887876, -296.6577441006658660, -345.4002883162921194 ) ) ;
#22534 = CARTESIAN_POINT ( 'NONE',  ( -62.82806531799420213, -292.2035393942699102, -201.8889803566277408 ) ) ;
#22535 = CARTESIAN_POINT ( 'NONE',  ( -89.01965424845269581, -288.4823313306475825, -322.6165725824428137 ) ) ;
#22536 = CARTESIAN_POINT ( 'NONE',  ( 19.32610810018613989, -299.2361782822673604, -193.4180472008978597 ) ) ;
#22537 = CARTESIAN_POINT ( 'NONE',  ( -110.0990318594879511, -296.6325513537497613, -276.9017552651960159 ) ) ;
#22538 = ORIENTED_EDGE ( 'NONE', *, *, #71792, .T. ) ;
#22539 = DIRECTION ( 'NONE',  ( 1.000000000000000000, -0.000000000000000000, -0.000000000000000000 ) ) ;
#22540 = CARTESIAN_POINT ( 'NONE',  ( -111.6450297054304315, -280.2964986378397043, -284.1553986849187368 ) ) ;
#22541 = CARTESIAN_POINT ( 'NONE',  ( 18.18972221567073078, -281.9528689193521132, -222.4828179980798950 ) ) ;
#22542 = CARTESIAN_POINT ( 'NONE',  ( -97.11769008258531244, -279.6767489313735382, -317.2738565767593286 ) ) ;
#22543 = CARTESIAN_POINT ( 'NONE',  ( 33.87615759099319490, -280.8360735141135933, -287.4856144781021499 ) ) ;
#22544 = CARTESIAN_POINT ( 'NONE',  ( -43.52114399251894383, -272.4526933469902588, -196.8761311456931651 ) ) ;
#22545 = CARTESIAN_POINT ( 'NONE',  ( 41.08708295871279859, -296.0521521680024080, -430.6442049081568939 ) ) ;
#22546 = CARTESIAN_POINT ( 'NONE',  ( 153.9133111279453203, 20.47222690886559704, 13.06183683676577267 ) ) ;
#22547 = CARTESIAN_POINT ( 'NONE',  ( 24.24437521223253711, -276.9675000215099772, -316.3101565485692959 ) ) ;
#22548 = CARTESIAN_POINT ( 'NONE',  ( 25.97444438457528193, -278.0943193268141158, -310.6580346857036261 ) ) ;
#22549 = CARTESIAN_POINT ( 'NONE',  ( -88.82857463648720397, -276.3334075857380299, -326.8209093824336264 ) ) ;
#22550 = ORIENTED_EDGE ( 'NONE', *, *, #31259, .F. ) ;
#22551 = CARTESIAN_POINT ( 'NONE',  ( 199.4955644831718189, 40.18497343027721769, 10.63455718547475648 ) ) ;
#22552 = CARTESIAN_POINT ( 'NONE',  ( 20.36700430224048830, -284.1986966210026253, -318.8184418773226980 ) ) ;
#22553 = CARTESIAN_POINT ( 'NONE',  ( -99.84426448602748394, -290.2718940567323216, -232.3344013821432270 ) ) ;
#22554 = CARTESIAN_POINT ( 'NONE',  ( 18.28350567566745966, -286.1730485862634623, -217.1886532087675050 ) ) ;
#22555 = CARTESIAN_POINT ( 'NONE',  ( -21.18859054937971464, -281.0820905885889260, -342.6430061844567376 ) ) ;
#22556 = CARTESIAN_POINT ( 'NONE',  ( -87.34239674746299897, -282.3401877989085165, -324.4244157405486249 ) ) ;
#22557 = AXIS2_PLACEMENT_3D ( 'NONE', #8601, #37931, #89519 ) ;
#22558 = CARTESIAN_POINT ( 'NONE',  ( -11.61828678393587566, -281.5997044746429196, -201.5655645842719252 ) ) ;
#22559 = DIRECTION ( 'NONE',  ( -0.3428573139466628561, 0.000000000000000000, 0.9393874931428879416 ) ) ;
#22560 = CARTESIAN_POINT ( 'NONE',  ( -94.74563448016067468, -282.2672103572789410, -320.4732795560731802 ) ) ;
#22561 = CARTESIAN_POINT ( 'NONE',  ( -112.2349716561223261, -298.4897306966552151, -275.2354500860950566 ) ) ;
#22562 = CARTESIAN_POINT ( 'NONE',  ( -106.6713477330333575, -279.8078359778444906, -246.6085214829126642 ) ) ;
#22563 = CARTESIAN_POINT ( 'NONE',  ( -109.1815857544270330, -286.8388378424853045, -248.0710490295336683 ) ) ;
#22564 = DIRECTION ( 'NONE',  ( 0.000000000000000000, 0.000000000000000000, -1.000000000000000000 ) ) ;
#22565 = DIRECTION ( 'NONE',  ( 0.000000000000000000, 0.9681751575201842375, 0.2502735790305606889 ) ) ;
#22566 = CARTESIAN_POINT ( 'NONE',  ( 38.27060701774458096, -295.4713574460122913, -270.2865095391824184 ) ) ;
#22567 = CARTESIAN_POINT ( 'NONE',  ( 10.93243487874202735, -274.3840315797502853, -327.7597985865685928 ) ) ;
#22568 = CARTESIAN_POINT ( 'NONE',  ( -67.99886345592852877, -288.6417004884300468, -340.8188865930616771 ) ) ;
#22569 = CARTESIAN_POINT ( 'NONE',  ( 34.08759011211144241, -291.7097103146563768, -251.8058784879941356 ) ) ;
#22570 = CARTESIAN_POINT ( 'NONE',  ( -95.67459479516085707, -276.6122773088797544, -315.0658926624392961 ) ) ;
#22571 = CARTESIAN_POINT ( 'NONE',  ( -111.0335929686983860, -294.5700828966379845, -279.7387666122154997 ) ) ;
#22572 = CARTESIAN_POINT ( 'NONE',  ( -70.45782826173180524, -292.9212209856526101, -204.7519300827885900 ) ) ;
#22573 = CARTESIAN_POINT ( 'NONE',  ( -85.28047601435906699, -280.1948066931273615, -330.5268031993605859 ) ) ;
#22574 = CARTESIAN_POINT ( 'NONE',  ( -44.74777653480868622, -293.6240174303553090, -346.3604583207958285 ) ) ;
#22575 = CARTESIAN_POINT ( 'NONE',  ( 29.52630890934421259, -288.7351815748234003, -239.1343701470424605 ) ) ;
#22576 = CARTESIAN_POINT ( 'NONE',  ( -111.6443060708512292, -288.9943751328019061, -254.3908009182405578 ) ) ;
#22577 = CARTESIAN_POINT ( 'NONE',  ( -29.08916763974091424, -290.3707935216937130, -343.4861521648430767 ) ) ;
#22578 = CYLINDRICAL_SURFACE ( 'NONE', #71327, 1.897123461337413275 ) ;
#22579 = CARTESIAN_POINT ( 'NONE',  ( -88.76732337151497632, -290.5999965870382198, -322.3996325732541663 ) ) ;
#22580 = EDGE_CURVE ( 'NONE', #46169, #33107, #59378, .T. ) ;
#22581 = CARTESIAN_POINT ( 'NONE',  ( 82.70991478241074901, -294.7622393454342955, -197.7570935515998087 ) ) ;
#22582 = CARTESIAN_POINT ( 'NONE',  ( 5.348826291215152295, -289.6933149964566496, -333.9655806547092425 ) ) ;
#22583 = CARTESIAN_POINT ( 'NONE',  ( -106.9827673550305320, -276.9461017368034845, -241.5769460174636265 ) ) ;
#22584 = CARTESIAN_POINT ( 'NONE',  ( -36.75697793451085005, -280.3925927418611082, -193.3714407658291350 ) ) ;
#22585 = CARTESIAN_POINT ( 'NONE',  ( -10.71333275034624499, -282.3810366851079152, -342.6442961314813829 ) ) ;
#22586 = CARTESIAN_POINT ( 'NONE',  ( 27.41025551473672550, -286.0588070559125526, -308.3079504644597932 ) ) ;
#22587 = DIRECTION ( 'NONE',  ( -1.000000000000000000, -0.000000000000000000, -0.000000000000000000 ) ) ;
#22588 = CARTESIAN_POINT ( 'NONE',  ( 1.058847993968061063, -278.7097230569691533, -206.7700097325325999 ) ) ;
#22589 = CARTESIAN_POINT ( 'NONE',  ( -30.42535961952033929, -280.9644985858746509, -345.0415363157139268 ) ) ;
#22590 = CARTESIAN_POINT ( 'NONE',  ( 181.0082777314984241, 252.6787652719002040, -164.6486270092325128 ) ) ;
#22591 = CARTESIAN_POINT ( 'NONE',  ( -98.85734849419212367, -277.6373887186409206, -225.1889591390722956 ) ) ;
#22592 = CARTESIAN_POINT ( 'NONE',  ( -95.11098289941921280, -282.7875832412171917, -320.8012059922886579 ) ) ;
#22593 = CARTESIAN_POINT ( 'NONE',  ( 52.01832293716342548, -300.1390605925521982, -197.1111399590675148 ) ) ;
#22594 = CARTESIAN_POINT ( 'NONE',  ( -87.66208520482945232, -274.7911321845207340, -212.7888858945432276 ) ) ;
#22595 = CARTESIAN_POINT ( 'NONE',  ( -16.37885764104276021, -276.4404811782455909, -340.3615981858769146 ) ) ;
#22596 = CARTESIAN_POINT ( 'NONE',  ( -79.04113971308001396, -297.6142186600198443, -332.7628848608052863 ) ) ;
#22597 = CARTESIAN_POINT ( 'NONE',  ( -105.1549656640309109, -290.2472513649459529, -306.8352323904114769 ) ) ;
#22598 = CARTESIAN_POINT ( 'NONE',  ( 35.60141979152266600, -279.3798612572268212, -250.5986592957176811 ) ) ;
#22599 = CARTESIAN_POINT ( 'NONE',  ( 23.10939165632237291, -292.7473551402242720, -222.6465942237843478 ) ) ;
#22600 = EDGE_CURVE ( 'NONE', #55409, #27807, #71451, .T. ) ;
#22601 = CARTESIAN_POINT ( 'NONE',  ( -31.86568611225878911, -288.0402444912931514, -343.4421837259578183 ) ) ;
#22602 = CARTESIAN_POINT ( 'NONE',  ( 36.83465199597038975, -291.6943164942666158, -281.4457665902666008 ) ) ;
#22603 = VERTEX_POINT ( 'NONE', #81589 ) ;
#22604 = CARTESIAN_POINT ( 'NONE',  ( 196.8803347170859865, 73.40565171261611965, 12.50000000000000711 ) ) ;
#22605 = CARTESIAN_POINT ( 'NONE',  ( -88.70878431863918934, -289.3050255424132047, -322.3169752399836625 ) ) ;
#22606 = LINE ( 'NONE', #73293, #53482 ) ;
#22607 = CARTESIAN_POINT ( 'NONE',  ( -7.445859927967695135, -287.3757928195747127, -199.6006166529968198 ) ) ;
#22608 = CARTESIAN_POINT ( 'NONE',  ( -6.941161984400275209, -297.1233781216987495, -333.4151289067050357 ) ) ;
#22609 = CARTESIAN_POINT ( 'NONE',  ( 22.09681380320278876, -293.2652029048347231, -318.9603791118698268 ) ) ;
#22610 = CARTESIAN_POINT ( 'NONE',  ( 17.48464388436363848, -283.6042872458888269, -323.7975903708006058 ) ) ;
#22611 = CARTESIAN_POINT ( 'NONE',  ( -110.3188846175833362, -284.3422696491132911, -273.6360186376242041 ) ) ;
#22612 = CARTESIAN_POINT ( 'NONE',  ( 22.87949496039619746, -277.4518885941686790, -312.5751226865164654 ) ) ;
#22613 = CARTESIAN_POINT ( 'NONE',  ( 24.27681434211216072, -292.1466705259947503, -312.5822780444832460 ) ) ;
#22614 = CARTESIAN_POINT ( 'NONE',  ( 25.62432395733213752, -273.8299538586905442, -232.5477868144641604 ) ) ;
#22615 = ORIENTED_EDGE ( 'NONE', *, *, #10809, .F. ) ;
#22616 = CARTESIAN_POINT ( 'NONE',  ( -32.04911714649202992, -124.5213432794980974, -365.6788127701597659 ) ) ;
#22617 = CARTESIAN_POINT ( 'NONE',  ( 29.55419283905159489, -293.7148451698776057, -308.5566313757004764 ) ) ;
#22618 = CARTESIAN_POINT ( 'NONE',  ( -10.24820624270802050, -288.3286735793968205, -201.0129434889128390 ) ) ;
#22619 = CARTESIAN_POINT ( 'NONE',  ( -101.3626108634006187, -297.0732757896138878, -312.6805340037668088 ) ) ;
#22620 = EDGE_CURVE ( 'NONE', #11326, #69004, #33570, .T. ) ;
#22621 = CARTESIAN_POINT ( 'NONE',  ( -52.11763068027443779, -286.5093794383482191, -198.7680698273709083 ) ) ;
#22622 = CARTESIAN_POINT ( 'NONE',  ( -107.2000071094652611, -278.0203483367379249, -238.4112205248872840 ) ) ;
#22623 = CARTESIAN_POINT ( 'NONE',  ( -77.02251135453006725, -296.2201432068360987, -336.2922210778831413 ) ) ;
#22624 = CARTESIAN_POINT ( 'NONE',  ( -62.37820261873216765, -287.5138601287436018, -341.9251985713036106 ) ) ;
#22625 = CIRCLE ( 'NONE', #87635, 5.603083949679982467 ) ;
#22626 = CARTESIAN_POINT ( 'NONE',  ( 39.21651000224836991, -293.9921059565856467, -278.8883081489851747 ) ) ;
#22627 = CARTESIAN_POINT ( 'NONE',  ( -107.4167836424392277, -291.1575248568599932, -249.7845368836059947 ) ) ;
#22628 = CARTESIAN_POINT ( 'NONE',  ( 159.6810783670777880, 8.542400036368780647, 25.74970488511327815 ) ) ;
#22629 = DIRECTION ( 'NONE',  ( 0.000000000000000000, 0.000000000000000000, 1.000000000000000000 ) ) ;
#22630 = CARTESIAN_POINT ( 'NONE',  ( -38.36988802030046486, -140.4513536129776412, -361.1260187711050662 ) ) ;
#22631 = AXIS2_PLACEMENT_3D ( 'NONE', #21535, #56131, #63727 ) ;
#22632 = CARTESIAN_POINT ( 'NONE',  ( 37.99366567511329151, -289.2294910628455114, -282.8191850300649435 ) ) ;
#22633 = CARTESIAN_POINT ( 'NONE',  ( 13.84574458161073807, -284.1952119285919025, -206.2264541496106460 ) ) ;
#22634 = ORIENTED_EDGE ( 'NONE', *, *, #3118, .F. ) ;
#22635 = CARTESIAN_POINT ( 'NONE',  ( -113.9415690105022065, -277.9927306780792264, -263.0154000966647345 ) ) ;
#22636 = CARTESIAN_POINT ( 'NONE',  ( 34.87631109955725606, -283.2990262893106319, -250.7012581078978428 ) ) ;
#22637 = CARTESIAN_POINT ( 'NONE',  ( -10.86276471313879632, -92.93242878793211048, -358.8789665578360086 ) ) ;
#22638 = CARTESIAN_POINT ( 'NONE',  ( -106.4802662602394463, -282.7069542370766158, -302.8951765131579350 ) ) ;
#22639 = CARTESIAN_POINT ( 'NONE',  ( -18.12489030421997427, -286.8825176474620093, -342.3315523510055414 ) ) ;
#22640 = CARTESIAN_POINT ( 'NONE',  ( -27.18592835138849040, -276.0401994777554933, -195.2274848994934757 ) ) ;
#22641 = CARTESIAN_POINT ( 'NONE',  ( -68.07912563937648542, -298.1297021990621374, -204.0662291882327395 ) ) ;
#22642 = CARTESIAN_POINT ( 'NONE',  ( 6.342712854686643809, -293.1299441708004565, -329.5254223798096405 ) ) ;
#22643 = CARTESIAN_POINT ( 'NONE',  ( 26.19170978608781297, -281.6303565386378978, -226.9459562399169670 ) ) ;
#22645 = CARTESIAN_POINT ( 'NONE',  ( -108.7044529258909336, -278.1102324348433399, -254.4529716086750852 ) ) ;
#22644 = CARTESIAN_POINT ( 'NONE',  ( -13.78539871757494240, -276.7378892667989589, -339.5091228563138088 ) ) ;
#22646 = CARTESIAN_POINT ( 'NONE',  ( -64.80229165145864556, -274.7814801134947515, -198.7410636321780544 ) ) ;
#22647 = CARTESIAN_POINT ( 'NONE',  ( -37.14163223813358883, -275.9700018962540184, -347.0647523795010443 ) ) ;
#22648 = DIRECTION ( 'NONE',  ( 0.000000000000000000, 0.000000000000000000, 1.000000000000000000 ) ) ;
#22649 = CARTESIAN_POINT ( 'NONE',  ( -67.38406429639361761, -275.4459653811994713, -339.0949792678342192 ) ) ;
#22650 = CARTESIAN_POINT ( 'NONE',  ( -95.12393327783939867, -297.2967488081391139, -320.3593162127646679 ) ) ;
#22651 = PLANE ( 'NONE',  #33949 ) ;
#22652 = CYLINDRICAL_SURFACE ( 'NONE', #15533, 1.000000000000000888 ) ;
#22653 = CARTESIAN_POINT ( 'NONE',  ( 4.892272440320851068, -287.7171646901823010, -210.3780776303739231 ) ) ;
#22654 = CARTESIAN_POINT ( 'NONE',  ( -110.1307546509781048, -286.0344040821171347, -292.2174348960887187 ) ) ;
#22655 = CARTESIAN_POINT ( 'NONE',  ( 18.74529896702300036, -286.2360095918974139, -223.4572749630345356 ) ) ;
#22656 = CARTESIAN_POINT ( 'NONE',  ( -97.55004068307407294, -276.3623267449929131, -313.0608915440399755 ) ) ;
#22657 = CARTESIAN_POINT ( 'NONE',  ( -108.9464186807513073, -286.1575422643813340, -289.9955221357749338 ) ) ;
#22658 = CARTESIAN_POINT ( 'NONE',  ( -110.6537889255837968, -277.1362267581268952, -262.3869392697350804 ) ) ;
#22659 = CARTESIAN_POINT ( 'NONE',  ( -61.88039495705736925, -278.4582917975523628, -339.4953147396041118 ) ) ;
#22660 = DIRECTION ( 'NONE',  ( 0.000000000000000000, 0.000000000000000000, 1.000000000000000000 ) ) ;
#22661 = CARTESIAN_POINT ( 'NONE',  ( 35.64808926029486713, -275.9887229816575882, -266.1291621752004062 ) ) ;
#22662 = CARTESIAN_POINT ( 'NONE',  ( -7.608933189270027597, -281.2349225782449480, -199.4940308079887643 ) ) ;
#22663 = CARTESIAN_POINT ( 'NONE',  ( 39.46816469795334115, -282.1107011621401739, -275.6504160986082752 ) ) ;
#22664 = ORIENTED_EDGE ( 'NONE', *, *, #70808, .T. ) ;
#22665 = ORIENTED_EDGE ( 'NONE', *, *, #69734, .F. ) ;
#22666 = CARTESIAN_POINT ( 'NONE',  ( 197.7570118961458263, 17.87787486654844571, -10.88803913699953974 ) ) ;
#22667 = CARTESIAN_POINT ( 'NONE',  ( -71.33076387494281789, -291.3565721278113756, -338.0741080922221613 ) ) ;
#22668 = CARTESIAN_POINT ( 'NONE',  ( -95.09709677030082275, -288.5544328190668466, -320.5369331965659399 ) ) ;
#22669 = ADVANCED_FACE ( 'NONE', ( #38962 ), #2547, .F. ) ;
#22670 = CARTESIAN_POINT ( 'NONE',  ( -107.7610049202036038, -295.4875981973454486, -290.2035785117758451 ) ) ;
#22671 = CARTESIAN_POINT ( 'NONE',  ( -8.541687487851248761, -291.7679564255004721, -199.0598412858064705 ) ) ;
#22672 = CARTESIAN_POINT ( 'NONE',  ( 32.04577529113598899, -286.3594122793471684, -295.1821978675232003 ) ) ;
#22673 = CARTESIAN_POINT ( 'NONE',  ( -17.13470088807447667, -290.5563125151219879, -199.1063071835174298 ) ) ;
#22674 = CARTESIAN_POINT ( 'NONE',  ( 29.16330360798184884, -288.3401925010050491, -239.3093067361381543 ) ) ;
#22675 = CARTESIAN_POINT ( 'NONE',  ( -37.30987171927208124, -291.5519495502701943, -345.3611179825600175 ) ) ;
#22676 = CARTESIAN_POINT ( 'NONE',  ( 25.77581920227296663, -290.0990160658569152, -310.9683981270106301 ) ) ;
#22677 = CARTESIAN_POINT ( 'NONE',  ( -7.667696378681542413, -286.6639937676915224, -339.4364524732916948 ) ) ;
#22678 = CARTESIAN_POINT ( 'NONE',  ( -73.90389798382059894, -284.4914329886111091, -333.8745104777723895 ) ) ;
#22679 = CARTESIAN_POINT ( 'NONE',  ( -110.8525252644344903, -292.7540674509536416, -254.6099447103820523 ) ) ;
#22680 = CARTESIAN_POINT ( 'NONE',  ( 82.16961421606863780, -297.9242554544695736, -194.1646132934808406 ) ) ;
#22681 = CARTESIAN_POINT ( 'NONE',  ( 153.8044938463029041, 20.39556813534549207, -12.88425144204669870 ) ) ;
#22682 = CARTESIAN_POINT ( 'NONE',  ( -98.25275556860052006, -275.1346827293161823, -225.9095922126304856 ) ) ;
#22683 = CARTESIAN_POINT ( 'NONE',  ( 35.58909546793568524, -280.8337438970376070, -276.7754495574499742 ) ) ;
#22684 = CARTESIAN_POINT ( 'NONE',  ( -69.89980877123716141, -281.4807601703192859, -337.9398652197405113 ) ) ;
#22685 = CARTESIAN_POINT ( 'NONE',  ( -4.580679678801258703, -293.8286225840001293, -339.8800480576171026 ) ) ;
#22686 = CARTESIAN_POINT ( 'NONE',  ( -111.3541991716151642, -270.8282264253883795, -267.5770889151806955 ) ) ;
#22687 = CARTESIAN_POINT ( 'NONE',  ( 36.45115243676555394, -273.5052900686502539, -260.5667773727956842 ) ) ;
#22688 = CARTESIAN_POINT ( 'NONE',  ( -71.91168270471584378, -298.9002826349354223, -205.4919094356256721 ) ) ;
#22689 = CARTESIAN_POINT ( 'NONE',  ( 159.4851178187871312, 0.000000000000000000, 7.000000000000000000 ) ) ;
#22690 = CARTESIAN_POINT ( 'NONE',  ( -67.84030759116568277, -293.6868567188345764, -339.9585960872456099 ) ) ;
#22691 = CARTESIAN_POINT ( 'NONE',  ( 31.14051418945081551, -295.3363995764118499, -297.4368706813414747 ) ) ;
#22692 = DIRECTION ( 'NONE',  ( 0.000000000000000000, 1.000000000000000000, 0.000000000000000000 ) ) ;
#22693 = CARTESIAN_POINT ( 'NONE',  ( -88.60772221111855629, -296.5964796720023742, -322.6280579143527234 ) ) ;
#22694 = AXIS2_PLACEMENT_3D ( 'NONE', #54742, #24952, #90700 ) ;
#22696 = CARTESIAN_POINT ( 'NONE',  ( -104.7622094669633697, -296.9275086513180213, -242.3704959729346058 ) ) ;
#22695 = CARTESIAN_POINT ( 'NONE',  ( -107.7747926669414085, -282.2241158388961253, -297.2944512803562134 ) ) ;
#22697 = CARTESIAN_POINT ( 'NONE',  ( -93.91973698330325249, -285.2639561508167958, -218.0534269499433719 ) ) ;
#22698 = CARTESIAN_POINT ( 'NONE',  ( -11.17728241618123519, -284.6341085752313234, -341.3020947738959876 ) ) ;
#22699 = VECTOR ( 'NONE', #43051, 1000.000000000000000 ) ;
#22700 = CARTESIAN_POINT ( 'NONE',  ( 22.07656087008093948, -286.5611476350845237, -221.4201887760816021 ) ) ;
#22701 = CARTESIAN_POINT ( 'NONE',  ( -36.15206223956474929, -290.0669091157924413, -195.5244473746655842 ) ) ;
#22702 = CARTESIAN_POINT ( 'NONE',  ( -113.6661288190491490, -277.7780515762037226, -280.1582730972108379 ) ) ;
#22703 = CARTESIAN_POINT ( 'NONE',  ( 31.95455697924147387, -279.4809262143061233, -303.7686719486574134 ) ) ;
#22704 = CARTESIAN_POINT ( 'NONE',  ( -43.49337173925265887, -253.3453352546504220, -491.1732795760416366 ) ) ;
#22705 = CARTESIAN_POINT ( 'NONE',  ( 32.68786815095917575, -286.6387749859839573, -292.5071935587822622 ) ) ;
#22706 = CARTESIAN_POINT ( 'NONE',  ( -51.64120287927517694, -288.1512942791672458, -345.7070981672038101 ) ) ;
#22707 = CARTESIAN_POINT ( 'NONE',  ( -48.18343439339133027, -248.4123448508205172, -430.6442049081568939 ) ) ;
#22708 = CARTESIAN_POINT ( 'NONE',  ( -95.68742849930090699, -279.3073181899726478, -319.7207665702244412 ) ) ;
#22710 = CARTESIAN_POINT ( 'NONE',  ( 17.98332403503773236, -280.5401447333096598, -222.6845076996868045 ) ) ;
#22709 = CARTESIAN_POINT ( 'NONE',  ( -0.2906709608072832740, -292.5821596727428755, -335.9932554481637794 ) ) ;
#22711 = CARTESIAN_POINT ( 'NONE',  ( 36.37030796215024253, -294.0002845385174055, -292.8024803949475086 ) ) ;
#22712 = CARTESIAN_POINT ( 'NONE',  ( -13.14133122367220352, -284.4439798700079791, -198.7813977996833898 ) ) ;
#22713 = CARTESIAN_POINT ( 'NONE',  ( -110.1506655130680343, -280.7840555642916343, -252.3123750123670277 ) ) ;
#22714 = CARTESIAN_POINT ( 'NONE',  ( -53.21200778094138428, -294.3192846342348616, -341.9083191063643312 ) ) ;
#22715 = ORIENTED_EDGE ( 'NONE', *, *, #17571, .F. ) ;
#22716 = DIRECTION ( 'NONE',  ( -0.000000000000000000, 0.000000000000000000, -1.000000000000000000 ) ) ;
#22717 = CARTESIAN_POINT ( 'NONE',  ( 23.43846087917011545, -282.9400340136804743, -227.0296186757534258 ) ) ;
#22718 = CARTESIAN_POINT ( 'NONE',  ( -108.2331318604038017, -296.2934583097169252, -252.6352646284919956 ) ) ;
#22719 = DIRECTION ( 'NONE',  ( 0.000000000000000000, 0.000000000000000000, 1.000000000000000000 ) ) ;
#22720 = CARTESIAN_POINT ( 'NONE',  ( 21.27581636871891391, -273.6952119285918457, -317.1477375740089997 ) ) ;
#22721 = CARTESIAN_POINT ( 'NONE',  ( 19.92237808443723424, -274.0523202826550460, -219.0483142096312008 ) ) ;
#22722 = CARTESIAN_POINT ( 'NONE',  ( -70.21881600624524822, -291.4396067079047725, -205.1837042868152992 ) ) ;
#22723 = CARTESIAN_POINT ( 'NONE',  ( -106.1687192835454852, -280.4223590243038871, -243.8827697135520225 ) ) ;
#22724 = CARTESIAN_POINT ( 'NONE',  ( -40.83296186252206184, -275.6077761908522916, -196.5934976232818769 ) ) ;
#22725 = CARTESIAN_POINT ( 'NONE',  ( -66.25364234098209693, -285.0244795096454595, -340.8772114131485296 ) ) ;
#22726 = EDGE_CURVE ( 'NONE', #77887, #19714, #29065, .T. ) ;
#22727 = CARTESIAN_POINT ( 'NONE',  ( 35.96172176885659155, -280.3957013810674539, -274.0677123757845948 ) ) ;
#22728 = CARTESIAN_POINT ( 'NONE',  ( -32.26029003107166915, -278.9883586160660229, -345.2401208762206579 ) ) ;
#22729 = ORIENTED_EDGE ( 'NONE', *, *, #20778, .F. ) ;
#22730 = CARTESIAN_POINT ( 'NONE',  ( -13.06047496500069371, -274.1924623411498487, -197.2897685419343361 ) ) ;
#22731 = CARTESIAN_POINT ( 'NONE',  ( -65.90161194582250914, -293.5957480110473057, -201.6040033838448267 ) ) ;
#22732 = DIRECTION ( 'NONE',  ( -1.000000000000000000, -0.000000000000000000, -0.000000000000000000 ) ) ;
#22733 = EDGE_CURVE ( 'NONE', #1023, #39404, #23389, .T. ) ;
#22734 = CARTESIAN_POINT ( 'NONE',  ( 154.5625123364532101, 250.0000000000000568, -13.15740740740742254 ) ) ;
#22735 = CARTESIAN_POINT ( 'NONE',  ( -19.59989027179562271, -292.9660803456000622, -344.0733412432311411 ) ) ;
#22736 = CARTESIAN_POINT ( 'NONE',  ( 17.33577515472369512, -274.3672531237997987, -221.8262426903179119 ) ) ;
#22737 = LINE ( 'NONE', #53013, #72289 ) ;
#22738 = CARTESIAN_POINT ( 'NONE',  ( 10.66741075741771816, -294.2216001917107064, -210.9818282037762458 ) ) ;
#22740 = CARTESIAN_POINT ( 'NONE',  ( -72.00637819585742250, -292.8091966474985952, -202.0357678544988573 ) ) ;
#22739 = CARTESIAN_POINT ( 'NONE',  ( 21.31550574532285580, -278.6948066931273615, -317.0979686699210447 ) ) ;
#22741 = CARTESIAN_POINT ( 'NONE',  ( 4.664257116669503489, -290.4842402642510706, -332.3552547765065128 ) ) ;
#22742 = CARTESIAN_POINT ( 'NONE',  ( -15.87882209927194488, -274.7738702344745434, -342.1048748589603861 ) ) ;
#22743 = CARTESIAN_POINT ( 'NONE',  ( 3.952851430080756678, -278.4113567900880071, -332.2971673211025632 ) ) ;
#22744 = CARTESIAN_POINT ( 'NONE',  ( 36.85786856815133206, -291.7093286840240012, -276.3392616079703998 ) ) ;
#22745 = CARTESIAN_POINT ( 'NONE',  ( -69.46064954653174084, -281.4944336589909994, -201.7271460564375047 ) ) ;
#22746 = EDGE_LOOP ( 'NONE', ( #86948, #66806, #23375, #26118, #46624, #65669, #90761, #62261, #88767, #91310, #67034, #88180, #77501, #91529, #62950, #37446, #69460, #12242, #82626, #64739, #73863, #64050, #59671, #38606, #42216 ) ) ;
#22747 = CARTESIAN_POINT ( 'NONE',  ( -13.52647936258182426, -282.4011125619427958, -339.4431566570673908 ) ) ;
#22748 = CARTESIAN_POINT ( 'NONE',  ( -33.94278438221868299, -281.1736391956857801, -193.7455850789679914 ) ) ;
#22749 = CARTESIAN_POINT ( 'NONE',  ( 23.92823234629980433, -280.9622221717011143, -316.3394182371355328 ) ) ;
#22750 = CARTESIAN_POINT ( 'NONE',  ( 14.73239419996653332, -277.2815191724564556, -326.8347959583882130 ) ) ;
#22751 = CARTESIAN_POINT ( 'NONE',  ( 0.000000000000000000, 0.000000000000000000, 0.000000000000000000 ) ) ;
#22752 = CARTESIAN_POINT ( 'NONE',  ( 26.34117372993448924, -276.5144197671795609, -228.3230479796506529 ) ) ;
#22753 = CIRCLE ( 'NONE', #27305, 0.5000000000000022204 ) ;
#22754 = CARTESIAN_POINT ( 'NONE',  ( -53.28691492658256834, -291.7662352645559167, -340.3683826091709079 ) ) ;
#22755 = ORIENTED_EDGE ( 'NONE', *, *, #65290, .T. ) ;
#22756 = B_SPLINE_CURVE_WITH_KNOTS ( 'NONE', 3,
 ( #32652, #34051, #26476, #10846, #69559, #4688, #39710, #77604, #3767, #40181 ),
 .UNSPECIFIED., .F., .F.,
 ( 4, 2, 2, 2, 4 ),
 ( 0.000000000000000000, 0.04477231361816515209, 0.08954462723633030419, 0.1343169408544954702, 0.1790892544726606084 ),
 .UNSPECIFIED. ) ;
#22757 = ORIENTED_EDGE ( 'NONE', *, *, #67229, .T. ) ;
#22758 = CARTESIAN_POINT ( 'NONE',  ( -68.91200057829905745, -299.6372711141936520, -202.3153437795381535 ) ) ;
#22759 = CIRCLE ( 'NONE', #84741, 1.999999999999998002 ) ;
#22760 = CARTESIAN_POINT ( 'NONE',  ( -30.79299449257197807, -293.2165522940872506, -197.3450887278570463 ) ) ;
#22761 = CARTESIAN_POINT ( 'NONE',  ( -97.43176018785064230, -275.9650703533350793, -314.6660869604590403 ) ) ;
#22762 = CARTESIAN_POINT ( 'NONE',  ( -97.55915349704285688, -292.9391401709866045, -223.9953431056200941 ) ) ;
#22763 = CARTESIAN_POINT ( 'NONE',  ( -28.08522986115089637, -291.5211917964301733, -197.7967795870209784 ) ) ;
#22764 = EDGE_CURVE ( 'NONE', #16725, #72158, #12429, .T. ) ;
#22765 = CARTESIAN_POINT ( 'NONE',  ( -1.834701946944296225, -288.1021422454562071, -338.6163740701982192 ) ) ;
#22766 = CARTESIAN_POINT ( 'NONE',  ( 154.5625123364532101, 275.5000000000000568, 13.15740740740740833 ) ) ;
#22768 = CARTESIAN_POINT ( 'NONE',  ( -64.36709589736504711, -281.8107076448854400, -339.0347548387805432 ) ) ;
#22767 = CARTESIAN_POINT ( 'NONE',  ( 34.90151646025780963, -291.8089060723391412, -245.3106039014988937 ) ) ;
#22769 = CARTESIAN_POINT ( 'NONE',  ( -93.32793867447479386, -291.7283439639663811, -319.1863069001528288 ) ) ;
#22770 = CARTESIAN_POINT ( 'NONE',  ( -109.8720068664262755, -283.2033640286816762, -257.2494340120659331 ) ) ;
#22771 = CARTESIAN_POINT ( 'NONE',  ( -64.22024288570915473, -284.7255395279689196, -338.7627803713127719 ) ) ;
#22772 = ORIENTED_EDGE ( 'NONE', *, *, #49942, .F. ) ;
#22773 = CARTESIAN_POINT ( 'NONE',  ( -40.31759989762937835, -290.0299206082618753, -347.0811623483997437 ) ) ;
#22774 = CARTESIAN_POINT ( 'NONE',  ( -16.91050925244443448, -280.8155941523984325, -200.2144510560181345 ) ) ;
#22775 = CARTESIAN_POINT ( 'NONE',  ( -13.97290882141705914, -291.1435456870715370, -197.3540172353421269 ) ) ;
#22776 = CARTESIAN_POINT ( 'NONE',  ( -12.76505267549691958, -287.1665277195018575, -197.5590079843245519 ) ) ;
#22777 = CARTESIAN_POINT ( 'NONE',  ( 34.79435364268214670, -287.7059417146654141, -243.6044991845759284 ) ) ;
#22778 = CARTESIAN_POINT ( 'NONE',  ( -97.35715053496559790, -285.2980992667718851, -228.7800786883462933 ) ) ;
#22779 = ORIENTED_EDGE ( 'NONE', *, *, #29447, .T. ) ;
#22780 = CARTESIAN_POINT ( 'NONE',  ( 193.9402003287077605, 249.5000000000000568, 16.58062614384823874 ) ) ;
#22781 = CARTESIAN_POINT ( 'NONE',  ( 27.06853868113006456, -295.9439221579730770, -310.3549262581429389 ) ) ;
#22782 = CARTESIAN_POINT ( 'NONE',  ( -33.47660968079976840, -293.6893154319278096, -346.7833109541220438 ) ) ;
#22783 = CARTESIAN_POINT ( 'NONE',  ( -79.17950020349032059, -278.5307175752861895, -210.2528246079047847 ) ) ;
#22784 = CARTESIAN_POINT ( 'NONE',  ( -89.53302443627046614, -296.6883992669565941, -213.8144110142056036 ) ) ;
#22785 = CARTESIAN_POINT ( 'NONE',  ( -0.8971089609653338792, -291.0252516736392181, -206.2957458962374631 ) ) ;
#22786 = CARTESIAN_POINT ( 'NONE',  ( -111.0574343037965406, -294.8854469085159167, -263.1793407518790673 ) ) ;
#22787 = CARTESIAN_POINT ( 'NONE',  ( 33.83486101183537897, -294.9924159393723926, -288.2783624762129193 ) ) ;
#22788 = CARTESIAN_POINT ( 'NONE',  ( 34.24870465095800398, -294.4237640906870297, -254.5221191405164802 ) ) ;
#22789 = CARTESIAN_POINT ( 'NONE',  ( 219.8344101925596021, 3.000000000000000000, 10.00000000000000000 ) ) ;
#22790 = CARTESIAN_POINT ( 'NONE',  ( 0.8162758624145598496, -292.5442274639501079, -335.1221965322361029 ) ) ;
#22791 = CARTESIAN_POINT ( 'NONE',  ( -101.4668613245127347, -298.0298803328688564, -309.3560345559305915 ) ) ;
#22792 = CARTESIAN_POINT ( 'NONE',  ( -108.3395303076698326, -291.7303467748802746, -252.3457680708250450 ) ) ;
#22793 = EDGE_CURVE ( 'NONE', #29874, #9616, #86552, .T. ) ;
#22794 = CARTESIAN_POINT ( 'NONE',  ( -69.72963153454597318, -295.8241083238206102, -335.8065867797317878 ) ) ;
#22795 = ADVANCED_FACE ( 'NONE', ( #3461 ), #59853, .F. ) ;
#22796 = CARTESIAN_POINT ( 'NONE',  ( -110.8737549414448438, -280.3214923827876532, -286.8366672158840629 ) ) ;
#22797 = CARTESIAN_POINT ( 'NONE',  ( -110.8587005888958146, -277.5042360618326711, -249.1821445290698591 ) ) ;
#22798 = VERTEX_POINT ( 'NONE', #32356 ) ;
#22799 = CARTESIAN_POINT ( 'NONE',  ( -102.6281135752596612, -272.4330257089519023, -229.7286555217281148 ) ) ;
#22800 = CARTESIAN_POINT ( 'NONE',  ( -0.5613685635308771626, -280.6391429359832728, -335.0799051208878154 ) ) ;
#22801 = CARTESIAN_POINT ( 'NONE',  ( -113.5770022875950360, -276.9726275541875680, -268.7308133519520652 ) ) ;
#22802 = CARTESIAN_POINT ( 'NONE',  ( -25.65490631274033007, -278.2005651184741737, -196.1085269536625901 ) ) ;
#22803 = CARTESIAN_POINT ( 'NONE',  ( -68.23968605179433666, -296.3224740033879243, -203.6648462538233275 ) ) ;
#22804 = CARTESIAN_POINT ( 'NONE',  ( -11.88347930468330205, -276.3835672010429789, -199.7597039274096744 ) ) ;
#22805 = CARTESIAN_POINT ( 'NONE',  ( 143.6449502718966755, 0.000000000000000000, -47.19625681453479871 ) ) ;
#22806 = CARTESIAN_POINT ( 'NONE',  ( -111.0262047432414505, -288.7746597923503487, -254.5205847825237697 ) ) ;
#22807 = CARTESIAN_POINT ( 'NONE',  ( -36.08684223591867379, -289.0368599404415590, -347.3640025296235194 ) ) ;
#22808 = CARTESIAN_POINT ( 'NONE',  ( 33.98207351173908108, -277.2444477820234283, -246.4706957618994636 ) ) ;
#22809 = CARTESIAN_POINT ( 'NONE',  ( -44.72524722593194468, -295.9584584440430035, -195.8412787701375635 ) ) ;
#22810 = CARTESIAN_POINT ( 'NONE',  ( -32.30676869908135274, -285.3112654799778056, -193.6745922750766340 ) ) ;
#22811 = DIRECTION ( 'NONE',  ( 0.000000000000000000, -1.000000000000000000, 0.000000000000000000 ) ) ;
#22812 = CARTESIAN_POINT ( 'NONE',  ( 35.63726443635285079, -279.7746893963228558, -287.7093475087763750 ) ) ;
#22813 =( BOUNDED_CURVE ( )  B_SPLINE_CURVE ( 3, ( #20787, #49659, #77615, #64387 ),
 .UNSPECIFIED., .F., .F. ) 
 B_SPLINE_CURVE_WITH_KNOTS ( ( 4, 4 ),
 ( 0.000000000000000000, 1.570796326794896558 ),
 .UNSPECIFIED. ) 
 CURVE ( )  GEOMETRIC_REPRESENTATION_ITEM ( )  RATIONAL_B_SPLINE_CURVE ( ( 1.000000000000000000, 0.8047378541243649375, 0.8047378541243649375, 1.000000000000000000 ) ) 
 REPRESENTATION_ITEM ( '' )  );
#22814 = CARTESIAN_POINT ( 'NONE',  ( 199.8090428943486643, 25.00736135706073426, 10.14950798392827558 ) ) ;
#22815 = CARTESIAN_POINT ( 'NONE',  ( 29.10448190937588109, -291.9267881195015661, -239.0636326948262820 ) ) ;
#22816 = CARTESIAN_POINT ( 'NONE',  ( -84.41310688868244938, -283.5362906318811156, -212.8909640408337793 ) ) ;
#22817 = CARTESIAN_POINT ( 'NONE',  ( 207.7761861081325776, 35.69891260691534285, 14.41714557868295010 ) ) ;
#22818 = FILL_AREA_STYLE ('',( #87668 ) ) ;
#22819 = CARTESIAN_POINT ( 'NONE',  ( 35.59865740017828273, -291.3272050173316075, -252.8503742251963047 ) ) ;
#22820 = CARTESIAN_POINT ( 'NONE',  ( -110.9648532524177966, -280.0765960735530484, -276.1618340421539415 ) ) ;
#22821 = CARTESIAN_POINT ( 'NONE',  ( -71.54759087307321863, -284.6990428877417116, -338.9028261502468808 ) ) ;
#22823 = CARTESIAN_POINT ( 'NONE',  ( -106.5323114736921326, -284.8631950325906814, -246.9292609112477805 ) ) ;
#22822 = CARTESIAN_POINT ( 'NONE',  ( -21.62990425952631668, -272.3319021090456431, -196.4527039436227938 ) ) ;
#22824 =( BOUNDED_CURVE ( )  B_SPLINE_CURVE ( 3, ( #59992, #22581, #30163, #66616 ),
 .UNSPECIFIED., .F., .F. ) 
 B_SPLINE_CURVE_WITH_KNOTS ( ( 4, 4 ),
 ( 1.570796326794433151, 4.712388980385153303 ),
 .UNSPECIFIED. ) 
 CURVE ( )  GEOMETRIC_REPRESENTATION_ITEM ( )  RATIONAL_B_SPLINE_CURVE ( ( 1.000000000000000000, 0.3333333333330242843, 0.3333333333330242843, 1.000000000000000000 ) ) 
 REPRESENTATION_ITEM ( '' )  );
#22825 = CARTESIAN_POINT ( 'NONE',  ( 28.37943907704037727, -276.5316721041541541, -237.2536146483415678 ) ) ;
#22826 = CARTESIAN_POINT ( 'NONE',  ( -7.432304353985270673, -277.4524491857194448, -337.1295968617869789 ) ) ;
#22827 = CARTESIAN_POINT ( 'NONE',  ( -102.3207591046432583, -287.0533518841056662, -232.8048436453463239 ) ) ;
#22828 = ORIENTED_EDGE ( 'NONE', *, *, #81728, .F. ) ;
#22829 = DIRECTION ( 'NONE',  ( 0.000000000000000000, 0.000000000000000000, 1.000000000000000000 ) ) ;
#22830 = CARTESIAN_POINT ( 'NONE',  ( -113.2042502678440741, -296.2167936307116065, -283.8485727529573523 ) ) ;
#22832 = CARTESIAN_POINT ( 'NONE',  ( 19.00151691237411100, -288.8493686725484508, -221.3990030523627013 ) ) ;
#22831 = VECTOR ( 'NONE', #68273, 1000.000000000000000 ) ;
#22833 = DIRECTION ( 'NONE',  ( 0.000000000000000000, 0.000000000000000000, -1.000000000000000000 ) ) ;
#22834 = CARTESIAN_POINT ( 'NONE',  ( -119.3990491898856732, -294.0523547857346784, -270.3284710469131937 ) ) ;
#22835 = CARTESIAN_POINT ( 'NONE',  ( -98.32217382835952435, -278.0952094886043824, -223.8330176317634255 ) ) ;
#22836 = CARTESIAN_POINT ( 'NONE',  ( -16.82225183866680496, -290.7127568243128053, -196.9758833949151438 ) ) ;
#22837 = VECTOR ( 'NONE', #38804, 1000.000000000000000 ) ;
#22838 = CARTESIAN_POINT ( 'NONE',  ( 34.69248652820068912, -289.2761949266253509, -285.9697713353139648 ) ) ;
#22839 = CARTESIAN_POINT ( 'NONE',  ( -106.4686551089934170, -280.6623396288676986, -243.7705632818004062 ) ) ;
#22840 = CARTESIAN_POINT ( 'NONE',  ( 7.602705703670109116, -289.8777964016595092, -332.2212524178387412 ) ) ;
#22841 = CARTESIAN_POINT ( 'NONE',  ( 11.22261843696981209, -284.3800312508116122, -327.5828045920850400 ) ) ;
#22842 = CARTESIAN_POINT ( 'NONE',  ( -89.21054873758203030, -277.9251035745185163, -327.2700149004718924 ) ) ;
#22843 = CARTESIAN_POINT ( 'NONE',  ( -67.46039558916896794, -295.6752633816268485, -202.0484428998865667 ) ) ;
#22844 = CARTESIAN_POINT ( 'NONE',  ( -69.96044476446304827, -279.4676661538749727, -200.5970513612901414 ) ) ;
#22845 = CARTESIAN_POINT ( 'NONE',  ( -67.58200756528542286, -275.5115775192335263, -202.5505148680412049 ) ) ;
#22846 = CARTESIAN_POINT ( 'NONE',  ( 196.9883954656811227, 295.9476850007761186, -7.765551635011542331 ) ) ;
#22847 = CARTESIAN_POINT ( 'NONE',  ( 21.27581636871892101, -289.4090924074130839, -223.5744983911110353 ) ) ;
#22848 = EDGE_CURVE ( 'NONE', #21957, #32677, #6490, .T. ) ;
#22849 = CARTESIAN_POINT ( 'NONE',  ( -98.73490887853469644, -271.3952536205675301, -225.4983732049233254 ) ) ;
#22850 = DIRECTION ( 'NONE',  ( -1.000000000000000000, 0.000000000000000000, 0.000000000000000000 ) ) ;
#22851 = CARTESIAN_POINT ( 'NONE',  ( -57.12385550252515287, -279.2975952226574918, -200.0286591159144791 ) ) ;
#22852 = CARTESIAN_POINT ( 'NONE',  ( 28.15503812785641102, -276.2348025467925368, -230.5333556394868140 ) ) ;
#22853 = CARTESIAN_POINT ( 'NONE',  ( -31.66568236574773110, -282.0409348993216554, -346.9289209039087041 ) ) ;
#22854 = CARTESIAN_POINT ( 'NONE',  ( -56.30387553490361086, -291.0598309202619589, -341.9574636689927729 ) ) ;
#22855 = CARTESIAN_POINT ( 'NONE',  ( -98.54800878943147779, -298.6840714951786140, -224.7707226745167475 ) ) ;
#22856 = CARTESIAN_POINT ( 'NONE',  ( -3.643216289488539594, -299.6703060159638881, -193.7514583082898980 ) ) ;
#22857 = CARTESIAN_POINT ( 'NONE',  ( 36.12906626429139578, -295.7352411283621905, -284.5764236440898003 ) ) ;
#22858 = CARTESIAN_POINT ( 'NONE',  ( 34.88970170094819423, -279.2993518203380745, -250.7505102836038873 ) ) ;
#22859 = CARTESIAN_POINT ( 'NONE',  ( -8.308312740321206036, -272.4541422371714248, -201.5389169675738117 ) ) ;
#22860 = CARTESIAN_POINT ( 'NONE',  ( 23.21315494456706574, -288.5288294261599162, -224.0844620599828261 ) ) ;
#22861 = EDGE_CURVE ( 'NONE', #64125, #20191, #29124, .T. ) ;
#22862 = CARTESIAN_POINT ( 'NONE',  ( -80.60094962465606727, -288.5743577796425825, -329.6092881494023459 ) ) ;
#22863 = CARTESIAN_POINT ( 'NONE',  ( 204.7385621006099257, 294.9048254156659823, -54.00000000002585665 ) ) ;
#22864 = ORIENTED_EDGE ( 'NONE', *, *, #6869, .F. ) ;
#22865 = CARTESIAN_POINT ( 'NONE',  ( -62.58624418680784629, -287.9489336413535057, -342.5372485129394704 ) ) ;
#22866 = CARTESIAN_POINT ( 'NONE',  ( 21.97639084872056614, -287.8140071819120180, -312.9457580501953089 ) ) ;
#22867 = ORIENTED_EDGE ( 'NONE', *, *, #45976, .T. ) ;
#22868 = CARTESIAN_POINT ( 'NONE',  ( -37.99366749977676960, -287.1238288974059856, -193.6729999342475423 ) ) ;
#22869 = CARTESIAN_POINT ( 'NONE',  ( -6.263773649677868427, -276.9655234373737471, -336.4524965866945081 ) ) ;
#22870 = CARTESIAN_POINT ( 'NONE',  ( -6.000628894711874217, -291.3748327941144112, -200.3523874316296371 ) ) ;
#22871 = CARTESIAN_POINT ( 'NONE',  ( -1.674044572686927523, -283.2434110234169680, -338.4869657503185181 ) ) ;
#22872 = CARTESIAN_POINT ( 'NONE',  ( 12.52433140809071865, -282.2526717859820451, -212.6022515651207812 ) ) ;
#22873 = CARTESIAN_POINT ( 'NONE',  ( -67.86906395222227673, -283.7753189327724499, -341.0281141655796091 ) ) ;
#22874 = CARTESIAN_POINT ( 'NONE',  ( -41.05650413763851247, -280.3373952814051222, -197.4345266869805755 ) ) ;
#22875 = CARTESIAN_POINT ( 'NONE',  ( -114.2704648735229114, -276.0523547857348490, -270.3284710469133074 ) ) ;
#22876 = CARTESIAN_POINT ( 'NONE',  ( -107.5233622349960143, -262.7998339567401445, -317.7199647377577776 ) ) ;
#22877 = EDGE_LOOP ( 'NONE', ( #47031, #76243, #24143, #36824 ) ) ;
#22878 = CARTESIAN_POINT ( 'NONE',  ( -96.71237328335487859, -279.9270754022212486, -315.9149498662736733 ) ) ;
#22879 = CARTESIAN_POINT ( 'NONE',  ( -84.92918389587137540, -218.7266517812545601, -351.7339122337344861 ) ) ;
#22880 = CARTESIAN_POINT ( 'NONE',  ( 83.26066877736924710, 82.48078560638359136, -299.1889401045851287 ) ) ;
#22881 = CARTESIAN_POINT ( 'NONE',  ( -37.81486326515116758, -297.3946560319042192, -197.2607158959976346 ) ) ;
#22882 = CARTESIAN_POINT ( 'NONE',  ( 28.05031060861441361, -293.5915381554420946, -311.0002138651627206 ) ) ;
#22883 = CARTESIAN_POINT ( 'NONE',  ( -110.5520848501708855, -271.4739283423095344, -283.6991303856082709 ) ) ;
#22885 = CARTESIAN_POINT ( 'NONE',  ( -109.1333380604779109, -288.7288743595184997, -287.4608589319041698 ) ) ;
#22884 = CARTESIAN_POINT ( 'NONE',  ( -108.7005367908344198, -271.5903782609459540, -242.6252554518754607 ) ) ;
#22886 = CARTESIAN_POINT ( 'NONE',  ( -106.0971639671342928, -298.0438304111626735, -298.3531109505069026 ) ) ;
#22887 = CARTESIAN_POINT ( 'NONE',  ( -8.006353524199305127, -289.9749296745324614, -337.8001041016131012 ) ) ;
#22888 = ORIENTED_EDGE ( 'NONE', *, *, #81666, .F. ) ;
#22889 = CARTESIAN_POINT ( 'NONE',  ( 8.774395754089230337, -295.3782415246955111, -331.7298878324195357 ) ) ;
#22890 = CARTESIAN_POINT ( 'NONE',  ( 0.1949017428794037610, -287.0585737428667699, -207.6204676616511904 ) ) ;
#22891 = CARTESIAN_POINT ( 'NONE',  ( -48.89487286685766065, -296.7031806015959887, -194.5810305377431746 ) ) ;
#22892 = CARTESIAN_POINT ( 'NONE',  ( 1.609407422514420372, -293.3614706655782811, -204.0661102242755192 ) ) ;
#22893 = CARTESIAN_POINT ( 'NONE',  ( 29.41913012166305563, -293.5472216982245754, -232.1182304418038029 ) ) ;
#22894 = CARTESIAN_POINT ( 'NONE',  ( -36.20825930646101654, -292.2333990132634085, -197.3574412278100567 ) ) ;
#22895 = ORIENTED_EDGE ( 'NONE', *, *, #55843, .F. ) ;
#22896 = CARTESIAN_POINT ( 'NONE',  ( -111.0442044302446618, -274.6845124885824134, -253.7101401615071836 ) ) ;
#22897 = CARTESIAN_POINT ( 'NONE',  ( 38.10372819436256009, -274.1793635155243578, -257.0197307579413746 ) ) ;
#22898 = ORIENTED_EDGE ( 'NONE', *, *, #86333, .F. ) ;
#22899 = CARTESIAN_POINT ( 'NONE',  ( -5.316111143675319006, -276.1495667217936898, -340.3174511746917119 ) ) ;
#22900 = CARTESIAN_POINT ( 'NONE',  ( -107.9560938384698261, -271.2350164550532554, -248.7375006393052672 ) ) ;
#22901 = CARTESIAN_POINT ( 'NONE',  ( -13.40922665110629453, -274.8777730879430123, -340.6867792316156738 ) ) ;
#22902 = CARTESIAN_POINT ( 'NONE',  ( 95.29650580809318683, -300.9540312850523378, -196.9362300929560945 ) ) ;
#22903 = CARTESIAN_POINT ( 'NONE',  ( -29.97808937807558038, -275.0888931880960513, -197.4969588592658738 ) ) ;
#22904 = CARTESIAN_POINT ( 'NONE',  ( -9.495033719286549712, -299.9954019213857919, -194.1536752346991648 ) ) ;
#22905 = VECTOR ( 'NONE', #10267, 1000.000000000000000 ) ;
#22906 = CARTESIAN_POINT ( 'NONE',  ( -80.29176131480143397, -271.4941183381000087, -208.3810282358067241 ) ) ;
#22907 = CARTESIAN_POINT ( 'NONE',  ( -58.42972677395699321, -295.9835123121719107, -340.3553163143595839 ) ) ;
#22908 = CARTESIAN_POINT ( 'NONE',  ( -12.82894162297253082, -293.3020599748949735, -339.8013953134497456 ) ) ;
#22909 = DIRECTION ( 'NONE',  ( 0.000000000000000000, 0.000000000000000000, 1.000000000000000000 ) ) ;
#22910 = CARTESIAN_POINT ( 'NONE',  ( 18.86254208852871272, -276.7616678237225756, -322.9026259556976584 ) ) ;
#22911 = EDGE_CURVE ( 'NONE', #58673, #7585, #52708, .T. ) ;
#22912 = CARTESIAN_POINT ( 'NONE',  ( -48.87752903021296191, -274.0679296571243526, -198.2271817964278853 ) ) ;
#22913 = CARTESIAN_POINT ( 'NONE',  ( -112.6545574498353517, -283.0638493678085297, -284.1160664332224997 ) ) ;
#22914 = CARTESIAN_POINT ( 'NONE',  ( -66.19653985408517372, -297.4290927373858722, -339.7826635079074435 ) ) ;
#22915 = CARTESIAN_POINT ( 'NONE',  ( 160.5350683151633291, 215.0000000000000568, 20.22542485937379908 ) ) ;
#22916 = CARTESIAN_POINT ( 'NONE',  ( -67.60517963137860420, -284.8417675753788103, -203.7523833015337118 ) ) ;
#22917 = CARTESIAN_POINT ( 'NONE',  ( -96.09085878621074528, -276.1673820875641354, -315.3778967769584938 ) ) ;
#22918 = CARTESIAN_POINT ( 'NONE',  ( -109.8698891021753639, -276.9629605387547713, -282.8870801509284547 ) ) ;
#22919 = CARTESIAN_POINT ( 'NONE',  ( -12.09036619058301376, -284.7238632199299673, -341.0363372823140367 ) ) ;
#22920 = CARTESIAN_POINT ( 'NONE',  ( 33.89085614128760682, -276.5250112258291892, -252.6678019186929305 ) ) ;
#22921 = CARTESIAN_POINT ( 'NONE',  ( 207.6662022560301182, 36.29800326561209545, 14.90057469441957316 ) ) ;
#22922 = CARTESIAN_POINT ( 'NONE',  ( 29.82814540138188519, -274.4232409526422884, -306.4537523632698708 ) ) ;
#22923 = CARTESIAN_POINT ( 'NONE',  ( -12.14840405729502137, -282.3792223695888310, -199.4875086002994919 ) ) ;
#22924 = DIRECTION ( 'NONE',  ( -1.000000000000000000, -0.000000000000000000, -0.000000000000000000 ) ) ;
#22925 = CARTESIAN_POINT ( 'NONE',  ( 17.29305766490441698, -288.7442011317996275, -218.0903091792585258 ) ) ;
#22926 =( NAMED_UNIT ( * ) SI_UNIT ( $, .STERADIAN. ) SOLID_ANGLE_UNIT ( ) );
#22927 = CARTESIAN_POINT ( 'NONE',  ( -102.1350131748652927, -288.0462287910465875, -308.2362795624047749 ) ) ;
#22928 = LINE ( 'NONE', #23410, #36160 ) ;
#22929 = CARTESIAN_POINT ( 'NONE',  ( -35.78972779189328435, -296.8669275165477757, -196.9643687994915524 ) ) ;
#22930 = CARTESIAN_POINT ( 'NONE',  ( -111.3561666106230632, -288.6093401080416356, -276.7123986008949146 ) ) ;
#22931 = CARTESIAN_POINT ( 'NONE',  ( 61.48257290429442889, 47.14312216093964025, -312.8229988924202871 ) ) ;
#22932 = CARTESIAN_POINT ( 'NONE',  ( 208.3418117619747818, 38.42745601219718310, 12.00000000000000000 ) ) ;
#22933 = CARTESIAN_POINT ( 'NONE',  ( 22.46070306245089299, -285.3918514258581922, -222.9442895481464859 ) ) ;
#22934 = CARTESIAN_POINT ( 'NONE',  ( -48.42897952224370073, -284.7957664921333389, -343.3235237083409856 ) ) ;
#22935 = CARTESIAN_POINT ( 'NONE',  ( -80.34600888977716693, -283.7185653825162035, -207.6509628155010034 ) ) ;
#22936 = CARTESIAN_POINT ( 'NONE',  ( 17.48982983209532449, -282.2808244831265370, -221.2807936141313121 ) ) ;
#22937 = CARTESIAN_POINT ( 'NONE',  ( 20.31452793060773487, -282.9883822624314007, -315.3984479830546093 ) ) ;
#22938 = CARTESIAN_POINT ( 'NONE',  ( -34.69870929487166222, -290.9989806303004798, -345.6699581337700806 ) ) ;
#22939 = CARTESIAN_POINT ( 'NONE',  ( -94.13253428802087797, -273.5926075519712413, -218.3748818926861475 ) ) ;
#22940 = CARTESIAN_POINT ( 'NONE',  ( 31.54190348104442165, -286.0362430933452060, -301.4153181661799863 ) ) ;
#22941 = CARTESIAN_POINT ( 'NONE',  ( 4.863160820755996205, -274.6050010984182563, -205.8948307274026490 ) ) ;
#22942 = CARTESIAN_POINT ( 'NONE',  ( 36.46817474507574275, -295.6800233298317835, -281.8313114947656572 ) ) ;
#22943 = CARTESIAN_POINT ( 'NONE',  ( -48.18343439339131606, -253.2159931059841256, -461.7098312862314629 ) ) ;
#22944 = CARTESIAN_POINT ( 'NONE',  ( 31.03373250439201669, -301.4082689599840705, -195.3320873922940848 ) ) ;
#22945 = CARTESIAN_POINT ( 'NONE',  ( -66.77233571673012591, -282.1308321146674416, -337.7177936702101420 ) ) ;
#22946 = CARTESIAN_POINT ( 'NONE',  ( -112.5509510421484407, -276.5367145921179599, -271.5532795534923025 ) ) ;
#22947 = CARTESIAN_POINT ( 'NONE',  ( -91.66179662871803657, -271.7748953214217522, -216.7697486382825502 ) ) ;
#22948 = CARTESIAN_POINT ( 'NONE',  ( 31.21678539507831829, -274.5629146278374719, -244.9913184014182832 ) ) ;
#22949 = CARTESIAN_POINT ( 'NONE',  ( -14.65113616183396950, -293.8717674158717159, -200.2480232123132566 ) ) ;
#22950 = CARTESIAN_POINT ( 'NONE',  ( 35.07247113035655417, -294.6415507602708885, -281.6273338381378721 ) ) ;
#22951 = CARTESIAN_POINT ( 'NONE',  ( -111.3228750145086394, -286.3406870128762876, -268.1794274846537860 ) ) ;
#22952 = CARTESIAN_POINT ( 'NONE',  ( 8.482944460584493029, -294.0908240747454556, -209.1501151698160186 ) ) ;
#22953 = CARTESIAN_POINT ( 'NONE',  ( 39.16223351306230427, -294.8305394199445004, -267.4386253259762043 ) ) ;
#22954 = CARTESIAN_POINT ( 'NONE',  ( -109.0452700252175049, -296.5670311119403095, -256.5979082342217907 ) ) ;
#22955 = CARTESIAN_POINT ( 'NONE',  ( -111.1425255844403210, -292.3807953661203669, -283.7192171284036704 ) ) ;
#22956 = CARTESIAN_POINT ( 'NONE',  ( -111.8744294936991679, -284.4762362498173047, -289.7491621985259940 ) ) ;
#22957 = CARTESIAN_POINT ( 'NONE',  ( -72.58675008682091345, -295.6695041169023739, -203.4670124633767045 ) ) ;
#22958 = CARTESIAN_POINT ( 'NONE',  ( -114.2084971262152067, -284.3185065081116818, -275.7156657377469173 ) ) ;
#22959 = CARTESIAN_POINT ( 'NONE',  ( -24.01165265740753085, -278.8610975586097993, -343.8586529574663473 ) ) ;
#22960 = CARTESIAN_POINT ( 'NONE',  ( -91.80561436760662275, -284.0486309817471806, -221.0847036836681241 ) ) ;
#22961 = CARTESIAN_POINT ( 'NONE',  ( 36.99639573262543735, -285.4243330106365306, -260.4188771728639722 ) ) ;
#22962 = CARTESIAN_POINT ( 'NONE',  ( -53.47399151803750783, -277.9870680884278045, -196.2800364275581728 ) ) ;
#22964 = AXIS2_PLACEMENT_3D ( 'NONE', #21630, #41986, #14991 ) ;
#22963 = CARTESIAN_POINT ( 'NONE',  ( 202.9738562182569694, 296.4636489450776367, -53.99999999999997868 ) ) ;
#22965 = CARTESIAN_POINT ( 'NONE',  ( -81.51080159783965939, -284.9400560793508248, -212.1625018751630591 ) ) ;
#22966 = COLOUR_RGB ( '',0.7921568627450980005, 0.8196078431372548767, 0.9333333333333333481 ) ;
#22967 = CARTESIAN_POINT ( 'NONE',  ( 39.13381660647873872, -282.8233149462358256, -275.6182787201078099 ) ) ;
#22968 = CARTESIAN_POINT ( 'NONE',  ( -5.734359013657527093, -287.7053336863788786, -340.3167911008455917 ) ) ;
#22969 = CARTESIAN_POINT ( 'NONE',  ( -86.56274151179913190, -279.3225764183724777, -328.5999738795804888 ) ) ;
#22970 = CARTESIAN_POINT ( 'NONE',  ( 7.962606359018053581, -277.7629737672214674, -332.0774945443131401 ) ) ;
#22971 = CARTESIAN_POINT ( 'NONE',  ( -54.49072983551907612, -279.6590751916525051, -199.3518160029029787 ) ) ;
#22972 = CARTESIAN_POINT ( 'NONE',  ( -18.88886148336236559, -276.2706384674692686, -197.9795143481037485 ) ) ;
#22973 = CARTESIAN_POINT ( 'NONE',  ( 35.48641470901812056, -293.8690876775477250, -295.5258246053791140 ) ) ;
#22974 = CARTESIAN_POINT ( 'NONE',  ( 33.11721102769511305, -285.8794511299716419, -295.5716368973623958 ) ) ;
#22975 = VECTOR ( 'NONE', #82780, 1000.000000000000000 ) ;
#22976 = CARTESIAN_POINT ( 'NONE',  ( -53.24248247744834828, -293.4518036238951026, -195.7846667730574097 ) ) ;
#22977 = CARTESIAN_POINT ( 'NONE',  ( -35.65723826049037370, -293.9508856762885216, -343.6634254068538894 ) ) ;
#22978 = CARTESIAN_POINT ( 'NONE',  ( 1.577513483448755194, -294.1832471369779114, -332.2059690744101772 ) ) ;
#22979 = CARTESIAN_POINT ( 'NONE',  ( -74.54104606260183630, -292.6488187284438141, -203.2962152976063521 ) ) ;
#22980 = CARTESIAN_POINT ( 'NONE',  ( 13.39989437834137753, -281.4362347407014795, -217.6675544099526292 ) ) ;
#22981 = CARTESIAN_POINT ( 'NONE',  ( -113.9453354313073845, -271.6827742692142920, -264.6318282315379520 ) ) ;
#22982 = CARTESIAN_POINT ( 'NONE',  ( 31.59971973709275161, -288.6432405057769301, -304.5457832979413411 ) ) ;
#22983 = CARTESIAN_POINT ( 'NONE',  ( 16.92475570159112763, -280.4292092753884731, -323.3081412820886271 ) ) ;
#22984 = CARTESIAN_POINT ( 'NONE',  ( -20.49689700323688513, -289.1749494576038728, -345.5289982074760928 ) ) ;
#22985 = CARTESIAN_POINT ( 'NONE',  ( -25.14246470401097255, -286.5451444338183364, -198.3149018609613847 ) ) ;
#22986 = CARTESIAN_POINT ( 'NONE',  ( 160.7988830096749382, 220.5294184115326459, -205.1624142896263550 ) ) ;
#22987 = CARTESIAN_POINT ( 'NONE',  ( -78.98035441448926974, -207.4150709411190689, -355.2989178682290685 ) ) ;
#22988 = CARTESIAN_POINT ( 'NONE',  ( 188.5977483363980127, 268.2578132117691894, -137.4814016061846189 ) ) ;
#22989 = CARTESIAN_POINT ( 'NONE',  ( -95.73446723578864237, -278.3673783251171017, -226.2621407561551052 ) ) ;
#22990 = CARTESIAN_POINT ( 'NONE',  ( -109.3494968692206868, -277.2909654271063005, -284.1789922881871462 ) ) ;
#22991 = CARTESIAN_POINT ( 'NONE',  ( -96.91700721076711034, -272.8737681429720396, -221.5909131080033774 ) ) ;
#22992 = CARTESIAN_POINT ( 'NONE',  ( 154.8888658863856165, 204.4229923944245684, -215.0313167292097205 ) ) ;
#22993 = CARTESIAN_POINT ( 'NONE',  ( -59.11672987363058240, -278.3504499402774854, -197.1186823927174601 ) ) ;
#22994 = CARTESIAN_POINT ( 'NONE',  ( 27.25644497146580392, -295.8436636034106755, -310.4731855529720406 ) ) ;
#22995 = CARTESIAN_POINT ( 'NONE',  ( -72.66219300452470975, -292.0637266457310375, -206.3476288016925082 ) ) ;
#22996 = CARTESIAN_POINT ( 'NONE',  ( -114.1068513207666797, -273.5291142825242332, -267.5143728961976990 ) ) ;
#22997 = CARTESIAN_POINT ( 'NONE',  ( -76.14322411918233513, -288.2674159912355663, -332.7765424677062356 ) ) ;
#22998 = CARTESIAN_POINT ( 'NONE',  ( -67.50331407874537604, -274.3181487566125156, -199.6250604822606078 ) ) ;
#22999 = CARTESIAN_POINT ( 'NONE',  ( -102.5332902185967043, -297.1660282703861071, -237.3995630500442928 ) ) ;
#23000 = ORIENTED_EDGE ( 'NONE', *, *, #15663, .F. ) ;
#23001 = CARTESIAN_POINT ( 'NONE',  ( -68.10898923914206193, -281.5714837469734562, -201.3347671768908640 ) ) ;
#23002 = ADVANCED_FACE ( 'NONE', ( #9627 ), #30034, .T. ) ;
#23003 = CARTESIAN_POINT ( 'NONE',  ( -109.4385882997463000, -279.8062272867600768, -257.0846429150424797 ) ) ;
#23004 = CARTESIAN_POINT ( 'NONE',  ( -101.2326514894390357, -279.7642788576508792, -311.5900488088277598 ) ) ;
#23005 = CARTESIAN_POINT ( 'NONE',  ( -6.218724311040165986, -272.9485804728112157, -203.5624044412007549 ) ) ;
#23006 = CARTESIAN_POINT ( 'NONE',  ( 215.9306832106270804, -125.2391364535880882, 9.184850993605173582E-16 ) ) ;
#23007 = FACE_OUTER_BOUND ( 'NONE', #80080, .T. ) ;
#23008 = CARTESIAN_POINT ( 'NONE',  ( -83.43938179525416388, -279.5666383645781821, -213.6917700477247024 ) ) ;
#23009 = CARTESIAN_POINT ( 'NONE',  ( 31.71466012861212747, -276.7898872167788227, -304.1777121561370336 ) ) ;
#23010 = CARTESIAN_POINT ( 'NONE',  ( 35.68162627385076746, -277.3320258031395156, -253.1999424596317283 ) ) ;
#23011 = CARTESIAN_POINT ( 'NONE',  ( -113.1837301557192745, -277.0043172686608273, -280.0863615219236635 ) ) ;
#23012 = VERTEX_POINT ( 'NONE', #11502 ) ;
#23013 = CARTESIAN_POINT ( 'NONE',  ( 196.7383257810085695, 42.27872732282709478, 11.00000000000001066 ) ) ;
#23014 = CARTESIAN_POINT ( 'NONE',  ( 30.91350203915564521, -283.9512322764812211, -302.4158513194743705 ) ) ;
#23015 = CARTESIAN_POINT ( 'NONE',  ( -101.2597868920018698, -290.2362179963678841, -234.6610229866321049 ) ) ;
#23016 = ADVANCED_FACE ( 'NONE', ( #77785 ), #48403, .F. ) ;
#23017 = CARTESIAN_POINT ( 'NONE',  ( -43.64962250782689779, -285.3231538857705800, -193.6690169835193558 ) ) ;
#23018 = CARTESIAN_POINT ( 'NONE',  ( -74.32227712914057349, -281.7904756997564846, -334.5320164725492305 ) ) ;
#23019 = CARTESIAN_POINT ( 'NONE',  ( -5.796700387507616625, -281.2038489659973379, -336.8602238486927831 ) ) ;
#23020 = CARTESIAN_POINT ( 'NONE',  ( -6.617133361948789094, -281.6698648055175340, -203.6905802588781000 ) ) ;
#23021 = CARTESIAN_POINT ( 'NONE',  ( 202.9737692353694740, 295.9636489105243413, -68.65455606434399272 ) ) ;
#23022 = AXIS2_PLACEMENT_3D ( 'NONE', #25341, #2180, #16379 ) ;
#23023 = CARTESIAN_POINT ( 'NONE',  ( 13.13543902327948487, -280.7607650365613949, -327.5145976760659323 ) ) ;
#23024 = CARTESIAN_POINT ( 'NONE',  ( 32.59592577037092553, -295.9046202721189616, -297.4485528984286020 ) ) ;
#23025 = CIRCLE ( 'NONE', #79013, 4.025000000000000355 ) ;
#23026 = CARTESIAN_POINT ( 'NONE',  ( -59.98256321325585816, -287.7597293091604342, -198.6310622545221634 ) ) ;
#23027 = CARTESIAN_POINT ( 'NONE',  ( 115.2448031289451222, -299.5541904835127980, -191.8695490883551713 ) ) ;
#23028 = CARTESIAN_POINT ( 'NONE',  ( -95.48672851981423548, -293.1336711991844481, -222.0868933449800693 ) ) ;
#23029 = VECTOR ( 'NONE', #40726, 1000.000000000000000 ) ;
#23030 = CARTESIAN_POINT ( 'NONE',  ( -35.08222007661247943, -275.0236121215559706, -345.3270796028173777 ) ) ;
#23031 = CARTESIAN_POINT ( 'NONE',  ( -71.84314555784575873, -288.6937545219195727, -339.0183032178874214 ) ) ;
#23032 = CARTESIAN_POINT ( 'NONE',  ( 17.34455401813339748, -291.2489898442638037, -220.7295676744528521 ) ) ;
#23033 = CARTESIAN_POINT ( 'NONE',  ( -71.90079450396511618, -276.2038635667711901, -335.2360302347020138 ) ) ;
#23035 = ADVANCED_FACE ( 'NONE', ( #83449 ), #33274, .T. ) ;
#23034 = CARTESIAN_POINT ( 'NONE',  ( -92.75133650044125488, -295.3864797292696949, -220.9583075494125239 ) ) ;
#23036 = CARTESIAN_POINT ( 'NONE',  ( -71.38642831329084970, -290.8267312493016448, -335.5075075301652987 ) ) ;
#23037 = CARTESIAN_POINT ( 'NONE',  ( -112.3417001280820386, -272.5521521680024648, -270.3611179825637691 ) ) ;
#23038 = FACE_OUTER_BOUND ( 'NONE', #44851, .T. ) ;
#23039 = CARTESIAN_POINT ( 'NONE',  ( -39.11133947780892584, -293.5538666671052965, -346.6472643746234894 ) ) ;
#23040 = CARTESIAN_POINT ( 'NONE',  ( 11.65007981682876981, -288.3453612610721279, -215.0996671610036799 ) ) ;
#23041 = CARTESIAN_POINT ( 'NONE',  ( -108.5166941645621250, -289.1347622914310023, -243.6012486297789508 ) ) ;
#23042 = CARTESIAN_POINT ( 'NONE',  ( -68.99511371268030757, -290.9020949972578478, -336.7948167171654745 ) ) ;
#23043 = LINE ( 'NONE', #16414, #63840 ) ;
#23044 = CARTESIAN_POINT ( 'NONE',  ( -15.79435479331285208, -289.5691331498177874, -340.3305388770136801 ) ) ;
#23045 = CARTESIAN_POINT ( 'NONE',  ( -41.82201281398626946, -297.0880962903817135, -345.6342887277464229 ) ) ;
#23046 = FACE_OUTER_BOUND ( 'NONE', #44420, .T. ) ;
#23047 = CARTESIAN_POINT ( 'NONE',  ( -3.223725644451214123, -289.8167228735741787, -338.9611848770142046 ) ) ;
#23048 = CARTESIAN_POINT ( 'NONE',  ( -66.69793324462361284, -277.6895848197020200, -200.9592564668876662 ) ) ;
#23049 = CARTESIAN_POINT ( 'NONE',  ( -69.95728058527336657, -279.9675463629112642, -200.6189171856417772 ) ) ;
#23050 = CARTESIAN_POINT ( 'NONE',  ( -56.54727495883272326, -279.4780139250356683, -195.7615820074706221 ) ) ;
#23051 = CARTESIAN_POINT ( 'NONE',  ( -41.40653712575242196, -284.0008302512565592, -195.4585063752245162 ) ) ;
#23052 = CARTESIAN_POINT ( 'NONE',  ( 207.7836171167862460, 29.58337601776884540, 14.84040491829734165 ) ) ;
#23053 = CARTESIAN_POINT ( 'NONE',  ( -46.58719455689786315, -278.0732848876314733, -196.6519309690943658 ) ) ;
#23054 = CARTESIAN_POINT ( 'NONE',  ( -35.96220590900719571, -281.0347259771733661, -345.3612111458625691 ) ) ;
#23055 = CARTESIAN_POINT ( 'NONE',  ( 175.2296996224749250, 250.5000000000000568, -24.99999999999999289 ) ) ;
#23056 = CARTESIAN_POINT ( 'NONE',  ( -113.3514020704284491, -277.1241618676822895, -263.0608265157525238 ) ) ;
#23057 = CARTESIAN_POINT ( 'NONE',  ( -103.7445085002272549, -274.4029410594257570, -238.6429535384267808 ) ) ;
#23058 = CARTESIAN_POINT ( 'NONE',  ( -92.22217477566852040, -282.7347260208776447, -323.9300083195294064 ) ) ;
#23059 = CARTESIAN_POINT ( 'NONE',  ( -51.60292306502575599, -274.6680237183493887, -198.5511518752886957 ) ) ;
#23060 = CARTESIAN_POINT ( 'NONE',  ( -102.2283298552442119, -274.5093765130136489, -230.0085273007811963 ) ) ;
#23061 = CARTESIAN_POINT ( 'NONE',  ( 29.17177926537851462, -275.6248953327231561, -300.4948954698955959 ) ) ;
#23062 = CARTESIAN_POINT ( 'NONE',  ( -36.96048529847585939, -297.0475027606361778, -345.3729185345040946 ) ) ;
#23063 = CARTESIAN_POINT ( 'NONE',  ( -100.6793905824125375, -290.1405600426522824, -314.1485245330976568 ) ) ;
#23064 = CARTESIAN_POINT ( 'NONE',  ( -36.73901250372355776, -278.1395225728509217, -194.7907156090710430 ) ) ;
#23065 = CARTESIAN_POINT ( 'NONE',  ( -112.6395228627787617, -290.5875780896378728, -254.1980526174594672 ) ) ;
#23066 = CARTESIAN_POINT ( 'NONE',  ( -74.84666357450154806, -288.6234962447686598, -333.2788435033249357 ) ) ;
#23067 = CARTESIAN_POINT ( 'NONE',  ( 30.39101023973152138, -291.1267789752083672, -238.0334972168624006 ) ) ;
#23068 = ORIENTED_EDGE ( 'NONE', *, *, #14172, .T. ) ;
#23069 = CARTESIAN_POINT ( 'NONE',  ( 153.5035891336125360, 20.65792664182377791, 10.22121553831927088 ) ) ;
#23070 = CARTESIAN_POINT ( 'NONE',  ( -109.2405925237924720, -289.8886904403756262, -283.3433255781566800 ) ) ;
#23071 = CARTESIAN_POINT ( 'NONE',  ( -54.94434090351493438, -282.8906705383787994, 74.50000000000001421 ) ) ;
#23072 = CARTESIAN_POINT ( 'NONE',  ( 5.039754113410213066, -287.5508204977185756, -206.2928695170018614 ) ) ;
#23073 = CARTESIAN_POINT ( 'NONE',  ( -109.1418805571601069, -287.0519495502701943, -270.3937649182068412 ) ) ;
#23074 = CARTESIAN_POINT ( 'NONE',  ( -2.086246166839725191, -293.6556151164621724, -338.5510965693142680 ) ) ;
#23075 = CARTESIAN_POINT ( 'NONE',  ( 6.655189435110066221, -283.7832082778465974, -333.0164210029108176 ) ) ;
#23076 = CARTESIAN_POINT ( 'NONE',  ( -94.95574884498813617, -285.0173244828348516, -225.5120202439765649 ) ) ;
#23077 = CARTESIAN_POINT ( 'NONE',  ( -1.496641101183209033, -275.8531247943793687, -206.1877254301955418 ) ) ;
#23078 = CARTESIAN_POINT ( 'NONE',  ( -45.29039825565088506, -293.1733013604011830, -344.6331137995465497 ) ) ;
#23079 = CARTESIAN_POINT ( 'NONE',  ( -43.50022387494253451, -272.7676887600310351, -197.1718852836665690 ) ) ;
#23080 = ORIENTED_EDGE ( 'NONE', *, *, #43751, .F. ) ;
#23081 = LINE ( 'NONE', #51038, #72787 ) ;
#23082 = CARTESIAN_POINT ( 'NONE',  ( -33.44015491470214130, -294.6710496593075845, -347.2541546797676233 ) ) ;
#23083 = CARTESIAN_POINT ( 'NONE',  ( -55.12356286014078677, -287.7419957932046941, -198.0227959426889583 ) ) ;
#23084 = CARTESIAN_POINT ( 'NONE',  ( -91.42730863239619055, -298.3836642213286723, -215.9898069624495349 ) ) ;
#23085 = CARTESIAN_POINT ( 'NONE',  ( 33.48526286457929757, -287.9644541050095086, -252.2154794284144259 ) ) ;
#23086 = CARTESIAN_POINT ( 'NONE',  ( -101.9056079770701615, -277.0633211618754785, -311.9830931275199646 ) ) ;
#23087 = CARTESIAN_POINT ( 'NONE',  ( -22.22196106315864839, -292.8921925681279390, -194.9098735930651571 ) ) ;
#23088 = CARTESIAN_POINT ( 'NONE',  ( -15.74253984827584496, -284.4681217844403704, -197.6858003489593898 ) ) ;
#23089 = CARTESIAN_POINT ( 'NONE',  ( 37.06105332286537646, -293.6375546479075638, -250.5624990414058288 ) ) ;
#23091 = CARTESIAN_POINT ( 'NONE',  ( -74.99414792047076617, -291.8692812635048881, -207.7370721497273678 ) ) ;
#23090 = AXIS2_PLACEMENT_3D ( 'NONE', #52721, #17225, #66045 ) ;
#23092 = CARTESIAN_POINT ( 'NONE',  ( 196.0143093133015384, 73.40565171261611965, -12.00000000000000355 ) ) ;
#23093 = CARTESIAN_POINT ( 'NONE',  ( 185.1269714985386940, 260.3434729467832085, -151.0899229522644305 ) ) ;
#23094 = CARTESIAN_POINT ( 'NONE',  ( -32.37109183951687186, -287.6338450157566058, -194.2034656106150408 ) ) ;
#23095 = CARTESIAN_POINT ( 'NONE',  ( -37.37352853689063181, -280.5523547857346784, -350.3611179825600175 ) ) ;
#23096 = ORIENTED_EDGE ( 'NONE', *, *, #56608, .F. ) ;
#23098 = CARTESIAN_POINT ( 'NONE',  ( -40.26037179800940891, -282.0100258253328889, -343.6121072589616006 ) ) ;
#23097 = AXIS2_PLACEMENT_3D ( 'NONE', #90759, #4161, #4618 ) ;
#23099 = CARTESIAN_POINT ( 'NONE',  ( -114.3638145849992327, -278.2033256827040191, -271.6038180778849664 ) ) ;
#23100 = CARTESIAN_POINT ( 'NONE',  ( 5.963875701497209469, -282.6412053479145925, -209.3311620105461657 ) ) ;
#23101 = CARTESIAN_POINT ( 'NONE',  ( 204.8862265131387232, 293.2993722356919761, -68.49257677906207675 ) ) ;
#23102 = CARTESIAN_POINT ( 'NONE',  ( -87.35049715070886123, -283.9457885820980891, -212.5180243721792124 ) ) ;
#23104 = CARTESIAN_POINT ( 'NONE',  ( 36.37978931252406056, -285.7243027336915020, -282.1466241914561692 ) ) ;
#23103 = CIRCLE ( 'NONE', #57872, 0.5000000000000004441 ) ;
#23105 = CARTESIAN_POINT ( 'NONE',  ( -57.81105076995320502, -275.6511065199740074, -197.3592595797459808 ) ) ;
#23106 = CARTESIAN_POINT ( 'NONE',  ( -79.76887163852329365, -297.9532412756065582, -210.8806711187741598 ) ) ;
#23107 = CARTESIAN_POINT ( 'NONE',  ( -55.94420165895228791, -293.9814351171912108, -341.5137210183028742 ) ) ;
#23108 = CARTESIAN_POINT ( 'NONE',  ( -98.71704893602846198, -278.5855093591795821, -316.7117600353072930 ) ) ;
#23109 = CARTESIAN_POINT ( 'NONE',  ( 34.16456340563001959, -275.7459637883437154, -285.0530979528506350 ) ) ;
#23110 = CARTESIAN_POINT ( 'NONE',  ( -108.8832376279748928, -273.9848380210694359, -242.5869697181078664 ) ) ;
#23111 = CARTESIAN_POINT ( 'NONE',  ( -67.59935648285741649, -276.3602814150734162, -340.8307337207493788 ) ) ;
#23112 = CARTESIAN_POINT ( 'NONE',  ( -13.31626158348878874, -91.39965012456295312, -359.9159752949001927 ) ) ;
#23113 = CARTESIAN_POINT ( 'NONE',  ( -96.53395615140642860, -275.9201402729734696, -316.4389672228826953 ) ) ;
#23114 = CARTESIAN_POINT ( 'NONE',  ( -111.3930835316681396, -297.7392333357630605, -289.2553042699672687 ) ) ;
#23115 = EDGE_CURVE ( 'NONE', #83756, #5915, #4922, .T. ) ;
#23116 = CARTESIAN_POINT ( 'NONE',  ( 157.4970531492008661, 250.0000000000000568, 16.90571646082702983 ) ) ;
#23117 = CARTESIAN_POINT ( 'NONE',  ( 201.7648208617462728, 289.3015991269851384, -82.29596988341933184 ) ) ;
#23118 = CARTESIAN_POINT ( 'NONE',  ( -103.2847323722991462, -285.1986753534072250, -302.5048719639568162 ) ) ;
#23119 = CARTESIAN_POINT ( 'NONE',  ( -109.7134906865551613, -286.0167569733327468, -293.5620943931781994 ) ) ;
#23120 = CARTESIAN_POINT ( 'NONE',  ( 4.790877695016662940, -285.9863587247015744, -210.5602492379419743 ) ) ;
#23121 = CARTESIAN_POINT ( 'NONE',  ( -91.56938560940982086, -276.2402371828815717, -320.4934276960730699 ) ) ;
#23122 = CARTESIAN_POINT ( 'NONE',  ( -89.74980892215164374, -285.6611360427416457, -323.0094337614041251 ) ) ;
#23123 = CARTESIAN_POINT ( 'NONE',  ( -16.70922533298621104, -278.8034489925120170, -199.6150316263843649 ) ) ;
#23124 = CARTESIAN_POINT ( 'NONE',  ( -70.58071852552338044, -278.5809021355741493, -335.7017158562146619 ) ) ;
#23125 = CARTESIAN_POINT ( 'NONE',  ( 184.1778392089217107, 3.000000000000000444, -9.000000000000001776 ) ) ;
#23126 = CARTESIAN_POINT ( 'NONE',  ( 9.001565720888773825, -299.2987937108537722, -197.2538927750957782 ) ) ;
#23127 = CARTESIAN_POINT ( 'NONE',  ( 38.26851345264829973, -282.5273960088877061, -284.1183472288806797 ) ) ;
#23128 = VECTOR ( 'NONE', #89073, 1000.000000000000000 ) ;
#23129 = CARTESIAN_POINT ( 'NONE',  ( -33.05590202049050674, -283.4919033845052923, -347.1932429325181033 ) ) ;
#23130 = ORIENTED_EDGE ( 'NONE', *, *, #30936, .T. ) ;
#23131 = ORIENTED_EDGE ( 'NONE', *, *, #41338, .T. ) ;
#23132 = CARTESIAN_POINT ( 'NONE',  ( 175.2296996224750103, 250.0000000000000568, 0.000000000000000000 ) ) ;
#23133 = CARTESIAN_POINT ( 'NONE',  ( -7.846218032262715525, -288.2948082872201780, -200.5176880699377193 ) ) ;
#23134 = CARTESIAN_POINT ( 'NONE',  ( -82.57464792869529902, -288.3407322873807175, -332.0642678598034081 ) ) ;
#23135 = CARTESIAN_POINT ( 'NONE',  ( -109.8950036751649861, -295.8782574299456769, -260.5650054114635168 ) ) ;
#23136 = EDGE_CURVE ( 'NONE', #62353, #19834, #53298, .T. ) ;
#23137 = CARTESIAN_POINT ( 'NONE',  ( 23.03320857062457350, -292.2627004819572676, -222.7146264494023171 ) ) ;
#23138 = CARTESIAN_POINT ( 'NONE',  ( 22.51363516826799227, -286.6273581318101265, -313.3500303904747852 ) ) ;
#23140 = CARTESIAN_POINT ( 'NONE',  ( -30.69394174215420534, -290.3771977414566550, -196.6469312759338663 ) ) ;
#23139 = CARTESIAN_POINT ( 'NONE',  ( -10.52616955324940484, -287.2701896116669218, -338.9453373976196531 ) ) ;
#23141 = CARTESIAN_POINT ( 'NONE',  ( -70.17374683063228247, -286.8146969797601855, -204.7026970882218677 ) ) ;
#23142 = CARTESIAN_POINT ( 'NONE',  ( -104.5643897065728680, -276.1118192978071875, -303.7362850233948848 ) ) ;
#23143 = CARTESIAN_POINT ( 'NONE',  ( 21.77149474858413569, -286.6041409881937625, -318.4656412901785529 ) ) ;
#23144 = CARTESIAN_POINT ( 'NONE',  ( 36.98962690132006514, -289.4240087407114288, -260.3683971037505671 ) ) ;
#23145 = CARTESIAN_POINT ( 'NONE',  ( -79.53313586798829249, -287.6200394206268811, -332.6326208329983274 ) ) ;
#23146 = CARTESIAN_POINT ( 'NONE',  ( -78.49899755629139975, -284.5627539808037341, -330.9373948245737438 ) ) ;
#23147 = CARTESIAN_POINT ( 'NONE',  ( -96.04806698317332803, -293.1963925878686723, -223.4186966317512031 ) ) ;
#23148 = CARTESIAN_POINT ( 'NONE',  ( 209.1374487190023501, 30.94653725228601360, 15.00000000000000000 ) ) ;
#23149 = DIRECTION ( 'NONE',  ( 1.000000000000000000, 0.000000000000000000, 0.000000000000000000 ) ) ;
#23150 = CARTESIAN_POINT ( 'NONE',  ( -82.13692737016141621, -299.3671430803469207, -209.4462635934506238 ) ) ;
#23151 = CARTESIAN_POINT ( 'NONE',  ( 31.22521321643745651, -280.4079841052864595, -244.6974888225194320 ) ) ;
#23152 = CARTESIAN_POINT ( 'NONE',  ( 22.95158276074157655, -278.9430459095565880, -225.7332082813008753 ) ) ;
#23153 = CARTESIAN_POINT ( 'NONE',  ( 37.90586491131076485, -292.5535674558253731, -254.7414366649772717 ) ) ;
#23154 = CARTESIAN_POINT ( 'NONE',  ( -91.85391228343023329, -271.5009101324063181, -220.2784769973490597 ) ) ;
#23155 = CARTESIAN_POINT ( 'NONE',  ( 20.28104307434243481, -274.2866120228680415, -317.5079784737774844 ) ) ;
#23156 = CARTESIAN_POINT ( 'NONE',  ( -106.4451965586153932, -297.5345032664055793, -295.5296603855035187 ) ) ;
#23157 = DIRECTION ( 'NONE',  ( 1.000000000000000000, 0.000000000000000000, 0.000000000000000000 ) ) ;
#23158 = CARTESIAN_POINT ( 'NONE',  ( -63.33942902849123868, -272.2946685124165356, -198.5090172173570409 ) ) ;
#23159 = CARTESIAN_POINT ( 'NONE',  ( -112.2094488735885420, -294.6235898437623177, -283.6510303108961466 ) ) ;
#23160 = VECTOR ( 'NONE', #56730, 1000.000000000000000 ) ;
#23161 = CARTESIAN_POINT ( 'NONE',  ( 34.02188085833573439, -295.2125768825517298, -288.3225830535881187 ) ) ;
#23162 = CARTESIAN_POINT ( 'NONE',  ( 142.6449502718966755, -27.00396092263537540, 22.50000000000000000 ) ) ;
#23163 = CARTESIAN_POINT ( 'NONE',  ( -78.03107744932488288, -296.4170835911325526, -331.2250690876712724 ) ) ;
#23164 = PLANE ( 'NONE',  #39921 ) ;
#23165 = AXIS2_PLACEMENT_3D ( 'NONE', #59866, #2088, #29587 ) ;
#23167 = CARTESIAN_POINT ( 'NONE',  ( -79.72804649810302635, -297.4609733392965722, -210.9271408196563868 ) ) ;
#23166 = CARTESIAN_POINT ( 'NONE',  ( -67.81205731565275130, -283.6743745887989121, -201.4270676777732376 ) ) ;
#23168 = VECTOR ( 'NONE', #61126, 1000.000000000000114 ) ;
#23169 = CARTESIAN_POINT ( 'NONE',  ( -74.27598446526295106, -283.5288494502705703, -337.9843474849482163 ) ) ;
#23170 = CARTESIAN_POINT ( 'NONE',  ( 38.18129690616638072, -283.5024435202262225, -272.7256716900491824 ) ) ;
#23171 = CARTESIAN_POINT ( 'NONE',  ( -80.92273809564112241, -285.1451956848103464, -206.8425642336146097 ) ) ;
#23172 = CARTESIAN_POINT ( 'NONE',  ( -1.540488127866042944, -290.5276815231948717, -204.6327781894834459 ) ) ;
#23173 = CARTESIAN_POINT ( 'NONE',  ( 10.59707575819633618, -273.9094976428775681, -330.5268031993606428 ) ) ;
#23174 = VECTOR ( 'NONE', #64807, 1000.000000000000000 ) ;
#23175 = CARTESIAN_POINT ( 'NONE',  ( -48.18343439339476930, -260.1500860263135451, -498.8200089662520327 ) ) ;
#23176 = CARTESIAN_POINT ( 'NONE',  ( 13.49267389295802744, -285.4664077818697479, -217.2144373099860104 ) ) ;
#23177 = CARTESIAN_POINT ( 'NONE',  ( -112.8652126534752540, -289.6398681779726871, -257.0310179803962569 ) ) ;
#23178 = DIRECTION ( 'NONE',  ( 0.000000000000000000, 1.000000000000000000, -0.000000000000000000 ) ) ;
#23179 = CARTESIAN_POINT ( 'NONE',  ( -99.12839207723251889, -298.7066111322874917, -229.9096502077262016 ) ) ;
#23180 = CARTESIAN_POINT ( 'NONE',  ( -90.66011675739846964, -280.7398643825711133, -215.5538671777336219 ) ) ;
#23182 = CARTESIAN_POINT ( 'NONE',  ( 30.04263589383815258, -280.8416039714027761, -242.2285968445845299 ) ) ;
#23181 = CARTESIAN_POINT ( 'NONE',  ( 22.70276846251368497, -292.1921377247896316, -315.8920810494681746 ) ) ;
#23183 = CARTESIAN_POINT ( 'NONE',  ( -72.07213583812325908, -295.6654071016297962, -339.0837259068874801 ) ) ;
#23184 = VECTOR ( 'NONE', #47355, 1000.000000000000000 ) ;
#23185 = CARTESIAN_POINT ( 'NONE',  ( -32.37616501558099458, -284.1941243810745732, -194.9515292680658547 ) ) ;
#23186 = CARTESIAN_POINT ( 'NONE',  ( -87.61032342335124667, -281.3504217482249032, -214.7008434753115864 ) ) ;
#23187 = CARTESIAN_POINT ( 'NONE',  ( -68.62871233428695916, -294.5324232815688106, -336.5906878928592505 ) ) ;
#23188 = CARTESIAN_POINT ( 'NONE',  ( -37.23030460611856540, -296.0533920991546779, -195.3604033763125187 ) ) ;
#23189 = EDGE_LOOP ( 'NONE', ( #49311, #35729, #36887, #56042, #64760, #52363, #3857 ) ) ;
#23190 = LINE ( 'NONE', #52072, #27235 ) ;
#23191 = VECTOR ( 'NONE', #25027, 1000.000000000000000 ) ;
#23192 = CARTESIAN_POINT ( 'NONE',  ( 32.91099910132031425, -283.8623807971577548, -295.7411597350413786 ) ) ;
#23193 = CARTESIAN_POINT ( 'NONE',  ( -95.65723462145159317, -295.4417982783928096, -314.3963507363878307 ) ) ;
#23194 = CARTESIAN_POINT ( 'NONE',  ( -83.63170945779074827, -296.0521521680024080, -525.1711561948568487 ) ) ;
#23195 = CARTESIAN_POINT ( 'NONE',  ( -4.829096099716524648, -280.1237833571632336, -337.9475929042657754 ) ) ;
#23196 = CARTESIAN_POINT ( 'NONE',  ( -73.85908977557677701, -272.7773911846299484, -202.6954716124624269 ) ) ;
#23197 = CARTESIAN_POINT ( 'NONE',  ( -92.41312301962470599, -289.7015755172369040, -318.3546998379551383 ) ) ;
#23198 = CARTESIAN_POINT ( 'NONE',  ( -62.56427261639770165, -281.2381611747639454, -201.0647058391529072 ) ) ;
#23199 = CARTESIAN_POINT ( 'NONE',  ( -67.40181763168531859, -275.2513320519411195, -202.9467554711895616 ) ) ;
#23200 = VECTOR ( 'NONE', #6684, 1000.000000000000000 ) ;
#23201 = CARTESIAN_POINT ( 'NONE',  ( 21.01066939769183506, -283.8189942461900159, -319.3656217377672419 ) ) ;
#23202 = CARTESIAN_POINT ( 'NONE',  ( -11.58953084956374369, -279.1899416906577471, -201.5763216191979836 ) ) ;
#23203 = CARTESIAN_POINT ( 'NONE',  ( 10.97131902505812562, -278.3837087079525645, -327.7270732700507665 ) ) ;
#23204 = ORIENTED_EDGE ( 'NONE', *, *, #89909, .T. ) ;
#23205 = CARTESIAN_POINT ( 'NONE',  ( -68.84212266237791766, -273.4826822037952638, -200.0849027925046926 ) ) ;
#23206 = CARTESIAN_POINT ( 'NONE',  ( -17.06335767002813952, -294.2360154427400403, -198.6827564499790526 ) ) ;
#23207 = LINE ( 'NONE', #37863, #20381 ) ;
#23208 = EDGE_CURVE ( 'NONE', #6260, #7585, #59410, .T. ) ;
#23209 = CARTESIAN_POINT ( 'NONE',  ( 197.1856756230095868, 68.15307035998191054, 10.54037349550492664 ) ) ;
#23210 = CARTESIAN_POINT ( 'NONE',  ( -63.85646719829682638, -293.5338488162076374, -341.3348638840794251 ) ) ;
#23211 = CARTESIAN_POINT ( 'NONE',  ( -66.82398576107701160, -297.3216081865396632, -203.5426269840474731 ) ) ;
#23212 = CARTESIAN_POINT ( 'NONE',  ( 222.8344101925596306, 35.72494958537217968, -7.000000000000000888 ) ) ;
#23213 = CARTESIAN_POINT ( 'NONE',  ( -66.76613668881105923, -293.1936707411405223, -199.9557894442065447 ) ) ;
#23214 = CARTESIAN_POINT ( 'NONE',  ( -95.95921662488163406, -280.4090924074130839, -317.1477375740089997 ) ) ;
#23215 = CARTESIAN_POINT ( 'NONE',  ( 37.48866874839452379, -289.5608954803890356, -271.0276891956934264 ) ) ;
#23216 = CARTESIAN_POINT ( 'NONE',  ( 1.809409478635427559, -274.5274096658723124, -334.1967465040609682 ) ) ;
#23217 = CARTESIAN_POINT ( 'NONE',  ( 31.62113498613430096, -277.8420504543230436, -298.5241164368026716 ) ) ;
#23218 = CARTESIAN_POINT ( 'NONE',  ( 9.108005016690839284, -292.4890540038915674, -328.5972628349492197 ) ) ;
#23219 = CARTESIAN_POINT ( 'NONE',  ( -110.8926297111280519, -280.6443336381020686, -252.1263398958670905 ) ) ;
#23220 = ORIENTED_EDGE ( 'NONE', *, *, #44799, .T. ) ;
#23221 = CARTESIAN_POINT ( 'NONE',  ( -82.81120301710156184, -283.3602070823393433, -327.5627857347354279 ) ) ;
#23222 = CARTESIAN_POINT ( 'NONE',  ( -101.6395985165605680, -280.1840719848489698, -228.4646074202884733 ) ) ;
#23223 = VECTOR ( 'NONE', #22565, 1000.000000000000114 ) ;
#23224 = CARTESIAN_POINT ( 'NONE',  ( -70.31319262419275162, -282.2719379550259191, -339.5194819836434021 ) ) ;
#23225 = CARTESIAN_POINT ( 'NONE',  ( -86.93402125105039602, -278.6638060523109175, -329.0260674517909365 ) ) ;
#23226 = CARTESIAN_POINT ( 'NONE',  ( 5.498173904724613870, -278.0035894714825986, -333.5074000915728334 ) ) ;
#23227 = CARTESIAN_POINT ( 'NONE',  ( -67.68488546085839630, -291.9805209788416391, -333.4427485647536855 ) ) ;
#23228 = EDGE_LOOP ( 'NONE', ( #90608, #34429, #49692, #89140, #61656, #12006 ) ) ;
#23229 = CARTESIAN_POINT ( 'NONE',  ( -110.1217768095011991, -298.7855627655889634, -252.1960095164200197 ) ) ;
#23230 = AXIS2_PLACEMENT_3D ( 'NONE', #88800, #59017, #43856 ) ;
#23231 = CARTESIAN_POINT ( 'NONE',  ( -60.36905172503362849, -292.8262349178734212, -200.7092348225381215 ) ) ;
#23232 = CARTESIAN_POINT ( 'NONE',  ( -71.22137473659145712, -275.5218334964210953, -336.8743832344716793 ) ) ;
#23233 = CARTESIAN_POINT ( 'NONE',  ( -6.023395597853273387, -290.4062899862208837, -339.5936090380857308 ) ) ;
#23234 = CARTESIAN_POINT ( 'NONE',  ( -89.88382808080551456, -290.6341816295014269, -219.5357556290681487 ) ) ;
#23235 = CARTESIAN_POINT ( 'NONE',  ( 39.29397142541546373, -286.9672888522335370, -262.9694154054036517 ) ) ;
#23236 = DIRECTION ( 'NONE',  ( -1.000000000000000000, 0.000000000000000000, 0.000000000000000000 ) ) ;
#23237 = CARTESIAN_POINT ( 'NONE',  ( -51.18775407657944498, -281.6318124543672070, -342.9027590173910767 ) ) ;
#23238 = CARTESIAN_POINT ( 'NONE',  ( -71.72415620242954049, -291.3718850251189565, -336.1684269271525523 ) ) ;
#23239 = CARTESIAN_POINT ( 'NONE',  ( -110.6824360606842959, -283.1326777471875857, -262.6585213728271242 ) ) ;
#23240 = CARTESIAN_POINT ( 'NONE',  ( -22.10843189992635871, -281.5664342479233824, -198.4118262717569223 ) ) ;
#23241 = VERTEX_POINT ( 'NONE', #20004 ) ;
#23242 = CARTESIAN_POINT ( 'NONE',  ( -104.9430788388014975, -291.0216986242278949, -306.7324502201704490 ) ) ;
#23243 = TOROIDAL_SURFACE ( 'NONE', #68604, 5.654241149514406040, 1.000000000000000000 ) ;
#23244 = CARTESIAN_POINT ( 'NONE',  ( -108.8236835104323319, -278.8453416376117389, -285.4711971875941572 ) ) ;
#23245 = CARTESIAN_POINT ( 'NONE',  ( 30.55413562263701266, -291.8857969571606645, -234.7762722596812353 ) ) ;
#23246 = CARTESIAN_POINT ( 'NONE',  ( 25.40731789069867474, -287.7666116624911865, -225.9907249690027413 ) ) ;
#23247 = CARTESIAN_POINT ( 'NONE',  ( -12.23787821491825412, -289.2265948227954482, -343.1446926993477859 ) ) ;
#23248 = CARTESIAN_POINT ( 'NONE',  ( -46.72697293178587330, -286.0965006771618846, -197.9161668777973944 ) ) ;
#23249 = ORIENTED_EDGE ( 'NONE', *, *, #79144, .T. ) ;
#23250 = DIRECTION ( 'NONE',  ( 0.000000000000000000, 0.000000000000000000, -1.000000000000000000 ) ) ;
#23251 = CARTESIAN_POINT ( 'NONE',  ( -11.59563683910588416, -294.2441977125491235, -199.0497891597565570 ) ) ;
#23252 = AXIS2_PLACEMENT_3D ( 'NONE', #77796, #91506, #77318 ) ;
#23253 = CARTESIAN_POINT ( 'NONE',  ( -107.9265843327669216, -294.8576346342608758, -300.0122397331491015 ) ) ;
#23254 = CONICAL_SURFACE ( 'NONE', #15693, 2.241321557046427326, 0.09862129276975473147 ) ;
#23255 = CARTESIAN_POINT ( 'NONE',  ( -48.65598010146408825, -276.2583610780988579, -342.7687068352769870 ) ) ;
#23256 = CARTESIAN_POINT ( 'NONE',  ( -109.7520853079921608, -296.2279283463375918, -244.4758151155552071 ) ) ;
#23257 = CARTESIAN_POINT ( 'NONE',  ( 34.32654477548992134, -291.8071658631701553, -253.1499209683281606 ) ) ;
#23258 = CARTESIAN_POINT ( 'NONE',  ( -104.8702353662897906, -294.3880289069327887, -300.7828693776153273 ) ) ;
#23259 = CARTESIAN_POINT ( 'NONE',  ( -65.49337432703740092, -292.8807851693272823, -202.5639486850024298 ) ) ;
#23260 = CARTESIAN_POINT ( 'NONE',  ( 16.39504089865694425, -295.3454948886044349, -320.2268250129523608 ) ) ;
#23261 = CARTESIAN_POINT ( 'NONE',  ( 145.2857639756989272, -299.5541904835127980, -201.0153591320744226 ) ) ;
#23262 = CARTESIAN_POINT ( 'NONE',  ( -55.64901225581454725, -293.2871030229669032, -343.2642780386795494 ) ) ;
#23263 = CARTESIAN_POINT ( 'NONE',  ( -94.36988634794697361, -299.2270841038119329, -221.6305095276072450 ) ) ;
#23264 = CARTESIAN_POINT ( 'NONE',  ( -101.8447249312820446, -291.0207030784135327, -305.1495542590761829 ) ) ;
#23265 = CARTESIAN_POINT ( 'NONE',  ( -20.83927121544913774, -295.1678696842265595, -341.5452097418858557 ) ) ;
#23266 = CARTESIAN_POINT ( 'NONE',  ( -73.28952984851748909, -279.5062559411719576, -336.6038905178002096 ) ) ;
#23267 = CARTESIAN_POINT ( 'NONE',  ( -38.14780144950937313, -278.7270804416718875, -193.8585136119885703 ) ) ;
#23268 = VECTOR ( 'NONE', #60019, 1000.000000000000114 ) ;
#23269 = EDGE_CURVE ( 'NONE', #29794, #43403, #91127, .T. ) ;
#23270 = CARTESIAN_POINT ( 'NONE',  ( -36.93193448223406961, -273.4057789934512357, -193.4511072721188043 ) ) ;
#23271 = CARTESIAN_POINT ( 'NONE',  ( 34.50981191351140609, -279.3793453141463488, -250.8527308020481712 ) ) ;
#23272 = CARTESIAN_POINT ( 'NONE',  ( -111.9302186717079763, -277.1498190171853935, -254.7100334137157915 ) ) ;
#23273 = CARTESIAN_POINT ( 'NONE',  ( -109.5683945903965224, -276.8193602342198574, -249.5444651516260990 ) ) ;
#23274 = EDGE_CURVE ( 'NONE', #79714, #82047, #55999, .T. ) ;
#23275 = CARTESIAN_POINT ( 'NONE',  ( -37.13149631189084943, -296.7396699976850982, -196.8651434942196090 ) ) ;
#23276 = DIRECTION ( 'NONE',  ( -1.387778780781440785E-14, 0.000000000000000000, 1.000000000000000000 ) ) ;
#23277 = CARTESIAN_POINT ( 'NONE',  ( -109.2207238160707163, -288.2797955091778022, -293.1550527246924958 ) ) ;
#23278 = CARTESIAN_POINT ( 'NONE',  ( -85.16467598022127561, -289.6915113693370927, -330.7778249780870397 ) ) ;
#23279 = AXIS2_PLACEMENT_3D ( 'NONE', #85409, #35215, #40879 ) ;
#23280 = CARTESIAN_POINT ( 'NONE',  ( -65.56310310867200997, -275.6841838584450670, -200.6796372794978254 ) ) ;
#23281 = CARTESIAN_POINT ( 'NONE',  ( -80.77184926015803512, -295.4611348635506829, -209.4197480422085391 ) ) ;
#23282 = CARTESIAN_POINT ( 'NONE',  ( -34.49521044067520137, -282.2143964689399809, -347.1468999825981427 ) ) ;
#23283 = B_SPLINE_CURVE_WITH_KNOTS ( 'NONE', 3,
 ( #60500, #82717, #68999, #4130, #85529, #91687, #62853, #78442, #5544, #56682 ),
 .UNSPECIFIED., .F., .F.,
 ( 4, 2, 2, 2, 4 ),
 ( -1.807859651496474836E-05, 0.002330337966246291345, 0.004678754529007548082, 0.007027171091768803952, 0.009375587654530059822 ),
 .UNSPECIFIED. ) ;
#23284 = DIRECTION ( 'NONE',  ( 0.000000000000000000, 1.000000000000000000, 0.000000000000000000 ) ) ;
#23285 = CARTESIAN_POINT ( 'NONE',  ( 37.56699174476693059, -279.4925984755161608, -265.7357445968982006 ) ) ;
#23286 = CARTESIAN_POINT ( 'NONE',  ( 198.4595007507759021, 25.14564487145584692, 10.76846978260893195 ) ) ;
#23287 = CARTESIAN_POINT ( 'NONE',  ( 11.20487646469172915, -291.5370370169802072, -215.2445762560115554 ) ) ;
#23288 = CARTESIAN_POINT ( 'NONE',  ( -110.1356125781775575, -282.8805732588281217, -255.8039275575864622 ) ) ;
#23289 = CARTESIAN_POINT ( 'NONE',  ( 200.4283040947223640, 40.93816728012065909, 10.50000000000114753 ) ) ;
#23290 = CARTESIAN_POINT ( 'NONE',  ( 157.4851178187871312, 1.000000000000001332, 7.000000000000000000 ) ) ;
#23291 = CARTESIAN_POINT ( 'NONE',  ( 25.01795185599723581, -290.9887891369123736, -228.6924912560687062 ) ) ;
#23292 = CARTESIAN_POINT ( 'NONE',  ( -62.03855187148693773, -278.9786648920089078, -339.9604337565301080 ) ) ;
#23293 = CARTESIAN_POINT ( 'NONE',  ( 15.49083027676914526, -283.5298621676657262, -325.8294192801051850 ) ) ;
#23295 = CARTESIAN_POINT ( 'NONE',  ( -83.64786928081187511, -285.3964072233478646, -213.8619499687001735 ) ) ;
#23294 = CARTESIAN_POINT ( 'NONE',  ( -91.12656288406512317, -271.3749277186235531, -217.2903846593624166 ) ) ;
#23296 = CARTESIAN_POINT ( 'NONE',  ( 14.15653979063705314, -277.7371666531194023, -322.9992634733325758 ) ) ;
#23297 = CARTESIAN_POINT ( 'NONE',  ( -48.62267331036382245, -278.0021648618229619, -342.6991424076827002 ) ) ;
#23298 = CARTESIAN_POINT ( 'NONE',  ( -89.04056962133726927, -285.7786127781236019, -324.7667082790004542 ) ) ;
#23299 = VERTEX_POINT ( 'NONE', #26171 ) ;
#23300 = AXIS2_PLACEMENT_3D ( 'NONE', #22915, #45600, #65581 ) ;
#23301 = CARTESIAN_POINT ( 'NONE',  ( 200.1145890159574208, 64.93834475843401322, 5.212391550061751921 ) ) ;
#23302 = CARTESIAN_POINT ( 'NONE',  ( -111.2159886395630650, -296.1125483779802607, -292.1237406227365909 ) ) ;
#23303 = CARTESIAN_POINT ( 'NONE',  ( 27.79052400944419787, -289.0429914653246897, -233.7911935675299446 ) ) ;
#23304 = DIRECTION ( 'NONE',  ( 1.000000000000000000, 0.000000000000000000, 0.000000000000000000 ) ) ;
#23305 = CARTESIAN_POINT ( 'NONE',  ( -115.3430155898818299, -287.8380690714489560, -288.1317622949166548 ) ) ;
#23306 = CARTESIAN_POINT ( 'NONE',  ( -97.44603533916775007, -278.1124905655667021, -222.7275016991840744 ) ) ;
#23307 = CARTESIAN_POINT ( 'NONE',  ( -27.92750716894570218, -290.5695084754560185, -194.6917755602924274 ) ) ;
#23308 =( REPRESENTATION_RELATIONSHIP ('NONE','NONE', #78428, #71246 ) REPRESENTATION_RELATIONSHIP_WITH_TRANSFORMATION ( #48256 )SHAPE_REPRESENTATION_RELATIONSHIP( ) );
#23309 = AXIS2_PLACEMENT_3D ( 'NONE', #81845, #73377, #88009 ) ;
#23310 = CARTESIAN_POINT ( 'NONE',  ( -105.8514168628970111, -285.7108616742070808, -297.6500058103541733 ) ) ;
#23311 = CARTESIAN_POINT ( 'NONE',  ( -90.21293732324741654, -281.0523667242918009, -218.4945783500481582 ) ) ;
#23312 = CARTESIAN_POINT ( 'NONE',  ( 30.88744572837336122, -288.5313313166724356, -235.9606827091901948 ) ) ;
#23313 = CARTESIAN_POINT ( 'NONE',  ( 20.92141384490246736, -284.2028694481392677, -317.6085879122549045 ) ) ;
#23314 = CARTESIAN_POINT ( 'NONE',  ( 19.87862433691756792, -276.4184067058993151, -321.9059365171859213 ) ) ;
#23315 = CARTESIAN_POINT ( 'NONE',  ( 54.21872727873468278, -297.2238285168403422, -195.7474017060856113 ) ) ;
#23316 = CARTESIAN_POINT ( 'NONE',  ( -48.11668167676107544, -279.7521365748772837, -194.0648984730356688 ) ) ;
#23317 = AXIS2_PLACEMENT_3D ( 'NONE', #76162, #11295, #11754 ) ;
#23318 = CARTESIAN_POINT ( 'NONE',  ( -60.99620677641041766, -299.6630280932378696, -199.7248724386597587 ) ) ;
#23319 = CIRCLE ( 'NONE', #53597, 1.000000000000000888 ) ;
#23320 = CARTESIAN_POINT ( 'NONE',  ( 185.8821869067168393, 215.0000000000000568, 23.16839473634431101 ) ) ;
#23321 = CARTESIAN_POINT ( 'NONE',  ( -18.20453976106250948, -63.49190233628851132, -21.50000000000000000 ) ) ;
#23322 = CARTESIAN_POINT ( 'NONE',  ( -55.07509983363680561, -272.0669901721399242, -196.4726848811926629 ) ) ;
#23323 = CARTESIAN_POINT ( 'NONE',  ( 129.9467878515196162, -299.5541904835127980, -195.3611179825600175 ) ) ;
#23324 = CARTESIAN_POINT ( 'NONE',  ( -16.89849494288845833, -279.8310582924833625, -200.2179515067299462 ) ) ;
#23325 = AXIS2_PLACEMENT_3D ( 'NONE', #5807, #28063, #56953 ) ;
#23326 = CARTESIAN_POINT ( 'NONE',  ( -63.43632891748307401, -274.9245924192893540, -198.3397387500548064 ) ) ;
#23327 = CARTESIAN_POINT ( 'NONE',  ( 37.10600378377182551, -280.3759911695543678, -251.6432229072009363 ) ) ;
#23328 = CARTESIAN_POINT ( 'NONE',  ( -74.02803292616864894, -291.3067595809320096, -334.6570387889773883 ) ) ;
#23329 = CARTESIAN_POINT ( 'NONE',  ( -59.96120240422219183, -299.2844946955736418, -197.4290307838639364 ) ) ;
#23330 = ADVANCED_FACE ( 'NONE', ( #46994 ), #26649, .F. ) ;
#23331 = CARTESIAN_POINT ( 'NONE',  ( -87.21543557016718751, -298.5804568805023678, -212.1480869423973843 ) ) ;
#23332 = CARTESIAN_POINT ( 'NONE',  ( -32.05250701161843807, -294.1191701809748906, -195.7019962100786188 ) ) ;
#23333 = CARTESIAN_POINT ( 'NONE',  ( 29.42842234223097364, -279.1031206889799705, -236.4559201851825776 ) ) ;
#23334 = CARTESIAN_POINT ( 'NONE',  ( 35.46864646699807366, -283.2711528789251361, -254.8095909193533544 ) ) ;
#23335 = CARTESIAN_POINT ( 'NONE',  ( -84.20405779875382279, -271.4240705508181009, -212.2597734791546031 ) ) ;
#23336 = CARTESIAN_POINT ( 'NONE',  ( -113.1062432911641338, -286.0494738921869384, -278.4958837259513871 ) ) ;
#23337 = VECTOR ( 'NONE', #9557, 1000.000000000000000 ) ;
#23338 = CARTESIAN_POINT ( 'NONE',  ( 8.161102698606372385, -287.3330513106757849, -327.8391225368562232 ) ) ;
#23339 = CARTESIAN_POINT ( 'NONE',  ( -112.2160709410385238, -274.3727637374173582, -284.1527603578829257 ) ) ;
#23340 = ORIENTED_EDGE ( 'NONE', *, *, #10248, .T. ) ;
#23341 = CARTESIAN_POINT ( 'NONE',  ( -12.43309089404968582, -287.3092843456158221, -342.6534409828449270 ) ) ;
#23342 = CARTESIAN_POINT ( 'NONE',  ( -82.56268449359332351, -289.3565593180966857, -327.6947909827397325 ) ) ;
#23343 = ORIENTED_EDGE ( 'NONE', *, *, #51125, .F. ) ;
#23344 = CARTESIAN_POINT ( 'NONE',  ( -32.34036460503271115, -287.1934655579176479, -193.8203679819181104 ) ) ;
#23345 = CARTESIAN_POINT ( 'NONE',  ( 20.69575246798601853, -275.2621750811438233, -226.0264138379587848 ) ) ;
#23346 = CARTESIAN_POINT ( 'NONE',  ( 37.46286475800634719, -292.2595500284507466, -253.3974698893223660 ) ) ;
#23347 = CARTESIAN_POINT ( 'NONE',  ( 37.23037318310591814, -281.9683987575965034, -251.5909643053241211 ) ) ;
#23348 = CARTESIAN_POINT ( 'NONE',  ( 36.31067086039960401, -282.8195813053796428, -250.3607749432480887 ) ) ;
#23349 = CARTESIAN_POINT ( 'NONE',  ( -86.08570385405211312, -284.0403258403158020, -329.9410339962473131 ) ) ;
#23350 = EDGE_CURVE ( 'NONE', #36174, #7661, #70224, .T. ) ;
#23351 = CARTESIAN_POINT ( 'NONE',  ( -16.91986785000901250, -280.6565537443357812, -200.2537984424178603 ) ) ;
#23352 = CARTESIAN_POINT ( 'NONE',  ( -92.05005921254146983, -294.6952119285919025, -226.6919474004047572 ) ) ;
#23353 = CARTESIAN_POINT ( 'NONE',  ( 198.0283610688475733, 285.1170005366674900, -111.8712284615754413 ) ) ;
#23354 = VERTEX_POINT ( 'NONE', #41773 ) ;
#23355 = CARTESIAN_POINT ( 'NONE',  ( -94.10095716986310777, -279.8749314876756671, -319.1301160161154939 ) ) ;
#23356 = CARTESIAN_POINT ( 'NONE',  ( -57.10806838110030981, -168.8649533382279060, -363.8072750875188035 ) ) ;
#23357 = CARTESIAN_POINT ( 'NONE',  ( -86.16221177476658966, -296.7019530828766278, -215.9510976696027171 ) ) ;
#23358 = CARTESIAN_POINT ( 'NONE',  ( 23.93002802275086438, -292.4389926912623423, -223.8066277808137272 ) ) ;
#23359 = CARTESIAN_POINT ( 'NONE',  ( -29.93913374795647542, -125.2961201611392568, -360.6981843052933527 ) ) ;
#23361 = CARTESIAN_POINT ( 'NONE',  ( -99.52671033333007244, -288.4082832812932224, -310.1036005480806921 ) ) ;
#23360 = CARTESIAN_POINT ( 'NONE',  ( -26.29730116933454553, -296.7626041866188302, -193.9529577754875902 ) ) ;
#23362 = CARTESIAN_POINT ( 'NONE',  ( -7.469891723505769576, -296.5167088783151712, -338.3347726063263963 ) ) ;
#23363 = CARTESIAN_POINT ( 'NONE',  ( -52.20492163588632906, -287.1730334191447014, -198.3866216452606182 ) ) ;
#23364 = VERTEX_POINT ( 'NONE', #3940 ) ;
#23365 = CARTESIAN_POINT ( 'NONE',  ( -4.592002640016518811, -295.5724248616011778, -339.8037634367398141 ) ) ;
#23366 = CARTESIAN_POINT ( 'NONE',  ( -94.17386315521936524, -285.6934710643051858, -224.4273059376094750 ) ) ;
#23367 = CARTESIAN_POINT ( 'NONE',  ( -36.17639422181220255, -296.8613671933729847, -193.7584200153915788 ) ) ;
#23368 = CARTESIAN_POINT ( 'NONE',  ( 8.745887779062593737, -293.4684845264431488, -208.8122564151247502 ) ) ;
#23369 = CARTESIAN_POINT ( 'NONE',  ( 36.31260720565570210, -294.3258991373899107, -292.7805723015426338 ) ) ;
#23370 = CARTESIAN_POINT ( 'NONE',  ( -109.9731005101578631, -290.8154837541315487, -263.0344759800364614 ) ) ;
#23371 = ORIENTED_EDGE ( 'NONE', *, *, #3993, .F. ) ;
#23372 = DIRECTION ( 'NONE',  ( -1.000000000000000000, 0.000000000000000000, 0.000000000000000000 ) ) ;
#23373 = CARTESIAN_POINT ( 'NONE',  ( -84.46694427061599697, -299.2715530945168325, -211.0356020364245353 ) ) ;
#23374 = CARTESIAN_POINT ( 'NONE',  ( -10.47243879690600288, -273.1898464362398045, -198.5686975274963402 ) ) ;
#23375 = ORIENTED_EDGE ( 'NONE', *, *, #85804, .T. ) ;
#23376 = CARTESIAN_POINT ( 'NONE',  ( 20.76964992338365690, -275.7419473887630375, -320.8052354438478346 ) ) ;
#23377 = CARTESIAN_POINT ( 'NONE',  ( -39.16627194019173430, -296.5087532886450390, -196.6778457893443601 ) ) ;
#23378 = CARTESIAN_POINT ( 'NONE',  ( -57.47051235682460657, -281.6499796111602905, -198.9069620776855629 ) ) ;
#23379 = CARTESIAN_POINT ( 'NONE',  ( 17.42670940123061740, -274.3988775921335446, -320.4928113953597517 ) ) ;
#23380 = CARTESIAN_POINT ( 'NONE',  ( -94.02612215519287986, -274.2877440152159352, -223.8538272194856802 ) ) ;
#23381 = CARTESIAN_POINT ( 'NONE',  ( -90.37523738873673551, -274.2195596235882249, -219.8368037000986703 ) ) ;
#23382 = CARTESIAN_POINT ( 'NONE',  ( 74.89888025017330619, -301.0353604444513849, -194.1311006668066739 ) ) ;
#23383 = CARTESIAN_POINT ( 'NONE',  ( -34.14713859778311900, -272.1122560616433361, -195.0736583253548417 ) ) ;
#23384 = CARTESIAN_POINT ( 'NONE',  ( -34.28864567643706351, -295.6641704521555880, -343.3992691567017914 ) ) ;
#23385 = CARTESIAN_POINT ( 'NONE',  ( 36.21083636208848588, -292.0964652252480391, -268.0374804507874842 ) ) ;
#23386 = DIRECTION ( 'NONE',  ( 0.000000000000000000, 0.000000000000000000, 1.000000000000000000 ) ) ;
#23387 = CARTESIAN_POINT ( 'NONE',  ( -54.11172239103611048, -277.7541360401057204, -345.5042831394254108 ) ) ;
#23388 = CARTESIAN_POINT ( 'NONE',  ( -1.724484571943819766, -274.7048162735077312, -206.6254271636781823 ) ) ;
#23389 = B_SPLINE_CURVE_WITH_KNOTS ( 'NONE', 3,
 ( #24302, #31426, #82058, #38027, #81136, #68338 ),
 .UNSPECIFIED., .F., .F.,
 ( 4, 2, 4 ),
 ( 0.000000000000000000, 0.0004262108901887199383, 0.0008524217803774398767 ),
 .UNSPECIFIED. ) ;
#23390 =( BOUNDED_CURVE ( )  B_SPLINE_CURVE ( 3, ( #43445, #64803, #79452, #72793 ),
 .UNSPECIFIED., .F., .F. ) 
 B_SPLINE_CURVE_WITH_KNOTS ( ( 4, 4 ),
 ( 0.000000000000000000, 1.112150975886356141 ),
 .UNSPECIFIED. ) 
 CURVE ( )  GEOMETRIC_REPRESENTATION_ITEM ( )  RATIONAL_B_SPLINE_CURVE ( ( 1.000000000000000000, 0.8995554851226789106, 0.8995554851226789106, 1.000000000000000000 ) ) 
 REPRESENTATION_ITEM ( '' )  );
#23391 = CARTESIAN_POINT ( 'NONE',  ( -103.9956589051564890, -282.7452900616530087, -308.0257229134611521 ) ) ;
#23392 = CARTESIAN_POINT ( 'NONE',  ( -108.5994234780850292, -298.2436910453701557, -294.2852749985610217 ) ) ;
#23393 = FACE_OUTER_BOUND ( 'NONE', #25682, .T. ) ;
#23394 =( BOUNDED_SURFACE ( )  B_SPLINE_SURFACE ( 3, 2, ( 
 ( #46635, #24885, #90193 ),
 ( #2647, #32459, #61359 ),
 ( #60413, #54221, #76947 ),
 ( #41879, #62277, #77413 ),
 ( #4500, #47097, #26760 ),
 ( #76004, #27225, #84498 ),
 ( #70336, #92535, #11607 ),
 ( #26281, #33378, #40922 ) ),
 .UNSPECIFIED., .F., .F., .F. ) 
 B_SPLINE_SURFACE_WITH_KNOTS ( ( 4, 2, 2, 4 ),
 ( 3, 3 ),
 ( 1.734723475976807094E-18, 0.004223792520783738701, 0.006335688781175607617, 0.008447585041567475667 ),
 ( 0.000000000000000000, 1.000000000000000000 ),
 .UNSPECIFIED. ) 
 GEOMETRIC_REPRESENTATION_ITEM ( )  RATIONAL_B_SPLINE_SURFACE ( (
 ( 1.000000000000000000, 0.7071067811865475727, 1.000000000000000000),
 ( 1.000000000000000000, 0.7191403781184192434, 1.000000000000000000),
 ( 1.000000000000000000, 0.7377564866452818171, 1.000000000000000000),
 ( 1.000000000000000000, 0.7710512730017622385, 1.000000000000000000),
 ( 1.000000000000000000, 0.7830816923593137968, 1.000000000000000000),
 ( 1.000000000000000000, 0.8079768302254115575, 1.000000000000000000),
 ( 1.000000000000000000, 0.8207366415440850993, 1.000000000000000000),
 ( 1.000000000000000000, 0.8333723006562868685, 1.000000000000000000) ) ) 
 REPRESENTATION_ITEM ( '' )  SURFACE ( )  );
#23395 = CARTESIAN_POINT ( 'NONE',  ( -79.39376050813815766, -284.6655375083424246, -210.4305239951248154 ) ) ;
#23396 = AXIS2_PLACEMENT_3D ( 'NONE', #37435, #67277, #50734 ) ;
#23397 = CARTESIAN_POINT ( 'NONE',  ( -68.45150373048697645, -281.4597367707630724, -338.8018569790756942 ) ) ;
#23398 = CARTESIAN_POINT ( 'NONE',  ( -107.3966977611688094, -277.1068782013626901, -246.3235212932698630 ) ) ;
#23399 = CARTESIAN_POINT ( 'NONE',  ( -48.71668498755099819, -275.7744186996101234, -343.1177008166039855 ) ) ;
#23400 = CARTESIAN_POINT ( 'NONE',  ( 30.85635034804982979, -283.1412119372277516, -239.0284951441596490 ) ) ;
#23401 = CARTESIAN_POINT ( 'NONE',  ( 29.52227771575282489, -277.1630046710104125, -300.6322093164892522 ) ) ;
#23402 = CARTESIAN_POINT ( 'NONE',  ( 155.0193286407022981, 19.71512530817699016, 13.29403319965802410 ) ) ;
#23403 = CARTESIAN_POINT ( 'NONE',  ( 32.28048319347293216, -274.3514764125042689, -301.3319430120811262 ) ) ;
#23404 = CARTESIAN_POINT ( 'NONE',  ( -40.94657607603063809, -282.0070757796791554, -195.2680576550856983 ) ) ;
#23405 = CARTESIAN_POINT ( 'NONE',  ( 152.4536156746142410, 275.0000000000000568, -11.50000000000000355 ) ) ;
#23406 = CARTESIAN_POINT ( 'NONE',  ( -37.99499693586979987, -287.9641754973689558, -194.8039382734148148 ) ) ;
#23407 = CARTESIAN_POINT ( 'NONE',  ( -110.2140130185359368, -271.2396475792842807, -270.3444066551136871 ) ) ;
#23408 = CARTESIAN_POINT ( 'NONE',  ( -53.68086286175488908, -289.8424574493982391, -197.1099487432183821 ) ) ;
#23409 = AXIS2_PLACEMENT_3D ( 'NONE', #71924, #85164, #86544 ) ;
#23410 = CARTESIAN_POINT ( 'NONE',  ( 113.5000000000000568, -298.0521521680024080, -397.9547385950631337 ) ) ;
#23411 = CARTESIAN_POINT ( 'NONE',  ( -79.94613302176524883, -296.2560916027570670, -210.5949670137222824 ) ) ;
#23412 = CARTESIAN_POINT ( 'NONE',  ( -109.9131720686559390, -288.8944701100449493, -254.7327161467352141 ) ) ;
#23413 = CARTESIAN_POINT ( 'NONE',  ( 2.709286185474054420, -58.23210827017373248, -348.3322198635470954 ) ) ;
#23414 = CARTESIAN_POINT ( 'NONE',  ( 10.54962298731482839, -296.6514948947842640, -195.3774371216965164 ) ) ;
#23415 = CARTESIAN_POINT ( 'NONE',  ( 16.18567835318193460, -286.7895243775723202, -324.8177292032018499 ) ) ;
#23416 = CARTESIAN_POINT ( 'NONE',  ( -51.14779310791936950, -284.8315542291692850, -342.9103760623195285 ) ) ;
#23417 = CARTESIAN_POINT ( 'NONE',  ( -62.84001718050091512, -283.9645456850599317, -198.7803255844399075 ) ) ;
#23418 = CARTESIAN_POINT ( 'NONE',  ( -109.2767602435404228, -290.7198480589157725, -257.6488530210459089 ) ) ;
#23419 = CARTESIAN_POINT ( 'NONE',  ( 25.63118785651181142, -282.4563228996513544, -232.1862957384384174 ) ) ;
#23420 = CARTESIAN_POINT ( 'NONE',  ( 7.901823547758239030, -283.2189089445976151, -327.9203933308711498 ) ) ;
#23421 = CARTESIAN_POINT ( 'NONE',  ( -8.831554727571921504, -290.6609471553683193, -340.1287799265948593 ) ) ;
#23422 = CARTESIAN_POINT ( 'NONE',  ( -40.44238317311387476, -298.1809966196762502, -193.3714470020651106 ) ) ;
#23423 = CARTESIAN_POINT ( 'NONE',  ( -8.800162087940272215, -286.7615306336245453, -340.3372107325507159 ) ) ;
#23424 = CARTESIAN_POINT ( 'NONE',  ( -2.557543758611196871, -274.4993504954848049, -201.6509825507039295 ) ) ;
#23425 = CARTESIAN_POINT ( 'NONE',  ( -67.24565010694620071, -293.6379794294977046, -201.9681316400787807 ) ) ;
#23426 = DIRECTION ( 'NONE',  ( 0.000000000000000000, 0.000000000000000000, -1.000000000000000000 ) ) ;
#23427 = CARTESIAN_POINT ( 'NONE',  ( -20.19161114001083490, -285.3376638359844719, -345.3538533559490702 ) ) ;
#23428 = CARTESIAN_POINT ( 'NONE',  ( -111.8952730818596280, -276.6797949464923931, -260.3853060289647487 ) ) ;
#23429 = CARTESIAN_POINT ( 'NONE',  ( 209.5571421737558353, 36.99274597021241107, 12.09245862095555601 ) ) ;
#23430 = CARTESIAN_POINT ( 'NONE',  ( -75.36287091201697308, -295.9543105265284453, -204.2639812833216695 ) ) ;
#23431 = CARTESIAN_POINT ( 'NONE',  ( 19.94054786046952543, -274.2603739588362828, -224.9248247189719336 ) ) ;
#23432 = CARTESIAN_POINT ( 'NONE',  ( -101.7388825753190389, -292.5587986142359114, -234.4273512581287946 ) ) ;
#23433 = CARTESIAN_POINT ( 'NONE',  ( -106.7982333311414465, -291.8008097581132461, -247.1404710609513415 ) ) ;
#23434 = CARTESIAN_POINT ( 'NONE',  ( -91.46742973379453190, -285.5962275565122468, -320.8425938768648393 ) ) ;
#23435 = CARTESIAN_POINT ( 'NONE',  ( 22.63419704107917596, -294.3390496182859692, -222.9957548681978778 ) ) ;
#23436 = CARTESIAN_POINT ( 'NONE',  ( 19.04083200773630224, -294.1591926123075496, -218.6474027522131678 ) ) ;
#23437 = CARTESIAN_POINT ( 'NONE',  ( 25.79159982292571485, -293.8882793100639219, -307.0106260527365407 ) ) ;
#23438 = CARTESIAN_POINT ( 'NONE',  ( 36.97445196070918882, -289.4177090016124225, -259.8777638137207759 ) ) ;
#23439 = CARTESIAN_POINT ( 'NONE',  ( 25.93153829849026337, -282.2987629140076251, -314.2647969230076797 ) ) ;
#23440 = CARTESIAN_POINT ( 'NONE',  ( -70.08253734947092539, -295.7040313650891790, -202.2630138902113970 ) ) ;
#23441 = CARTESIAN_POINT ( 'NONE',  ( -71.06431610092320739, -285.4526513453951679, -201.1383964491991776 ) ) ;
#23442 = CARTESIAN_POINT ( 'NONE',  ( 34.48735205319458430, -277.7951493866578403, -290.7164237667528823 ) ) ;
#23443 = CARTESIAN_POINT ( 'NONE',  ( -83.88789911814953371, -284.1915253829378116, -213.5449223988324547 ) ) ;
#23444 = CARTESIAN_POINT ( 'NONE',  ( 4.421944806646524562, -286.4885950570701993, -332.6571741056147857 ) ) ;
#23445 = CARTESIAN_POINT ( 'NONE',  ( -58.92719763480694439, -277.9153763641402861, -197.7362477542605461 ) ) ;
#23446 = CARTESIAN_POINT ( 'NONE',  ( -49.37856652629597676, -155.6656457446864010, -366.7448178265262868 ) ) ;
#23447 = CARTESIAN_POINT ( 'NONE',  ( -110.0550090738036744, -284.1602869175135311, -262.7374027660993079 ) ) ;
#23448 = CARTESIAN_POINT ( 'NONE',  ( 39.31301473653432765, -282.7516456136942793, -269.9171724271684525 ) ) ;
#23449 = CARTESIAN_POINT ( 'NONE',  ( -106.3074097421376365, -289.1753056467402985, -304.1947568983028418 ) ) ;
#23450 = CARTESIAN_POINT ( 'NONE',  ( -84.35660642430981682, -279.2866338203835994, -330.3951334378114097 ) ) ;
#23451 = ADVANCED_FACE ( 'NONE', ( #39890 ), #54164, .F. ) ;
#23452 = CARTESIAN_POINT ( 'NONE',  ( 14.56100101959348692, -277.6553809904083892, -326.6418474436669612 ) ) ;
#23454 = ADVANCED_FACE ( 'NONE', ( #45711 ), #66594, .F. ) ;
#23453 = CARTESIAN_POINT ( 'NONE',  ( -89.47209198682517695, -279.1258560742897998, -219.1874052828304968 ) ) ;
#23455 = CARTESIAN_POINT ( 'NONE',  ( -91.38712892237528251, -299.2815941995733624, -218.5267148475721797 ) ) ;
#23456 = CARTESIAN_POINT ( 'NONE',  ( 37.46143141386919950, -285.5971482509502835, -273.8705863856440601 ) ) ;
#23457 = CARTESIAN_POINT ( 'NONE',  ( -111.8619470053454137, -292.3541002016450534, -254.3880597077790640 ) ) ;
#23458 = CARTESIAN_POINT ( 'NONE',  ( -0.6149505866814742872, -293.4725366883398578, -333.8648693268341958 ) ) ;
#23459 = VERTEX_POINT ( 'NONE', #31539 ) ;
#23460 = CARTESIAN_POINT ( 'NONE',  ( 10.30210858037631638, -294.0397776248563559, -325.6978596506181702 ) ) ;
#23461 = CARTESIAN_POINT ( 'NONE',  ( -111.2404196005671793, -291.3738785194781826, -290.8665263092275381 ) ) ;
#23462 = AXIS2_PLACEMENT_3D ( 'NONE', #75697, #46338, #67677 ) ;
#23463 = CARTESIAN_POINT ( 'NONE',  ( -67.35571448802896555, -280.2992433411040452, -203.6912722524530466 ) ) ;
#23464 = CARTESIAN_POINT ( 'NONE',  ( 30.46245456227480730, -297.8026840890044014, -193.6823012627349101 ) ) ;
#23465 = CARTESIAN_POINT ( 'NONE',  ( 39.24666770736248367, -288.2899038058766905, -277.2556592056690192 ) ) ;
#23466 = CARTESIAN_POINT ( 'NONE',  ( -38.91548642885345544, -289.4046705166271067, -347.3238848786846802 ) ) ;
#23467 = CARTESIAN_POINT ( 'NONE',  ( -81.49473269013293475, -285.7655515821485324, -212.2010182383625931 ) ) ;
#23468 = DIRECTION ( 'NONE',  ( 0.000000000000000000, 0.000000000000000000, -1.000000000000000000 ) ) ;
#23469 = CARTESIAN_POINT ( 'NONE',  ( 199.9777737730213119, 292.7032345016298791, -82.77980196592716311 ) ) ;
#23470 = CARTESIAN_POINT ( 'NONE',  ( 160.4524113272230181, 217.9076703733470879, -202.3092286760552554 ) ) ;
#23471 = CARTESIAN_POINT ( 'NONE',  ( -21.62828341911615482, -276.0428233677268963, -341.8673366536299909 ) ) ;
#23472 = CARTESIAN_POINT ( 'NONE',  ( -59.30063096982176063, -276.2635352555924442, -340.3041764608137214 ) ) ;
#23473 = CARTESIAN_POINT ( 'NONE',  ( -114.3205561439198874, -272.2189246291147811, -270.3568838636807641 ) ) ;
#23474 = CARTESIAN_POINT ( 'NONE',  ( 46.79431152631179458, 10.63313198298185114, -329.4643313189536116 ) ) ;
#23475 = CARTESIAN_POINT ( 'NONE',  ( -79.96542937547629037, -276.3001900730918692, -333.9584828280872557 ) ) ;
#23476 = CARTESIAN_POINT ( 'NONE',  ( -55.80212160902548391, -297.0467995301833071, -344.0712723038736272 ) ) ;
#23477 = AXIS2_PLACEMENT_3D ( 'NONE', #91322, #84226, #18917 ) ;
#23478 = CARTESIAN_POINT ( 'NONE',  ( 6.708358894044986975, -293.1622806422601002, -212.0723476952181841 ) ) ;
#23479 = CARTESIAN_POINT ( 'NONE',  ( -65.49238998103280096, -298.4962842910365453, -198.8081086969549460 ) ) ;
#23480 = CARTESIAN_POINT ( 'NONE',  ( -36.19182844920897679, -298.5585315653030989, -193.4225628156010828 ) ) ;
#23481 = CARTESIAN_POINT ( 'NONE',  ( -106.7074509629423176, -297.0226299362166742, -247.4545826240741917 ) ) ;
#23482 = EDGE_LOOP ( 'NONE', ( #60303, #81125, #60140, #63694, #79397, #69219 ) ) ;
#23483 = CARTESIAN_POINT ( 'NONE',  ( 188.7399167944524550, -12.49482340714361506, 10.00000000000000000 ) ) ;
#23484 = CARTESIAN_POINT ( 'NONE',  ( -71.87099015364437093, -281.5195575060055830, -203.1377934289358507 ) ) ;
#23485 = CARTESIAN_POINT ( 'NONE',  ( 15.70656479875309408, -281.8327126843012138, -326.0873101309804269 ) ) ;
#23486 = CARTESIAN_POINT ( 'NONE',  ( -107.4080032043713118, -279.3453949281718565, -292.0934459617955667 ) ) ;
#23487 = CARTESIAN_POINT ( 'NONE',  ( -105.2797664069807126, -280.7572521816142626, -236.2086864157508330 ) ) ;
#23488 = CARTESIAN_POINT ( 'NONE',  ( -63.53523545373780479, -272.1843679650526155, -201.4663940986789896 ) ) ;
#23489 = CARTESIAN_POINT ( 'NONE',  ( 196.2715852227941866, 71.88751843463604985, -11.58297462746890538 ) ) ;
#23490 = CARTESIAN_POINT ( 'NONE',  ( 175.2296996224750103, 154.6894116713782807, 24.16304133878946558 ) ) ;
#23491 = CARTESIAN_POINT ( 'NONE',  ( 17.96313950408061544, -281.0400251356763874, -222.6934809092687715 ) ) ;
#23492 = CARTESIAN_POINT ( 'NONE',  ( 37.12620247485178027, -276.1174930344740233, -251.4219970159843456 ) ) ;
#23493 = CARTESIAN_POINT ( 'NONE',  ( 36.22568031408611944, -277.7396327974316819, -284.9501956354350227 ) ) ;
#23494 = CARTESIAN_POINT ( 'NONE',  ( -112.7208955753931292, -276.9691810318370244, -282.8744383690524273 ) ) ;
#23495 = ORIENTED_EDGE ( 'NONE', *, *, #2023, .T. ) ;
#23496 = CARTESIAN_POINT ( 'NONE',  ( 197.2991535282351379, 42.14527734682575755, 10.37297551676668839 ) ) ;
#23497 = CARTESIAN_POINT ( 'NONE',  ( -16.57048577135595835, -284.7651116773957938, -342.8511553626584600 ) ) ;
#23498 = CARTESIAN_POINT ( 'NONE',  ( -75.05409881503862835, -290.7333507131862689, -207.6092600630848040 ) ) ;
#23499 = CARTESIAN_POINT ( 'NONE',  ( -20.99753407276626405, -285.6051818535179905, -195.2200438471334962 ) ) ;
#23500 = CARTESIAN_POINT ( 'NONE',  ( -103.9340603573664623, -282.3593196420072218, -302.7810863540076980 ) ) ;
#23502 = CARTESIAN_POINT ( 'NONE',  ( 30.12517940097567148, -285.2154656458999966, -238.9042528891214658 ) ) ;
#23501 = CARTESIAN_POINT ( 'NONE',  ( -15.97864367260608276, -281.3450961218981661, -340.7812481641582849 ) ) ;
#23503 = CARTESIAN_POINT ( 'NONE',  ( 9.518319208454666835, -281.9181137974733815, -213.8035582641167025 ) ) ;
#23504 = CARTESIAN_POINT ( 'NONE',  ( 168.2163488282115225, 233.8014272134587941, -193.1015290748493385 ) ) ;
#23505 = CARTESIAN_POINT ( 'NONE',  ( 25.26132950738688976, -280.5322397052373162, -313.8271366257532122 ) ) ;
#23506 = CARTESIAN_POINT ( 'NONE',  ( 29.11463320946414157, -295.0905173511296766, -235.4850882693889957 ) ) ;
#23507 = CARTESIAN_POINT ( 'NONE',  ( -66.50191932104934267, -287.6713123427426808, -201.0811782817712583 ) ) ;
#23508 = DIRECTION ( 'NONE',  ( -1.000000000000000000, 0.000000000000000000, 0.000000000000000000 ) ) ;
#23509 = CARTESIAN_POINT ( 'NONE',  ( -41.99026512915360598, -293.9141387681626156, -194.9442429315811580 ) ) ;
#23510 = CARTESIAN_POINT ( 'NONE',  ( 37.64300481556626465, -273.5325373231307822, -268.8463010935575426 ) ) ;
#23511 = CARTESIAN_POINT ( 'NONE',  ( 32.71345748152251787, -287.1533847503155812, -301.9274562608538304 ) ) ;
#23512 = CARTESIAN_POINT ( 'NONE',  ( 35.10587121427636959, -292.1355343636108159, -284.4248949795370436 ) ) ;
#23513 = DIRECTION ( 'NONE',  ( 0.000000000000000000, 1.000000000000000000, 0.000000000000000000 ) ) ;
#23514 = CARTESIAN_POINT ( 'NONE',  ( -76.63353191152623367, -276.2744616560302120, -332.5289114047803309 ) ) ;
#23515 = CARTESIAN_POINT ( 'NONE',  ( -111.6094868382501488, -294.7135145379022561, -268.6817049044715873 ) ) ;
#23516 = CARTESIAN_POINT ( 'NONE',  ( -110.7983922557024385, -291.8203126241483005, -273.9496247675755285 ) ) ;
#23517 = CARTESIAN_POINT ( 'NONE',  ( 221.8344101925596021, 1.000000000000000444, 8.171572875253808377 ) ) ;
#23518 = CARTESIAN_POINT ( 'NONE',  ( -83.63170945779074827, -298.0521521680024080, -517.1711561948568487 ) ) ;
#23519 = CARTESIAN_POINT ( 'NONE',  ( 37.08935566046246635, -291.8191707954212006, -253.4880171775016890 ) ) ;
#23520 = CARTESIAN_POINT ( 'NONE',  ( 33.85909981965790649, -289.4082111814997802, -289.9645185982417388 ) ) ;
#23521 = CARTESIAN_POINT ( 'NONE',  ( -107.8664126688921101, -288.4282312385181513, -298.6496126896894907 ) ) ;
#23522 = CARTESIAN_POINT ( 'NONE',  ( 35.85866687328238811, -288.8785630501906780, -262.8059086996532869 ) ) ;
#23523 = CYLINDRICAL_SURFACE ( 'NONE', #56248, 4.999999999999990230 ) ;
#23524 = CARTESIAN_POINT ( 'NONE',  ( 11.23365076474864921, -287.5481937864954602, -215.5844037493591259 ) ) ;
#23525 = CARTESIAN_POINT ( 'NONE',  ( -6.448457155595283652, -296.6283075887543532, -339.0925834451596188 ) ) ;
#23526 = LINE ( 'NONE', #87893, #47358 ) ;
#23527 = CARTESIAN_POINT ( 'NONE',  ( -75.45274609958812562, -290.7538245273672715, -336.8107748187499055 ) ) ;
#23528 = CARTESIAN_POINT ( 'NONE',  ( -25.62591083777251910, -278.2208301491812676, -195.9222364639070975 ) ) ;
#23529 = CARTESIAN_POINT ( 'NONE',  ( -62.39509707870276856, -277.7024976222360237, -343.2052629585372188 ) ) ;
#23530 = CARTESIAN_POINT ( 'NONE',  ( -88.91413412554706497, -279.0173557941939180, -213.2119417590596129 ) ) ;
#23531 = CARTESIAN_POINT ( 'NONE',  ( -72.46065280030273925, -299.5648933895737400, -204.4792619127440219 ) ) ;
#23532 = CARTESIAN_POINT ( 'NONE',  ( -33.10077252724253327, -284.1052760838761628, -195.4299285963734008 ) ) ;
#23533 = CARTESIAN_POINT ( 'NONE',  ( -48.18343439339133738, -256.1235685800110673, -485.9512705677856275 ) ) ;
#23534 = CARTESIAN_POINT ( 'NONE',  ( -38.34717579188062331, -278.1790047405590940, -196.1201137718282723 ) ) ;
#23535 = CARTESIAN_POINT ( 'NONE',  ( -33.19545634619050389, -280.9997982591336836, -345.2592196878421760 ) ) ;
#23536 = DIRECTION ( 'NONE',  ( -0.000000000000000000, -1.000000000000000000, -0.000000000000000000 ) ) ;
#23537 = CARTESIAN_POINT ( 'NONE',  ( -48.41270154851726915, -275.6703622962211853, -345.9138047990541622 ) ) ;
#23538 = AXIS2_PLACEMENT_3D ( 'NONE', #16372, #44776, #308 ) ;
#23539 = CARTESIAN_POINT ( 'NONE',  ( -103.3809674688449007, -297.6317489508992935, -303.1799350553461636 ) ) ;
#23540 = CARTESIAN_POINT ( 'NONE',  ( -81.39528169475926234, -282.5558487563033623, -333.2013193362076322 ) ) ;
#23541 = CARTESIAN_POINT ( 'NONE',  ( -101.4262312441805278, -297.9763214060499195, -234.9128272036355440 ) ) ;
#23542 = CARTESIAN_POINT ( 'NONE',  ( -112.4921638422901111, -274.1551650546416568, -256.2574839311059236 ) ) ;
#23543 = CARTESIAN_POINT ( 'NONE',  ( -6.271483248217240458, -276.2990689888347333, -336.4561211331753725 ) ) ;
#23544 = CARTESIAN_POINT ( 'NONE',  ( 22.94900238363420542, -296.1610629447498582, -314.9708909259636016 ) ) ;
#23545 = CARTESIAN_POINT ( 'NONE',  ( 10.22961282020613716, -288.5834803138327516, -330.9762068367739403 ) ) ;
#23546 = CARTESIAN_POINT ( 'NONE',  ( -81.37939867735384780, -277.5382371918254307, -208.9608305079144941 ) ) ;
#23547 = CARTESIAN_POINT ( 'NONE',  ( -100.6818060166591806, -289.8072537748542459, -314.1450304451814191 ) ) ;
#23548 = ADVANCED_FACE ( 'NONE', ( #87872 ), #30599, .F. ) ;
#23549 = CARTESIAN_POINT ( 'NONE',  ( -107.1801026994411075, -289.3176068332623458, -292.5744800926738094 ) ) ;
#23550 = CARTESIAN_POINT ( 'NONE',  ( 35.81623944262175741, -291.3392100435644920, -253.7832622219589496 ) ) ;
#23551 = EDGE_LOOP ( 'NONE', ( #14876, #23699, #49436, #84236 ) ) ;
#23552 = CARTESIAN_POINT ( 'NONE',  ( 196.9829714441682427, 72.62824309771482945, 12.32222797397095704 ) ) ;
#23553 = CARTESIAN_POINT ( 'NONE',  ( -96.80779806890419081, -290.6533868864454462, -227.8282724568342132 ) ) ;
#23554 = FACE_OUTER_BOUND ( 'NONE', #33852, .T. ) ;
#23555 = CARTESIAN_POINT ( 'NONE',  ( -54.92239823472858973, -286.7726919984503979, -195.6366958278105983 ) ) ;
#23556 = CARTESIAN_POINT ( 'NONE',  ( -82.08285599513421005, -286.1948066931273615, -326.5171145203363494 ) ) ;
#23557 = CARTESIAN_POINT ( 'NONE',  ( 36.14094849259062414, -292.8925313064224838, -292.7474091686557358 ) ) ;
#23558 = EDGE_CURVE ( 'NONE', #3067, #11722, #66143, .T. ) ;
#23559 = CARTESIAN_POINT ( 'NONE',  ( 11.19276923560565606, -283.7115161180572613, -329.5710712945125351 ) ) ;
#23560 = CARTESIAN_POINT ( 'NONE',  ( -109.4207908131238725, -284.5389947961608641, -258.7232033088644130 ) ) ;
#23561 = CARTESIAN_POINT ( 'NONE',  ( 36.09560996715755010, -276.9192415102693303, -274.3226278999974852 ) ) ;
#23562 = CARTESIAN_POINT ( 'NONE',  ( -30.63462814121000832, -290.1574822226092465, -196.0182502149615686 ) ) ;
#23563 = CARTESIAN_POINT ( 'NONE',  ( 22.61400874048008092, -273.7590846117007004, -228.0020968140500202 ) ) ;
#23564 = ORIENTED_EDGE ( 'NONE', *, *, #31692, .T. ) ;
#23565 = CARTESIAN_POINT ( 'NONE',  ( -78.59295187722810283, -208.2960365483323244, -357.4574221067172743 ) ) ;
#23566 = CARTESIAN_POINT ( 'NONE',  ( -36.27899912000115989, -294.7059279999600676, -347.3457386169311008 ) ) ;
#23567 = CARTESIAN_POINT ( 'NONE',  ( -19.49382052750853234, -288.2036628583100537, -198.0924014539831148 ) ) ;
#23568 = CARTESIAN_POINT ( 'NONE',  ( -92.46523033144005410, -296.8984075073406075, -323.6798663498537394 ) ) ;
#23569 = CARTESIAN_POINT ( 'NONE',  ( -33.24122393159622391, -286.7564215905910032, -197.3243884534402639 ) ) ;
#23570 = CARTESIAN_POINT ( 'NONE',  ( -111.8546203887142809, -277.8431189493210809, -251.8506538120986988 ) ) ;
#23571 = CARTESIAN_POINT ( 'NONE',  ( 26.40374852036649855, -293.6350272628185962, -227.2578057689176489 ) ) ;
#23572 = CARTESIAN_POINT ( 'NONE',  ( -0.2990882997848233193, -284.6788213662377984, -204.2543252490236796 ) ) ;
#23573 = CARTESIAN_POINT ( 'NONE',  ( 25.69977724022104226, -294.4699911791835234, -314.5600954182273767 ) ) ;
#23574 = CARTESIAN_POINT ( 'NONE',  ( -101.1442168695890160, -291.3721488760276657, -234.7420961536823256 ) ) ;
#23575 = CARTESIAN_POINT ( 'NONE',  ( 196.0143093133015384, 73.40565171261611965, -12.00000000000000355 ) ) ;
#23576 = CARTESIAN_POINT ( 'NONE',  ( 196.0143093133015384, 250.0000000000000568, 11.99999999999998757 ) ) ;
#23577 = CARTESIAN_POINT ( 'NONE',  ( 201.5944599935328370, 289.7950610217533836, -82.37615236527834384 ) ) ;
#23578 = CARTESIAN_POINT ( 'NONE',  ( -62.98680599413593484, -287.2442800355714780, -198.4929310210908966 ) ) ;
#23579 = CARTESIAN_POINT ( 'NONE',  ( 44.71564893372296723, -273.0523547857346784, -270.3937649182068412 ) ) ;
#23580 = VERTEX_POINT ( 'NONE', #38627 ) ;
#23581 = CARTESIAN_POINT ( 'NONE',  ( -24.02276734314449769, -281.7983367913138864, -342.4501747263089442 ) ) ;
#23582 = CARTESIAN_POINT ( 'NONE',  ( -106.3283173799112262, -277.7784303942466977, -304.6364541672766109 ) ) ;
#23583 = CARTESIAN_POINT ( 'NONE',  ( 32.77948886033910014, -283.2105256915716609, -244.0774173914742846 ) ) ;
#23584 = CARTESIAN_POINT ( 'NONE',  ( -107.4366190058017452, -267.2042186947507503, -306.5197711127555067 ) ) ;
#23585 = CARTESIAN_POINT ( 'NONE',  ( -70.23306157161640328, -282.0517770589909787, -339.3447723352304592 ) ) ;
#23586 = CARTESIAN_POINT ( 'NONE',  ( 37.19670806341779468, -285.5095962568583445, -265.5042523385958475 ) ) ;
#23587 = CARTESIAN_POINT ( 'NONE',  ( 30.13923431255202701, -276.9616627408163367, -235.9136367270153869 ) ) ;
#23588 = CARTESIAN_POINT ( 'NONE',  ( -70.50107694906718336, -298.0950670391416111, -205.2438596243530355 ) ) ;
#23589 = CARTESIAN_POINT ( 'NONE',  ( -2.927558067487958215, -293.2720838604775508, -335.2988597454757951 ) ) ;
#23590 = CARTESIAN_POINT ( 'NONE',  ( -104.8820951776833112, -278.7271707259505433, -307.1253373111703695 ) ) ;
#23591 = CARTESIAN_POINT ( 'NONE',  ( -37.80975951750138364, -277.0581396920400721, -343.3720703023441843 ) ) ;
#23592 = CARTESIAN_POINT ( 'NONE',  ( -112.7668337591357215, -273.8096200108537914, -256.2013796315380887 ) ) ;
#23593 = CARTESIAN_POINT ( 'NONE',  ( -104.7106323510944037, -276.9963648012179078, -307.0069837805684188 ) ) ;
#23594 = CARTESIAN_POINT ( 'NONE',  ( -84.39908107233776491, -219.2962774960793979, -352.3863144506248091 ) ) ;
#23595 = CARTESIAN_POINT ( 'NONE',  ( 10.67323324769085247, -274.3889048359586127, -328.0435385926230083 ) ) ;
#23596 = CARTESIAN_POINT ( 'NONE',  ( -111.7051398859757683, -298.1988547736701776, -252.7916808038707188 ) ) ;
#23597 = LINE ( 'NONE', #52464, #86857 ) ;
#23598 = DIRECTION ( 'NONE',  ( -0.000000000000000000, -1.000000000000000000, -0.000000000000000000 ) ) ;
#23599 = CARTESIAN_POINT ( 'NONE',  ( -68.74690798376259693, -285.2194302501843595, -339.5684534487003248 ) ) ;
#23600 = CARTESIAN_POINT ( 'NONE',  ( -77.09755191397748320, -284.8527762138687649, -208.9547915133703668 ) ) ;
#23601 = CARTESIAN_POINT ( 'NONE',  ( -103.8608281804737743, -276.5228849773250204, -302.4426294836409852 ) ) ;
#23602 = CARTESIAN_POINT ( 'NONE',  ( -74.39308335077448930, -285.4104486083722918, -334.7474456918561714 ) ) ;
#23603 = CARTESIAN_POINT ( 'NONE',  ( -106.1548236246012351, -277.3826046744385394, -243.8466796971943609 ) ) ;
#23604 = CARTESIAN_POINT ( 'NONE',  ( -1.306342928227328892, -277.6422220336684745, -334.2596121709232762 ) ) ;
#23605 = LINE ( 'NONE', #74251, #20069 ) ;
#23606 = CARTESIAN_POINT ( 'NONE',  ( -34.04417049204357681, -274.5870931576932890, -197.3740318639470956 ) ) ;
#23607 = TOROIDAL_SURFACE ( 'NONE', #6989, 5.654241149514406040, 0.5000000000000000000 ) ;
#23608 = CARTESIAN_POINT ( 'NONE',  ( 33.02097094963124846, -281.9604002381283294, -239.4863169495665431 ) ) ;
#23609 = CARTESIAN_POINT ( 'NONE',  ( 38.73291562117786668, -281.8962747702636875, -258.5188183353056957 ) ) ;
#23610 = ORIENTED_EDGE ( 'NONE', *, *, #52972, .T. ) ;
#23611 = ORIENTED_EDGE ( 'NONE', *, *, #88201, .T. ) ;
#23612 = CARTESIAN_POINT ( 'NONE',  ( 197.7323754217837006, 18.47808631420720715, -11.36704352365809889 ) ) ;
#23613 = CARTESIAN_POINT ( 'NONE',  ( 9.035670697446112953, -288.5415056901899788, -210.4491412741920158 ) ) ;
#23614 = CARTESIAN_POINT ( 'NONE',  ( -95.41100991186628733, -296.3742644784641129, -225.8372593236062755 ) ) ;
#23615 = CARTESIAN_POINT ( 'NONE',  ( -36.37131084586341956, -291.4126097395954957, -193.4561581629470766 ) ) ;
#23616 = CARTESIAN_POINT ( 'NONE',  ( 23.30962994678129974, -286.6097956958180362, -312.2417321816748768 ) ) ;
#23617 = CARTESIAN_POINT ( 'NONE',  ( -29.12520881523634486, -287.5207084020196362, -343.4902106005949918 ) ) ;
#23618 = CARTESIAN_POINT ( 'NONE',  ( -79.55010188561553264, -286.6731226058781772, -210.2522209410640812 ) ) ;
#23619 = CARTESIAN_POINT ( 'NONE',  ( -73.16458745200385749, -275.5268462611056179, -336.2674725587354487 ) ) ;
#23620 = CARTESIAN_POINT ( 'NONE',  ( -43.14193866221108209, -287.5241126698760468, -346.3400469592653508 ) ) ;
#23621 = CARTESIAN_POINT ( 'NONE',  ( -62.55372808273050822, -287.7242411624579290, -199.7257564820693005 ) ) ;
#23622 = CARTESIAN_POINT ( 'NONE',  ( -74.77335587903566250, -287.5491056496915121, -335.5447016130929114 ) ) ;
#23623 = CARTESIAN_POINT ( 'NONE',  ( 10.07011855260182465, -283.3212931710614271, -326.2447316867698532 ) ) ;
#23624 = CARTESIAN_POINT ( 'NONE',  ( -96.91134893754593804, -293.1791205058588616, -224.4983202420237660 ) ) ;
#23625 = CARTESIAN_POINT ( 'NONE',  ( 195.4781563537916043, 27.48493576247232895, 15.50000000000000000 ) ) ;
#23626 = CARTESIAN_POINT ( 'NONE',  ( 144.2857639756989272, -299.5541904835127980, -189.7068768330456123 ) ) ;
#23627 = CARTESIAN_POINT ( 'NONE',  ( -112.8982735732997185, -298.4814843182186905, -269.6411149513203895 ) ) ;
#23628 = EDGE_CURVE ( 'NONE', #30942, #49115, #66326, .T. ) ;
#23629 = CARTESIAN_POINT ( 'NONE',  ( 20.65017696660128266, -280.1227418842138377, -225.7364488081120157 ) ) ;
#23630 = CARTESIAN_POINT ( 'NONE',  ( 12.65758128666331039, -278.7492407457295371, -214.4587700520113458 ) ) ;
#23631 = CARTESIAN_POINT ( 'NONE',  ( 1.678608228784536971, -293.7413621927649956, -336.5545795642934195 ) ) ;
#23632 = CARTESIAN_POINT ( 'NONE',  ( -41.89759333070529124, -296.3936530147983603, -196.7018738034329886 ) ) ;
#23633 = CARTESIAN_POINT ( 'NONE',  ( 18.49956782502580666, -274.3215419306684453, -319.6049986156690466 ) ) ;
#23634 = CARTESIAN_POINT ( 'NONE',  ( -92.55013752300727958, -297.1794518962731217, -318.8716520887538195 ) ) ;
#23635 = CARTESIAN_POINT ( 'NONE',  ( 60.29495240252359878, -249.1689065933675238, 21.50000000000000000 ) ) ;
#23636 = CARTESIAN_POINT ( 'NONE',  ( -3.770512523477011602, -296.9451216367822894, -194.0629393281858768 ) ) ;
#23637 = CARTESIAN_POINT ( 'NONE',  ( -100.7946061276290521, -294.2339211616690591, -312.2618534305539697 ) ) ;
#23638 = CARTESIAN_POINT ( 'NONE',  ( 21.45372518083881630, -294.3609187266864637, -226.1064811485536836 ) ) ;
#23639 = PLANE ( 'NONE',  #92853 ) ;
#23640 = CARTESIAN_POINT ( 'NONE',  ( 30.97553211781579208, -294.0061167409050995, -244.1817844366976544 ) ) ;
#23641 = CYLINDRICAL_SURFACE ( 'NONE', #58087, 2.000000000000000000 ) ;
#23643 = CARTESIAN_POINT ( 'NONE',  ( 3.816386721421738848, -294.4806905750288024, -330.6521777417710837 ) ) ;
#23642 = CARTESIAN_POINT ( 'NONE',  ( -107.4879428154368242, -282.9304951549263478, -242.6891434258418485 ) ) ;
#23644 = CARTESIAN_POINT ( 'NONE',  ( -98.04442191513393823, -283.9191831028469437, -317.7338904119175709 ) ) ;
#23645 = CARTESIAN_POINT ( 'NONE',  ( -36.78813083755425595, -281.9792085351709261, -194.7903407221597547 ) ) ;
#23646 = CARTESIAN_POINT ( 'NONE',  ( 0.2771659567876044727, -286.2057095461482277, -203.1853325412872664 ) ) ;
#23647 = CARTESIAN_POINT ( 'NONE',  ( -103.2700900060842457, -288.0797640030843354, -305.8755136904109122 ) ) ;
#23648 = CARTESIAN_POINT ( 'NONE',  ( -54.49178911615187815, -280.7666405000204009, -345.3538533559490702 ) ) ;
#23649 = CARTESIAN_POINT ( 'NONE',  ( 19.05086839509208829, -285.5723561561008523, -223.2127284513679228 ) ) ;
#23650 = CARTESIAN_POINT ( 'NONE',  ( -109.1794400119410966, -289.8151225119756873, -243.3615450881882794 ) ) ;
#23651 = CARTESIAN_POINT ( 'NONE',  ( 206.6195589736935005, 30.30844190587211884, 15.00000000000000178 ) ) ;
#23652 = CARTESIAN_POINT ( 'NONE',  ( -6.411260363033599141, -296.2390725767519939, -337.3667021773065926 ) ) ;
#23653 = CARTESIAN_POINT ( 'NONE',  ( -111.5183373542898124, -280.2092604009340562, -251.9652789025995787 ) ) ;
#23655 = CARTESIAN_POINT ( 'NONE',  ( 31.09160564204640309, -280.8774598790478194, -244.7411384554898746 ) ) ;
#23654 = CARTESIAN_POINT ( 'NONE',  ( -1.510962052055676796, -292.5997228194920012, -336.6671985461200052 ) ) ;
#23656 = CARTESIAN_POINT ( 'NONE',  ( -37.68684804680010814, -295.2230053076495437, -347.3734229007654335 ) ) ;
#23657 = CARTESIAN_POINT ( 'NONE',  ( -94.70697914160658115, -283.3089630194299389, -221.1040267450195245 ) ) ;
#23658 = CARTESIAN_POINT ( 'NONE',  ( -91.64376406224226912, -281.2790824145236570, -218.5540490039744270 ) ) ;
#23659 = ADVANCED_FACE ( 'NONE', ( #25815 ), #40464, .F. ) ;
#23660 = CARTESIAN_POINT ( 'NONE',  ( -5.449845175431134336, -293.6807130319604084, -336.3015827400045623 ) ) ;
#23661 = CARTESIAN_POINT ( 'NONE',  ( -94.61386983468875655, -271.2244966725415338, -221.6594127210166505 ) ) ;
#23662 = VERTEX_POINT ( 'NONE', #54695 ) ;
#23663 = CARTESIAN_POINT ( 'NONE',  ( 189.9243309297870610, 250.5000000000000568, 20.22542485937349355 ) ) ;
#23664 = CARTESIAN_POINT ( 'NONE',  ( 36.77603671812038044, -283.6517312517378286, -279.6381901162179702 ) ) ;
#23665 = CARTESIAN_POINT ( 'NONE',  ( -100.2226289584829857, -295.5478707892269767, -307.6625933678001843 ) ) ;
#23666 = CARTESIAN_POINT ( 'NONE',  ( 208.4306832106270804, -199.2391364535880882, 0.000000000000000000 ) ) ;
#23667 = CARTESIAN_POINT ( 'NONE',  ( -4.829096099716524648, -274.1237833571632905, -337.9475929042657754 ) ) ;
#23668 = CARTESIAN_POINT ( 'NONE',  ( -18.57948399627296965, -273.4848991087040986, -195.7935311083072349 ) ) ;
#23669 = CARTESIAN_POINT ( 'NONE',  ( -31.84537720400900440, -290.2994674338366394, -346.7225023559164470 ) ) ;
#23670 = CARTESIAN_POINT ( 'NONE',  ( -108.3509113692800270, -290.1620906597057115, -287.2930972950791215 ) ) ;
#23671 = CARTESIAN_POINT ( 'NONE',  ( -22.06944292388590156, -281.7713492211050834, -198.2153180721255694 ) ) ;
#23672 = CARTESIAN_POINT ( 'NONE',  ( -43.56973256083086454, -275.5724403804326812, -196.7731117260306917 ) ) ;
#23673 = CARTESIAN_POINT ( 'NONE',  ( -36.99111024483472221, -278.8515612959367900, -196.9648810698413968 ) ) ;
#23674 = CARTESIAN_POINT ( 'NONE',  ( -21.19836542798471157, -278.8453654253348191, -343.6565583733109861 ) ) ;
#23675 = ORIENTED_EDGE ( 'NONE', *, *, #75724, .F. ) ;
#23676 = CARTESIAN_POINT ( 'NONE',  ( -85.80658563474980838, -273.2352961210023636, -210.5267225455737332 ) ) ;
#23677 = CARTESIAN_POINT ( 'NONE',  ( -58.07909303802962597, -293.7024421546607300, -198.8140131671668485 ) ) ;
#23678 = CARTESIAN_POINT ( 'NONE',  ( 180.7287904564219332, 275.5000000000000568, -24.90000000000003411 ) ) ;
#23679 = EDGE_CURVE ( 'NONE', #19395, #43024, #91126, .T. ) ;
#23680 = CARTESIAN_POINT ( 'NONE',  ( 161.2244399300530233, -11.64849832608277325, 13.00000000000000178 ) ) ;
#23681 = CARTESIAN_POINT ( 'NONE',  ( 21.26903376294168524, -291.0365544468612029, -222.3497926835745488 ) ) ;
#23682 = CARTESIAN_POINT ( 'NONE',  ( -105.4713553622504776, -272.4137758091697492, -243.8333662622118823 ) ) ;
#23683 = VECTOR ( 'NONE', #37611, 1000.000000000000000 ) ;
#23684 = LINE ( 'NONE', #2383, #70805 ) ;
#23685 = CARTESIAN_POINT ( 'NONE',  ( 14.94882903990264822, -294.2932183090470630, -214.7151357154085076 ) ) ;
#23686 = CARTESIAN_POINT ( 'NONE',  ( -55.63300648810263738, -300.3376638359844719, -190.3683826091709363 ) ) ;
#23687 = CARTESIAN_POINT ( 'NONE',  ( 17.29604931729026873, -288.8344578617546858, -219.2076403802323625 ) ) ;
#23688 = CARTESIAN_POINT ( 'NONE',  ( 28.36459331370843984, -274.0301895428460170, -306.2843399587681574 ) ) ;
#23689 = CARTESIAN_POINT ( 'NONE',  ( 12.49275071668670023, -276.6726242751695395, -214.9939777256952880 ) ) ;
#23690 = CARTESIAN_POINT ( 'NONE',  ( -73.30154083974619539, -289.6516149867449599, -205.1249540572253238 ) ) ;
#23691 = CARTESIAN_POINT ( 'NONE',  ( -47.96933495990111140, -281.7789060834294332, -195.2924112356211310 ) ) ;
#23692 = ORIENTED_EDGE ( 'NONE', *, *, #86200, .T. ) ;
#23693 = CARTESIAN_POINT ( 'NONE',  ( -29.44187087593311603, -282.2981713747406616, -343.0855205921752713 ) ) ;
#23694 = CARTESIAN_POINT ( 'NONE',  ( -112.9919834803592238, -279.4737202304755783, -282.9518740670446277 ) ) ;
#23695 = CARTESIAN_POINT ( 'NONE',  ( -8.204209013251229976, -281.4740211295047629, -341.2623691472579139 ) ) ;
#23696 = CARTESIAN_POINT ( 'NONE',  ( -72.72154477837992204, -278.4502987993755596, -338.5012982650375193 ) ) ;
#23697 = CARTESIAN_POINT ( 'NONE',  ( -8.131969979251900682, -278.1966032418925465, -340.8699522798682437 ) ) ;
#23698 = CARTESIAN_POINT ( 'NONE',  ( -82.08285599513421005, -286.1948066931273615, -326.5171145203363494 ) ) ;
#23699 = ORIENTED_EDGE ( 'NONE', *, *, #34031, .T. ) ;
#23700 = VERTEX_POINT ( 'NONE', #26297 ) ;
#23701 = CARTESIAN_POINT ( 'NONE',  ( -105.5477509207837414, -298.9631972017145927, -239.0441111789417903 ) ) ;
#23702 = CARTESIAN_POINT ( 'NONE',  ( -84.87504876384126362, -290.8052159675451662, -326.2385652259831659 ) ) ;
#23703 = CARTESIAN_POINT ( 'NONE',  ( -90.26948662756966257, -275.8249925059587326, -323.0700456038410380 ) ) ;
#23704 = CARTESIAN_POINT ( 'NONE',  ( -59.70734677668481538, -291.0981220780837475, -342.9817201686347516 ) ) ;
#23705 = CARTESIAN_POINT ( 'NONE',  ( -33.49478737170256437, -291.4504024451915711, -197.3479650668444094 ) ) ;
#23706 = CARTESIAN_POINT ( 'NONE',  ( 36.72346799070689372, -287.3215950561159957, -291.2391520109006819 ) ) ;
#23707 = CARTESIAN_POINT ( 'NONE',  ( 196.1963538710215857, 305.7026273589066250, -40.00000000000000711 ) ) ;
#23708 = CARTESIAN_POINT ( 'NONE',  ( -91.34056130169399523, -282.2365002186331253, -320.6658236015437069 ) ) ;
#23709 = CARTESIAN_POINT ( 'NONE',  ( -76.50052936066884968, -291.4424939987589482, -333.4281582862054734 ) ) ;
#23710 = CARTESIAN_POINT ( 'NONE',  ( -75.05849261621393964, -284.0196463547703729, -207.0511557583419631 ) ) ;
#23711 = CARTESIAN_POINT ( 'NONE',  ( -5.358919178937607164, -281.7972513551345628, -204.1920526839323315 ) ) ;
#23712 = CARTESIAN_POINT ( 'NONE',  ( 27.25331354631952863, -289.0402782859607669, -311.9357054173046322 ) ) ;
#23713 = CARTESIAN_POINT ( 'NONE',  ( -99.22388079738097133, -278.5074608347254070, -309.2961039327813069 ) ) ;
#23714 = CARTESIAN_POINT ( 'NONE',  ( 23.66834049785471805, -291.7263794272370205, -224.0169230836491465 ) ) ;
#23715 = CARTESIAN_POINT ( 'NONE',  ( -36.57732853976609277, -286.8643449668857670, -193.5133842317157473 ) ) ;
#23716 = CARTESIAN_POINT ( 'NONE',  ( 37.96198084474539769, -287.8462400112704245, -254.5213404396648968 ) ) ;
#23717 = CARTESIAN_POINT ( 'NONE',  ( -95.92047378970561056, -284.1078156761905120, -313.9217341492939113 ) ) ;
#23718 = EDGE_LOOP ( 'NONE', ( #79138, #28168, #36998, #1237 ) ) ;
#23719 = CYLINDRICAL_SURFACE ( 'NONE', #83644, 1.000000000000000888 ) ;
#23720 = CARTESIAN_POINT ( 'NONE',  ( 34.27711181027408571, -295.0940647306704250, -245.4830056167927523 ) ) ;
#23721 = CARTESIAN_POINT ( 'NONE',  ( 39.21813982612355431, -292.2365499623663823, -270.3270031064367345 ) ) ;
#23722 = CARTESIAN_POINT ( 'NONE',  ( 3.254608541759664408, -275.5504116477532079, -331.3147739031238075 ) ) ;
#23723 = CARTESIAN_POINT ( 'NONE',  ( -99.83386833973021623, -296.4953568145294867, -225.5499397012155214 ) ) ;
#23724 = CARTESIAN_POINT ( 'NONE',  ( 30.11703625713074572, -292.4273791275849135, -300.0263608761631531 ) ) ;
#23725 = CARTESIAN_POINT ( 'NONE',  ( -95.23005910177541011, -295.4344117431912196, -224.2426627599575966 ) ) ;
#23726 = CARTESIAN_POINT ( 'NONE',  ( -91.97895070757937219, -292.4549808932696351, -221.3331180906272380 ) ) ;
#23727 = CARTESIAN_POINT ( 'NONE',  ( 23.19599393104245166, -295.2057403767670962, -311.7949675016975561 ) ) ;
#23728 = DIRECTION ( 'NONE',  ( -0.000000000000000000, 0.000000000000000000, -1.000000000000000000 ) ) ;
#23729 = CARTESIAN_POINT ( 'NONE',  ( -61.03834599168131092, -293.3587371776023360, -341.7492416118952292 ) ) ;
#23730 = CARTESIAN_POINT ( 'NONE',  ( -111.4051325982030676, -298.3995686644375951, -282.2571981095354090 ) ) ;
#23731 = CARTESIAN_POINT ( 'NONE',  ( -0.8638712076543580975, -289.4966536073875432, -333.9236406160345609 ) ) ;
#23732 = CARTESIAN_POINT ( 'NONE',  ( 32.66575191105214060, -277.8950840933381983, -298.3831569637608254 ) ) ;
#23733 = CARTESIAN_POINT ( 'NONE',  ( -96.42582866246149820, -277.8943071983611048, -221.7365944833149740 ) ) ;
#23734 = CARTESIAN_POINT ( 'NONE',  ( -5.149371496979327389, -273.8134592347573175, -200.5258348918962952 ) ) ;
#23735 = CARTESIAN_POINT ( 'NONE',  ( 37.12854104167171698, -279.6088583577912914, -268.5729121899955203 ) ) ;
#23736 = CARTESIAN_POINT ( 'NONE',  ( 0.6305054117470390018, -274.9550107430797539, -336.4857164793249922 ) ) ;
#23737 = ADVANCED_FACE ( 'NONE', ( #18731, #41416, #47592, #55191, #68451 ), #17796, .T. ) ;
#23738 = CARTESIAN_POINT ( 'NONE',  ( -94.33554197619169202, -294.5844211212437358, -316.7807452265661823 ) ) ;
#23739 = CARTESIAN_POINT ( 'NONE',  ( 206.0205385567603571, 30.15663536185482485, 14.00000000000000000 ) ) ;
#23740 = CARTESIAN_POINT ( 'NONE',  ( -6.493500732843245693, -275.1197641780397021, -204.0868298866615760 ) ) ;
#23741 = CARTESIAN_POINT ( 'NONE',  ( 208.4306832106270804, -324.2391364535881735, 0.000000000000000000 ) ) ;
#23742 = CARTESIAN_POINT ( 'NONE',  ( -100.9272138103576282, -288.0295444183770428, -310.8958990310553645 ) ) ;
#23743 = CARTESIAN_POINT ( 'NONE',  ( -112.8679962522325866, -290.3638129636675558, -285.4205680058415169 ) ) ;
#23744 = CARTESIAN_POINT ( 'NONE',  ( 6.761243456491912163, -300.5815312243726680, -194.9911137133431964 ) ) ;
#23745 = CARTESIAN_POINT ( 'NONE',  ( -110.9499677108039037, -294.3775424395805089, -283.9174618738385334 ) ) ;
#23746 = CARTESIAN_POINT ( 'NONE',  ( 6.823820858814699797, -281.6655426567394329, -333.3035610497407788 ) ) ;
#23747 = DIRECTION ( 'NONE',  ( 1.000000000000000000, 0.000000000000000000, 0.000000000000000000 ) ) ;
#23748 = CARTESIAN_POINT ( 'NONE',  ( 26.02162632492521155, -280.0928590006643617, -310.5826702957890575 ) ) ;
#23749 = DIRECTION ( 'NONE',  ( 0.000000000000000000, 0.000000000000000000, 1.000000000000000000 ) ) ;
#23750 = CARTESIAN_POINT ( 'NONE',  ( -62.92483046979299388, -290.5063902385302299, -201.5669761773716573 ) ) ;
#23751 = CARTESIAN_POINT ( 'NONE',  ( -92.60007452029728370, -281.9939301119690640, -319.9521959839975125 ) ) ;
#23752 = CARTESIAN_POINT ( 'NONE',  ( 200.1126601882106968, 275.5000000000000568, -2.416251949619912409 ) ) ;
#23753 = CARTESIAN_POINT ( 'NONE',  ( -23.68628624284178130, -44.55766379199612004, 21.50000000000000000 ) ) ;
#23754 = CARTESIAN_POINT ( 'NONE',  ( 36.69218430280204757, -291.3968879084102923, -258.2812851779880816 ) ) ;
#23755 = CARTESIAN_POINT ( 'NONE',  ( -32.34627376723635450, -278.5883910844883076, -344.0423731885952634 ) ) ;
#23756 = CARTESIAN_POINT ( 'NONE',  ( -65.09395149291948712, -284.6118741767489269, -341.7742756927728465 ) ) ;
#23757 = CARTESIAN_POINT ( 'NONE',  ( -5.694686395241257415, -272.5449236736599801, -201.7478486865377079 ) ) ;
#23758 = CARTESIAN_POINT ( 'NONE',  ( 33.08553933276996872, -277.2582394440208304, -291.7444443146456479 ) ) ;
#23759 = CARTESIAN_POINT ( 'NONE',  ( 25.51952530406399688, -276.8684533413307918, -307.7919617326492698 ) ) ;
#23760 = CARTESIAN_POINT ( 'NONE',  ( -106.1029658601182604, -286.9457713872822069, -240.2830571392789523 ) ) ;
#23761 = ADVANCED_FACE ( 'NONE', ( #61373 ), #56031, .T. ) ;
#23762 = ORIENTED_EDGE ( 'NONE', *, *, #89138, .F. ) ;
#23763 = CARTESIAN_POINT ( 'NONE',  ( -111.0908949349528712, -270.9825380859393249, -270.3411330354564370 ) ) ;
#23764 = CARTESIAN_POINT ( 'NONE',  ( -53.29131893547408083, -295.0844389604874323, -345.7456665325554468 ) ) ;
#23765 = CARTESIAN_POINT ( 'NONE',  ( -24.89175949740537064, -288.1914903908325982, -196.7094422370003315 ) ) ;
#23766 = CARTESIAN_POINT ( 'NONE',  ( 195.5540042012145818, 26.59710438755789141, 14.87405783778811852 ) ) ;
#23767 = CARTESIAN_POINT ( 'NONE',  ( -111.2869819898779866, -293.6237833571632905, -305.9350535429201159 ) ) ;
#23768 = CARTESIAN_POINT ( 'NONE',  ( -101.6245809791751640, -278.0250773646622520, -228.4415664899898388 ) ) ;
#23769 = CARTESIAN_POINT ( 'NONE',  ( 8.387283476604746824, -291.0659102710815773, -209.3419860969198396 ) ) ;
#23770 = CARTESIAN_POINT ( 'NONE',  ( -107.1956738927552095, -286.3830719421417825, -246.7250458566439875 ) ) ;
#23771 = CARTESIAN_POINT ( 'NONE',  ( -52.05036797764275036, -281.6216019020221211, -197.7715789073788528 ) ) ;
#23772 = CARTESIAN_POINT ( 'NONE',  ( -10.22021151092482683, -287.8244532225228909, -198.8692541545776464 ) ) ;
#23773 = CARTESIAN_POINT ( 'NONE',  ( -34.75266722667074504, -285.0198105566751678, -345.3291987317878124 ) ) ;
#23774 = CARTESIAN_POINT ( 'NONE',  ( 31.85621553845096443, -276.1538370432323859, -304.2560587003409296 ) ) ;
#23775 = CARTESIAN_POINT ( 'NONE',  ( -85.10845996581620909, -295.4095287780866101, -212.9335309116574138 ) ) ;
#23776 = CARTESIAN_POINT ( 'NONE',  ( -100.2477601903501920, -278.9730484463010498, -225.9558523943842658 ) ) ;
#23777 = CARTESIAN_POINT ( 'NONE',  ( -111.2307951829731678, -298.3500433393001003, -279.8124643945582193 ) ) ;
#23778 = CARTESIAN_POINT ( 'NONE',  ( 156.4851178187871312, 14.99999999999999645, 10.00000000000000178 ) ) ;
#23779 = EDGE_CURVE ( 'NONE', #37492, #79467, #400, .T. ) ;
#23780 = CARTESIAN_POINT ( 'NONE',  ( -85.33152481854864391, -275.9090924074130839, -210.2361428286349110 ) ) ;
#23781 = CARTESIAN_POINT ( 'NONE',  ( -26.40771704191215008, -296.3272358670997733, -194.5997318284844084 ) ) ;
#23782 = CARTESIAN_POINT ( 'NONE',  ( 180.7149167944524493, -12.49482340714361506, 10.00000000000000000 ) ) ;
#23783 = CARTESIAN_POINT ( 'NONE',  ( -110.4125176284502885, -278.0922414299042202, -267.8999406243838166 ) ) ;
#23784 = CARTESIAN_POINT ( 'NONE',  ( -13.20223463151127063, -275.5639970889189385, -197.6610841212505534 ) ) ;
#23785 = CARTESIAN_POINT ( 'NONE',  ( 22.33276463728777728, -281.2606203925236628, -318.6703453541426825 ) ) ;
#23786 = CARTESIAN_POINT ( 'NONE',  ( -12.93283279051736301, -290.4906883977004668, -340.2337249750351020 ) ) ;
#23787 = CARTESIAN_POINT ( 'NONE',  ( -34.80774276975866854, -299.6034472235986641, -194.0538049768059921 ) ) ;
#23788 = CARTESIAN_POINT ( 'NONE',  ( -95.28089541048503008, -298.4382944112228415, -220.1714697068004511 ) ) ;
#23789 = CARTESIAN_POINT ( 'NONE',  ( -69.83615561411666306, -293.6234967448971815, -202.9367386652224070 ) ) ;
#23790 = CARTESIAN_POINT ( 'NONE',  ( 36.50880623550769855, -279.7075511326453352, -282.4495892469234377 ) ) ;
#23791 = CARTESIAN_POINT ( 'NONE',  ( -4.953634996015651382, -282.4021334475221465, -203.3362909475473828 ) ) ;
#23792 = CARTESIAN_POINT ( 'NONE',  ( -93.82132065097373186, -295.3091709421734095, -221.8506269889319640 ) ) ;
#23793 = CARTESIAN_POINT ( 'NONE',  ( -95.22238364596634597, -286.8286742636647659, -220.7212164923518856 ) ) ;
#23794 = CARTESIAN_POINT ( 'NONE',  ( -74.88597072180587588, -288.4850991617178124, -333.3413654865399280 ) ) ;
#23795 = CARTESIAN_POINT ( 'NONE',  ( -98.37663915457927999, -248.8749983746587588, -334.1288200131682515 ) ) ;
#23796 = EDGE_LOOP ( 'NONE', ( #2617, #58758, #77226, #53153, #79683 ) ) ;
#23797 = CARTESIAN_POINT ( 'NONE',  ( -59.87099359773471008, -287.9132215709267939, -343.3750702615831756 ) ) ;
#23798 = CARTESIAN_POINT ( 'NONE',  ( 26.38790659474636868, -286.7301904746042283, -234.6118299107389475 ) ) ;
#23799 = VERTEX_POINT ( 'NONE', #69855 ) ;
#23800 = CARTESIAN_POINT ( 'NONE',  ( -83.68542741185271439, -284.7507385847470118, -331.5322490186136406 ) ) ;
#23801 = CARTESIAN_POINT ( 'NONE',  ( 29.17527318117884150, -276.2913504179543338, -300.4871822534802845 ) ) ;
#23802 = EDGE_CURVE ( 'NONE', #40445, #93104, #27936, .T. ) ;
#23803 = CARTESIAN_POINT ( 'NONE',  ( -76.99760560997145831, -290.4547072366088400, -204.6576534808791621 ) ) ;
#23804 = CARTESIAN_POINT ( 'NONE',  ( -10.72951485012345074, -283.3655723005207392, -342.5641011175051176 ) ) ;
#23805 = CARTESIAN_POINT ( 'NONE',  ( 36.52555394281589685, -283.3139965145331303, -289.5010377970299942 ) ) ;
#23806 = CARTESIAN_POINT ( 'NONE',  ( -31.63362043503224186, -283.3152623811682247, -347.1413160497097010 ) ) ;
#23807 = CARTESIAN_POINT ( 'NONE',  ( 0.3999504757506849861, -280.5698389978297769, -207.8160622513621547 ) ) ;
#23808 = CARTESIAN_POINT ( 'NONE',  ( -53.28691492658257545, -295.3380690714490129, -200.3538533559491555 ) ) ;
#23809 = CARTESIAN_POINT ( 'NONE',  ( -112.0640318895732719, -271.7261958592908400, -296.4135090774117316 ) ) ;
#23810 = EDGE_LOOP ( 'NONE', ( #67824, #53642, #34446, #61347 ) ) ;
#23811 = CARTESIAN_POINT ( 'NONE',  ( 35.61557228249901641, -277.3373698464109793, -253.6526428978296792 ) ) ;
#23812 = CARTESIAN_POINT ( 'NONE',  ( 179.1553158749216266, 254.2886184646079357, -166.4193513437393790 ) ) ;
#23813 = CARTESIAN_POINT ( 'NONE',  ( -41.86637595129381140, -297.3422149966701227, -197.3993473282040725 ) ) ;
#23814 = CARTESIAN_POINT ( 'NONE',  ( 15.40054671173733247, -292.2810732461673524, -214.2720501491700702 ) ) ;
#23815 = CARTESIAN_POINT ( 'NONE',  ( 201.7602898703672736, 289.7935802246685171, -82.39453363523685425 ) ) ;
#23817 = CARTESIAN_POINT ( 'NONE',  ( -23.65659818303267059, -287.2743562672910116, -342.9334358167427013 ) ) ;
#23816 = CARTESIAN_POINT ( 'NONE',  ( -35.82431374170981542, -296.6455330352716828, -193.9507017958873973 ) ) ;
#23818 = CARTESIAN_POINT ( 'NONE',  ( -71.47805722691788333, -297.3683545409638214, -336.2963095267152767 ) ) ;
#23819 = CARTESIAN_POINT ( 'NONE',  ( -73.81482698521389807, -286.8722041519692425, -206.5424903439755724 ) ) ;
#23820 = EDGE_LOOP ( 'NONE', ( #33566, #39244, #7536, #76828 ) ) ;
#23821 = CARTESIAN_POINT ( 'NONE',  ( -94.46843459369449647, -296.7953301135331117, -321.6579492710721979 ) ) ;
#23822 = CARTESIAN_POINT ( 'NONE',  ( -101.0480484625467597, -285.5347574658555914, -234.4874666514279227 ) ) ;
#23823 = CARTESIAN_POINT ( 'NONE',  ( -14.93901213210802581, -297.1216951677442921, -193.7626547343421919 ) ) ;
#23824 = CARTESIAN_POINT ( 'NONE',  ( -53.36564568420788390, -292.6546361128370108, -195.1576014967284038 ) ) ;
#23825 = CARTESIAN_POINT ( 'NONE',  ( 20.32840346640906759, -293.3541058025260782, -219.4129714714107422 ) ) ;
#23826 = CARTESIAN_POINT ( 'NONE',  ( -94.10294619750740708, -290.0695529661919636, -316.2649407992306010 ) ) ;
#23827 = ORIENTED_EDGE ( 'NONE', *, *, #42791, .T. ) ;
#23828 = DIRECTION ( 'NONE',  ( -0.000000000000000000, -0.000000000000000000, -1.000000000000000000 ) ) ;
#23829 = CARTESIAN_POINT ( 'NONE',  ( 51.75226373859299400, -301.0166613338370780, -194.5684141701167107 ) ) ;
#23830 = CARTESIAN_POINT ( 'NONE',  ( 36.85032307720787514, -274.5869354967246636, -289.4281684230728047 ) ) ;
#23831 = ORIENTED_EDGE ( 'NONE', *, *, #87216, .F. ) ;
#23832 = CARTESIAN_POINT ( 'NONE',  ( 26.01264011972551415, -275.6376536612108907, -314.1082674476651846 ) ) ;
#23833 = CARTESIAN_POINT ( 'NONE',  ( -41.89199681228512873, -296.4736465157424732, -196.8083984324122753 ) ) ;
#23834 = CARTESIAN_POINT ( 'NONE',  ( -108.8138658240379186, -280.6739260031801564, -250.2491787424162055 ) ) ;
#23835 = CARTESIAN_POINT ( 'NONE',  ( 14.57858332972057092, -274.4520077790725168, -323.4906689658292862 ) ) ;
#23836 = CARTESIAN_POINT ( 'NONE',  ( -109.6697496110946730, -297.9209907192684454, -257.8797813783895663 ) ) ;
#23837 = CARTESIAN_POINT ( 'NONE',  ( -34.04203350448968735, -275.0359254128838415, -197.2001950198926181 ) ) ;
#23838 = CARTESIAN_POINT ( 'NONE',  ( -112.8581325102493338, -274.4192598553474340, -261.9205935356417854 ) ) ;
#23839 = CARTESIAN_POINT ( 'NONE',  ( -5.779709832144479087, -272.4851952159589246, -201.9341673327492970 ) ) ;
#23840 = CARTESIAN_POINT ( 'NONE',  ( 16.23949007678421808, -294.9173058159784091, -320.0898694699145608 ) ) ;
#23841 = CARTESIAN_POINT ( 'NONE',  ( -72.89583931315375764, -290.1464168377394230, -205.8734492928335840 ) ) ;
#23842 = CARTESIAN_POINT ( 'NONE',  ( 41.08708295871279859, -296.0521521680024080, -465.6442049081569508 ) ) ;
#23843 = CARTESIAN_POINT ( 'NONE',  ( -91.28141809152558039, -278.2864630770181975, -325.2994934917702494 ) ) ;
#23844 = CARTESIAN_POINT ( 'NONE',  ( 35.10635481474194819, -275.8423480909079331, -279.7242288040310427 ) ) ;
#23845 = CARTESIAN_POINT ( 'NONE',  ( 186.6539576904058890, 276.0000000000000568, 11.60392986742922616 ) ) ;
#23846 = CARTESIAN_POINT ( 'NONE',  ( -64.35728263601791355, -284.3916973768498906, -198.7687176775378362 ) ) ;
#23847 = CARTESIAN_POINT ( 'NONE',  ( -47.36136915731026420, -297.1793749862714549, -344.8569880512051213 ) ) ;
#23848 = CARTESIAN_POINT ( 'NONE',  ( 184.7149167944524493, -12.49482340714361506, -3.999999999999998224 ) ) ;
#23849 = CARTESIAN_POINT ( 'NONE',  ( -83.74240713423068883, -284.5937038152087553, -213.7305055269242757 ) ) ;
#23850 = CARTESIAN_POINT ( 'NONE',  ( -24.86361577729069339, -280.8933118845253034, -344.5376624190648727 ) ) ;
#23851 = CARTESIAN_POINT ( 'NONE',  ( -46.04925959493782983, -275.4037982373302498, -343.9117833643645099 ) ) ;
#23852 = CARTESIAN_POINT ( 'NONE',  ( 35.60698321438832181, -274.0000920151603623, -260.6727478587579299 ) ) ;
#23853 = CARTESIAN_POINT ( 'NONE',  ( -7.896232487481309903, -282.4379590160257862, -201.3285514889731758 ) ) ;
#23854 = CARTESIAN_POINT ( 'NONE',  ( 32.48062166773370052, -277.0557994643210122, -292.9879578831901767 ) ) ;
#23855 = DIRECTION ( 'NONE',  ( -1.000000000000000000, -0.000000000000000000, -0.000000000000000000 ) ) ;
#23856 = CARTESIAN_POINT ( 'NONE',  ( -13.29542512518735364, -272.7592449605619436, -198.0547069756708822 ) ) ;
#23857 = CARTESIAN_POINT ( 'NONE',  ( 11.77451335985401748, -282.7326330422181968, -213.4609774177922645 ) ) ;
#23858 = CARTESIAN_POINT ( 'NONE',  ( 41.08708295871279859, -296.0521521680024080, -507.6442049081570076 ) ) ;
#23859 = CARTESIAN_POINT ( 'NONE',  ( -13.18761188330635825, -288.2836691543280381, -198.7657674517327280 ) ) ;
#23860 = CARTESIAN_POINT ( 'NONE',  ( 154.3564990690631191, 19.12150670424431098, -10.40578999957124040 ) ) ;
#23861 = CARTESIAN_POINT ( 'NONE',  ( -112.3706766292436896, -288.5754777742207580, -268.5316172249676470 ) ) ;
#23862 = DIRECTION ( 'NONE',  ( 0.9167375550253848981, 0.000000000000000000, 0.3994899938747897283 ) ) ;
#23863 = CARTESIAN_POINT ( 'NONE',  ( -110.2005776581172967, -295.2253174345212869, -279.6409053897473314 ) ) ;
#23864 = CARTESIAN_POINT ( 'NONE',  ( -106.2686032546539394, -288.3273018208026315, -298.0663386365166616 ) ) ;
#23865 = CARTESIAN_POINT ( 'NONE',  ( 85.37101130053461873, 80.99577858023421584, -298.5812782549759845 ) ) ;
#23866 = LINE ( 'NONE', #58477, #42917 ) ;
#23867 = CARTESIAN_POINT ( 'NONE',  ( 30.81131567701246610, -285.5864111041672686, -236.0409462525921924 ) ) ;
#23868 = CARTESIAN_POINT ( 'NONE',  ( 8.304588364289221758, -284.0160764638553132, -328.4165410077273464 ) ) ;
#23869 = CARTESIAN_POINT ( 'NONE',  ( -103.5453083600116742, -282.3003944884046632, -307.7646101432980572 ) ) ;
#23870 = CARTESIAN_POINT ( 'NONE',  ( -79.53070514208576469, -291.4646717474291222, -210.7249372514021388 ) ) ;
#23871 = CARTESIAN_POINT ( 'NONE',  ( 27.38184324191901098, -283.4513769997220720, -305.3787970786149231 ) ) ;
#23872 = CARTESIAN_POINT ( 'NONE',  ( 5.695310469968751121, -283.2547879006495464, -329.5254437648013663 ) ) ;
#23873 = CARTESIAN_POINT ( 'NONE',  ( -6.280930527751023895, -290.6260054003775508, -339.0170383244702066 ) ) ;
#23874 = CARTESIAN_POINT ( 'NONE',  ( -36.18651701771133133, -298.2329201614146541, -193.3610862879390311 ) ) ;
#23875 = CARTESIAN_POINT ( 'NONE',  ( -31.95432840838165234, -287.0646614741164626, -345.7803928787717496 ) ) ;
#23876 = CARTESIAN_POINT ( 'NONE',  ( 39.38050151352002359, -275.6338790170673860, -276.8959305480021840 ) ) ;
#23877 = CARTESIAN_POINT ( 'NONE',  ( -27.92325412946086161, -294.1520733013399536, -196.2610019592440835 ) ) ;
#23878 = CARTESIAN_POINT ( 'NONE',  ( 180.2288731078812702, 249.5000000000000568, -24.90909090909092782 ) ) ;
#23879 = CARTESIAN_POINT ( 'NONE',  ( -85.28047601435908120, -286.1948066931273615, -330.5268031993605859 ) ) ;
#23880 = CARTESIAN_POINT ( 'NONE',  ( -45.47712670929725221, -275.1547142858140091, -345.1380317294898532 ) ) ;
#23881 = LINE ( 'NONE', #71898, #17095 ) ;
#23882 = CARTESIAN_POINT ( 'NONE',  ( -101.6304058046137442, -295.4938606898023750, -229.4538724497002988 ) ) ;
#23883 = CARTESIAN_POINT ( 'NONE',  ( -66.90303124352954001, -293.2582770051119496, -202.7403510586119069 ) ) ;
#23884 = CARTESIAN_POINT ( 'NONE',  ( 15.52623723758388863, -274.1728276660218739, -219.8014603362215666 ) ) ;
#23885 = CARTESIAN_POINT ( 'NONE',  ( -110.3067230472953781, -291.9360447949975992, -280.7865290769095736 ) ) ;
#23886 = CARTESIAN_POINT ( 'NONE',  ( -28.08846191411517879, -293.1136004314858496, -197.6618340841534121 ) ) ;
#23887 = CARTESIAN_POINT ( 'NONE',  ( -104.4131198845685446, -286.7305219381780717, -238.9442005070774542 ) ) ;
#23888 = CARTESIAN_POINT ( 'NONE',  ( -11.37072441228891861, -293.8091242230677267, -198.4437398750833665 ) ) ;
#23889 = CARTESIAN_POINT ( 'NONE',  ( 6.201724264528955644, -293.9450042304076760, -207.4542943158702997 ) ) ;
#23890 = CARTESIAN_POINT ( 'NONE',  ( -7.990256111431073727, -294.4899406038641700, -337.2140004973140321 ) ) ;
#23891 = CARTESIAN_POINT ( 'NONE',  ( 2.392167251682307594, -290.5198157390677807, -333.9710262581976394 ) ) ;
#23892 = CARTESIAN_POINT ( 'NONE',  ( 24.25637975933156198, -282.3337561422110298, -316.5636780708224478 ) ) ;
#23893 = CARTESIAN_POINT ( 'NONE',  ( -84.30199401848265950, -295.4915915241630842, -211.1661435939996920 ) ) ;
#23894 = CARTESIAN_POINT ( 'NONE',  ( -67.18710026026457172, -285.5048218637452351, -199.3804720608231946 ) ) ;
#23895 = CARTESIAN_POINT ( 'NONE',  ( 10.74240339485621476, -278.3634436810751822, -327.4554766186412280 ) ) ;
#23896 = CARTESIAN_POINT ( 'NONE',  ( -62.68565492269070916, -284.5098659060736850, -201.4243077839427656 ) ) ;
#23897 = CARTESIAN_POINT ( 'NONE',  ( 30.90303789707364501, -285.1423027157269985, -239.1288291535903170 ) ) ;
#23898 = CARTESIAN_POINT ( 'NONE',  ( -17.29563249692224147, -278.4477748599451843, -197.2963477405119477 ) ) ;
#23899 = DIRECTION ( 'NONE',  ( 0.000000000000000000, -1.000000000000000000, 0.000000000000000000 ) ) ;
#23900 = CARTESIAN_POINT ( 'NONE',  ( -84.90658679699598110, -283.2370646750198375, -325.8189397721372416 ) ) ;
#23901 = CARTESIAN_POINT ( 'NONE',  ( -72.33916100788187009, -280.8045948323829748, -202.2056101964543302 ) ) ;
#23902 = CARTESIAN_POINT ( 'NONE',  ( 25.35986498400079370, -286.0228087338464888, -226.0514999871602697 ) ) ;
#23903 = CARTESIAN_POINT ( 'NONE',  ( -15.26955331896128598, -296.5227243923497440, -341.0605870371815627 ) ) ;
#23904 = CARTESIAN_POINT ( 'NONE',  ( -99.79799510027925180, -279.5691221042563370, -314.0148879717900741 ) ) ;
#23905 = CARTESIAN_POINT ( 'NONE',  ( -92.96387463440578358, -279.1447027761931849, -322.9677960686437928 ) ) ;
#23906 = CARTESIAN_POINT ( 'NONE',  ( -64.33511580822029430, -277.2476619686501067, -338.2407217379158055 ) ) ;
#23907 = CARTESIAN_POINT ( 'NONE',  ( -40.62323327122707894, -300.0109735787196428, -195.5869007918923330 ) ) ;
#23908 = CARTESIAN_POINT ( 'NONE',  ( 20.08462882394540117, -284.8874804685262916, -222.3594286362373680 ) ) ;
#23909 = CARTESIAN_POINT ( 'NONE',  ( -110.7656065109321872, -291.8942514084221784, -290.7417555607279382 ) ) ;
#23910 = CARTESIAN_POINT ( 'NONE',  ( 24.68147399423603972, -293.0112072294700170, -309.5377965601114170 ) ) ;
#23911 = ORIENTED_EDGE ( 'NONE', *, *, #33481, .F. ) ;
#23912 = CARTESIAN_POINT ( 'NONE',  ( 20.53736924031489863, -293.8454898468997953, -314.9023798082772601 ) ) ;
#23913 = ORIENTED_EDGE ( 'NONE', *, *, #87263, .T. ) ;
#23914 = CARTESIAN_POINT ( 'NONE',  ( -73.30099428914419946, -292.6663771704143642, -202.6083873396415242 ) ) ;
#23915 = CARTESIAN_POINT ( 'NONE',  ( -27.55292716731614178, -280.8310658396268309, -197.8662740700175391 ) ) ;
#23916 = ADVANCED_FACE ( 'NONE', ( #19656 ), #48525, .T. ) ;
#23917 = CARTESIAN_POINT ( 'NONE',  ( -75.61367048977638206, -296.4746835240489986, -203.8415520073582456 ) ) ;
#23918 = CARTESIAN_POINT ( 'NONE',  ( 22.00620840721034099, -287.5456827016009811, -221.4618486675311431 ) ) ;
#23919 = CARTESIAN_POINT ( 'NONE',  ( 30.34612202740482445, -288.3610802007995630, -307.1346199572772662 ) ) ;
#23921 = CARTESIAN_POINT ( 'NONE',  ( -95.13057066695022002, -284.2569086975846062, -315.0193357681693556 ) ) ;
#23920 = AXIS2_PLACEMENT_3D ( 'NONE', #54514, #41220, #25632 ) ;
#23922 = CARTESIAN_POINT ( 'NONE',  ( 173.6393091186583035, 243.4999469645294425, -179.6212980618050210 ) ) ;
#23923 = CARTESIAN_POINT ( 'NONE',  ( -114.0692606672204477, -271.5444964837377029, -270.3482881119212493 ) ) ;
#23924 = CARTESIAN_POINT ( 'NONE',  ( -77.20900537737810509, -207.8186285356463259, -353.4261111359479060 ) ) ;
#23925 = CARTESIAN_POINT ( 'NONE',  ( -27.00879002244773375, -276.1145696363147408, -342.7892388707338114 ) ) ;
#23926 = CARTESIAN_POINT ( 'NONE',  ( -95.52671526393385193, -276.8477418197925886, -314.9562980829682601 ) ) ;
#23927 = CARTESIAN_POINT ( 'NONE',  ( -73.93107113370481898, -273.2468667334241559, -202.5747474471526175 ) ) ;
#23928 = CARTESIAN_POINT ( 'NONE',  ( -109.1284923609438238, -270.2178699211290791, -295.6185954890034964 ) ) ;
#23929 = CARTESIAN_POINT ( 'NONE',  ( -94.85123006512304755, -276.5498030080088938, -320.8185479603513954 ) ) ;
#23930 = CARTESIAN_POINT ( 'NONE',  ( -73.57003431435376228, -290.0391701915085605, -333.8223395237987461 ) ) ;
#23931 = CARTESIAN_POINT ( 'NONE',  ( -9.194102113407405241, -299.1989826547440998, -193.5188644571881582 ) ) ;
#23932 = CARTESIAN_POINT ( 'NONE',  ( -109.0745196346259007, -273.5566487964402427, -242.5068259347219168 ) ) ;
#23933 = CARTESIAN_POINT ( 'NONE',  ( -109.7365167224504177, -296.8476136959104679, -260.5988440050695090 ) ) ;
#23934 = EDGE_LOOP ( 'NONE', ( #17060, #22485, #26611, #77860, #537, #76910 ) ) ;
#23935 = CARTESIAN_POINT ( 'NONE',  ( 196.5477508190182903, 71.74599609987329529, -11.11079997048496892 ) ) ;
#23936 = CARTESIAN_POINT ( 'NONE',  ( -90.30196549952719920, -279.7140398929894332, -324.3280051383205773 ) ) ;
#23937 = CARTESIAN_POINT ( 'NONE',  ( 19.73364297326644490, -281.7616661695618063, -322.0329710821996514 ) ) ;
#23938 = CARTESIAN_POINT ( 'NONE',  ( -87.29616588362910079, -278.8482891705223778, -324.0153575546233355 ) ) ;
#23939 = CARTESIAN_POINT ( 'NONE',  ( -108.6629507555766736, -280.6497591483076235, -243.9935703873790658 ) ) ;
#23940 = CARTESIAN_POINT ( 'NONE',  ( 95.76662123053866083, -298.3250659313402480, -196.8050307037779021 ) ) ;
#23941 = FACE_OUTER_BOUND ( 'NONE', #78985, .T. ) ;
#23942 = CARTESIAN_POINT ( 'NONE',  ( -6.771356966445523540, -280.6316374636527371, -204.0567934928062073 ) ) ;
#23943 = CARTESIAN_POINT ( 'NONE',  ( 8.153700883368010466, -277.2507147900504378, -332.3489450671041254 ) ) ;
#23944 = CARTESIAN_POINT ( 'NONE',  ( 34.58291505140212507, -277.8266213278472492, -291.6632550308056011 ) ) ;
#23945 = CARTESIAN_POINT ( 'NONE',  ( 37.91497188685495701, -273.9592025254017926, -257.0560006027221789 ) ) ;
#23946 = ORIENTED_EDGE ( 'NONE', *, *, #54972, .T. ) ;
#23947 = DIRECTION ( 'NONE',  ( 0.000000000000000000, 1.000000000000000000, 0.000000000000000000 ) ) ;
#23948 = CARTESIAN_POINT ( 'NONE',  ( -103.6984915610428288, -290.1643219826851805, -239.5491404876763113 ) ) ;
#23949 = CARTESIAN_POINT ( 'NONE',  ( 0.2412273258851620195, -285.8876288778715775, -203.2578166836876221 ) ) ;
#23950 = CARTESIAN_POINT ( 'NONE',  ( -33.46526014224244960, -281.2425783014975309, -344.2856181345452455 ) ) ;
#23951 = CARTESIAN_POINT ( 'NONE',  ( 16.24255596435040161, -280.8479255910486359, -320.8737105092341722 ) ) ;
#23952 = CARTESIAN_POINT ( 'NONE',  ( -95.81995174611536470, -291.9060327787839810, -317.3417518730313418 ) ) ;
#23953 = CARTESIAN_POINT ( 'NONE',  ( -9.108713640866275441, -281.6348572780157156, -202.6113653671510804 ) ) ;
#23954 = CARTESIAN_POINT ( 'NONE',  ( -82.35875606868249577, -271.4379707664899115, -210.3089252440176722 ) ) ;
#23955 = CARTESIAN_POINT ( 'NONE',  ( -2.023218349699846375, -280.9922334229024727, -337.8818204526351110 ) ) ;
#23956 = CARTESIAN_POINT ( 'NONE',  ( 3.169018264107629435, -296.5085695028729447, -333.5402786762712140 ) ) ;
#23957 = CARTESIAN_POINT ( 'NONE',  ( -102.5305802070660803, -277.3091000817353802, -231.2154991483648985 ) ) ;
#23958 = CARTESIAN_POINT ( 'NONE',  ( -74.05730758487722198, -278.2053778895952405, -333.5739081229071985 ) ) ;
#23959 = CARTESIAN_POINT ( 'NONE',  ( -112.0782437926158082, -286.4494415202189543, -278.3909041774814455 ) ) ;
#23960 = EDGE_CURVE ( 'NONE', #23364, #35701, #5475, .T. ) ;
#23961 = EDGE_CURVE ( 'NONE', #81433, #74457, #24900, .T. ) ;
#23962 = CARTESIAN_POINT ( 'NONE',  ( 208.4306832106271656, 1.063508326895939327, -7.500000000000014211 ) ) ;
#23963 = CARTESIAN_POINT ( 'NONE',  ( -107.0482918840414612, -292.8502531109541565, -241.2011237905825283 ) ) ;
#23964 = CARTESIAN_POINT ( 'NONE',  ( 29.81017751619885559, -273.9942016173828279, -303.8791028315648646 ) ) ;
#23965 = CARTESIAN_POINT ( 'NONE',  ( -48.85491922567549494, -288.3922638284930144, -346.3860276065843777 ) ) ;
#23966 = CARTESIAN_POINT ( 'NONE',  ( -11.96620081880925035, -290.7877398135687486, -201.0063951513710663 ) ) ;
#23967 = CARTESIAN_POINT ( 'NONE',  ( -43.38476897654369679, -264.5837039706560745, -435.9172296759396659 ) ) ;
#23968 = CARTESIAN_POINT ( 'NONE',  ( -107.5929501375299253, -276.9509359331373730, -292.1188166171854732 ) ) ;
#23969 = CARTESIAN_POINT ( 'NONE',  ( -111.3324369047018649, -294.6057818723013497, -276.9867039834608704 ) ) ;
#23970 = CARTESIAN_POINT ( 'NONE',  ( -94.47717563777250405, -291.2178609897763977, -316.5864456496148591 ) ) ;
#23971 = SURFACE_SIDE_STYLE ('',( #59037 ) ) ;
#23972 = DIRECTION ( 'NONE',  ( 0.000000000000000000, 0.000000000000000000, 1.000000000000000000 ) ) ;
#23973 = CARTESIAN_POINT ( 'NONE',  ( 31.59526911869172494, -292.4565297260984948, -303.2012257864039384 ) ) ;
#23974 = CARTESIAN_POINT ( 'NONE',  ( 36.35015695339029662, -289.0890404907353854, -265.5140760727286420 ) ) ;
#23975 = CARTESIAN_POINT ( 'NONE',  ( -106.8141325011825984, -288.3924901878856986, -301.2730027581621925 ) ) ;
#23976 = CARTESIAN_POINT ( 'NONE',  ( -44.09638606840582042, -287.3903494591515937, -197.0825458423149144 ) ) ;
#23977 = CARTESIAN_POINT ( 'NONE',  ( 195.0811277904324754, 39.36132622696000283, 15.19607843137254477 ) ) ;
#23978 = CARTESIAN_POINT ( 'NONE',  ( 31.55489321480201781, -288.6819924654222405, -294.9753649245494671 ) ) ;
#23979 = CARTESIAN_POINT ( 'NONE',  ( -71.30955064076870542, -297.4783258995264532, -337.6262050490568072 ) ) ;
#23980 = DIRECTION ( 'NONE',  ( 0.000000000000000000, 0.000000000000000000, 1.000000000000000000 ) ) ;
#23981 = CIRCLE ( 'NONE', #70846, 2.500000000000009326 ) ;
#23982 = CARTESIAN_POINT ( 'NONE',  ( 38.95768582296182103, -288.6644383284276500, -262.9801780157574740 ) ) ;
#23983 = CARTESIAN_POINT ( 'NONE',  ( -31.18250303832461157, -278.1495677559947239, -195.2064831246659367 ) ) ;
#23984 = CARTESIAN_POINT ( 'NONE',  ( -34.28768442688075879, -277.3480157702554152, -347.2793686106254540 ) ) ;
#23985 = CARTESIAN_POINT ( 'NONE',  ( -16.99349426536716834, -279.9746637911981111, -196.1203285901392519 ) ) ;
#23986 = CARTESIAN_POINT ( 'NONE',  ( -95.75385141253924814, -299.1738394472778282, -223.8867445098934468 ) ) ;
#23987 = CARTESIAN_POINT ( 'NONE',  ( -94.77055790362604171, -283.2188027989268448, -222.1228868096299038 ) ) ;
#23988 = LINE ( 'NONE', #68957, #91232 ) ;
#23989 = CARTESIAN_POINT ( 'NONE',  ( -2.549558956960578548, -278.6569489036358505, -204.7694736121925416 ) ) ;
#23990 = CARTESIAN_POINT ( 'NONE',  ( -106.3959287420960322, -282.1680181412125421, -299.7603465414932202 ) ) ;
#23991 = SPHERICAL_SURFACE ( 'NONE', #48710, 2.000000000000000000 ) ;
#23992 = CARTESIAN_POINT ( 'NONE',  ( -39.95873918027843530, -275.5643242329203417, -346.6358447972009458 ) ) ;
#23993 = CARTESIAN_POINT ( 'NONE',  ( -104.5611745072759931, -297.6677642711055114, -300.6892603022994876 ) ) ;
#23994 = CARTESIAN_POINT ( 'NONE',  ( -63.81825088255502010, -282.3097839389124033, -342.3367025211248347 ) ) ;
#23995 = CARTESIAN_POINT ( 'NONE',  ( -97.08159317062981586, -298.0830161059922716, -227.9989458506799451 ) ) ;
#23996 = CARTESIAN_POINT ( 'NONE',  ( -113.5943785400798731, -274.0489174888291473, -264.6882063956397246 ) ) ;
#23997 = CARTESIAN_POINT ( 'NONE',  ( -8.958693874168883298, -274.1004872762172795, -203.0279766285698599 ) ) ;
#23998 = CARTESIAN_POINT ( 'NONE',  ( 37.19753870975527832, -295.6647713107479944, -279.1194778449742557 ) ) ;
#23999 = CARTESIAN_POINT ( 'NONE',  ( 21.49039423764156354, -288.3880808071408524, -320.0379201850865911 ) ) ;
#24000 = CARTESIAN_POINT ( 'NONE',  ( -102.1634311530903432, -277.1491130150744198, -231.4334491674557341 ) ) ;
#24001 = CARTESIAN_POINT ( 'NONE',  ( -114.3901496886219746, -290.3746479219313983, -271.2266388070503353 ) ) ;
#24002 = CARTESIAN_POINT ( 'NONE',  ( -104.2676010946641441, -289.2103627284244567, -300.2241264792394873 ) ) ;
#24003 = CARTESIAN_POINT ( 'NONE',  ( 36.10856825881999299, -291.3564332654094073, -255.1303845328275486 ) ) ;
#24004 = EDGE_LOOP ( 'NONE', ( #34502, #19347, #84806, #52128 ) ) ;
#24005 = CARTESIAN_POINT ( 'NONE',  ( 28.92138380700103895, -24.05900251067409457, -347.7894294321414463 ) ) ;
#24006 = CARTESIAN_POINT ( 'NONE',  ( -102.4615737567793872, -290.5106841674224256, -237.1222601914937229 ) ) ;
#24007 = DIRECTION ( 'NONE',  ( 0.000000000000000000, 0.000000000000000000, 1.000000000000000000 ) ) ;
#24008 = CARTESIAN_POINT ( 'NONE',  ( -105.2296266693531237, -285.9587564480613082, -234.4136310133014263 ) ) ;
#24009 = CARTESIAN_POINT ( 'NONE',  ( 13.13280560600884073, -291.7964315240021733, -212.5238939548889334 ) ) ;
#24010 = CARTESIAN_POINT ( 'NONE',  ( 23.87067568443297816, -283.4820644124300770, -316.2560340571390611 ) ) ;
#24011 = CARTESIAN_POINT ( 'NONE',  ( -103.0135927354892402, -283.9525244412004099, -302.3551481932249203 ) ) ;
#24012 = CARTESIAN_POINT ( 'NONE',  ( -68.17745805382324420, -297.6584023455129682, -199.7482714480778725 ) ) ;
#24013 = CARTESIAN_POINT ( 'NONE',  ( 11.86436072089016136, -276.0677416204142105, -215.7031678710926599 ) ) ;
#24014 = CARTESIAN_POINT ( 'NONE',  ( -5.313529187195955572, -290.4957845859748886, -202.9226721014413783 ) ) ;
#24015 = CARTESIAN_POINT ( 'NONE',  ( 19.31509798575756420, -273.6894139809560329, -223.7013094366977555 ) ) ;
#24016 = ORIENTED_EDGE ( 'NONE', *, *, #45671, .F. ) ;
#24017 = DIRECTION ( 'NONE',  ( -0.000000000000000000, -1.000000000000000000, -0.000000000000000000 ) ) ;
#24018 = CARTESIAN_POINT ( 'NONE',  ( -16.79747137322971184, -288.2395862551080086, -198.7583066653558603 ) ) ;
#24019 = CARTESIAN_POINT ( 'NONE',  ( -114.0290016266300626, -297.6411369145560570, -269.6192974228089270 ) ) ;
#24020 = CARTESIAN_POINT ( 'NONE',  ( -109.0305551328621902, -285.3919961689906586, -256.0572465978581818 ) ) ;
#24021 = CARTESIAN_POINT ( 'NONE',  ( -113.8457029045860480, -277.5238828230081367, -277.2978523315670714 ) ) ;
#24022 = CARTESIAN_POINT ( 'NONE',  ( 37.66004072891103505, -293.9903543095188638, -253.3300238259291177 ) ) ;
#24023 = CARTESIAN_POINT ( 'NONE',  ( 24.82441493895079532, -286.2744659137090935, -313.7602766908942158 ) ) ;
#24024 = CARTESIAN_POINT ( 'NONE',  ( 39.48135836021926082, -293.9563912595863258, -276.0333594785666378 ) ) ;
#24025 = CARTESIAN_POINT ( 'NONE',  ( -36.21005868477442391, -292.3999731901431574, -197.3362630471475256 ) ) ;
#24026 = DIRECTION ( 'NONE',  ( 1.000000000000000000, 0.000000000000000000, 0.000000000000000000 ) ) ;
#24027 = CARTESIAN_POINT ( 'NONE',  ( 153.6987871352711181, 19.48326534539917887, -11.45812909362560639 ) ) ;
#24028 = CARTESIAN_POINT ( 'NONE',  ( -97.39219751933890734, -246.9239084015181902, -331.4851807666239552 ) ) ;
#24029 = CARTESIAN_POINT ( 'NONE',  ( -113.5148738872261163, -286.0050369231415175, -275.6888339762146529 ) ) ;
#24030 = CARTESIAN_POINT ( 'NONE',  ( -106.6379572354042296, -294.4809262143061233, -236.9535640164627353 ) ) ;
#24031 = ORIENTED_EDGE ( 'NONE', *, *, #13958, .T. ) ;
#24032 = CARTESIAN_POINT ( 'NONE',  ( -53.77226634314865095, -282.1881939430227817, -341.8575472872119008 ) ) ;
#24033 = CARTESIAN_POINT ( 'NONE',  ( -98.55696196329681413, -278.8414789833790906, -223.6659283124894841 ) ) ;
#24034 = CARTESIAN_POINT ( 'NONE',  ( 29.40538630022882671, -283.1027979550383975, -236.4105907008620306 ) ) ;
#24035 = CARTESIAN_POINT ( 'NONE',  ( -109.7673734041845250, -271.5244187881392577, -296.0454323531374712 ) ) ;
#24036 = CARTESIAN_POINT ( 'NONE',  ( -74.00930885969619055, -282.1038073525274399, -337.4581557811464450 ) ) ;
#24037 = CARTESIAN_POINT ( 'NONE',  ( 36.13644118953845918, -285.7418516898928260, -283.5068227219726964 ) ) ;
#24038 = CARTESIAN_POINT ( 'NONE',  ( -78.19576668289161603, -275.3693793909611713, -206.5547646540406959 ) ) ;
#24039 = CARTESIAN_POINT ( 'NONE',  ( -69.74572868557065419, -295.9831485914014024, -335.8436910468028032 ) ) ;
#24040 = VERTEX_POINT ( 'NONE', #6879 ) ;
#24041 = CARTESIAN_POINT ( 'NONE',  ( 13.25471663912096432, -291.4626902602138330, -217.0577776790478595 ) ) ;
#24042 = CARTESIAN_POINT ( 'NONE',  ( -102.0067704589574902, -278.6557295953940070, -312.0724651775327629 ) ) ;
#24043 = CARTESIAN_POINT ( 'NONE',  ( 5.396786294105012871, -276.4557763541437225, -329.6048022234635937 ) ) ;
#24044 = CARTESIAN_POINT ( 'NONE',  ( -78.68652459779990238, -274.5887606757104891, -205.7693383287437996 ) ) ;
#24045 = CARTESIAN_POINT ( 'NONE',  ( -103.3467885130483381, -276.9605693250397849, -309.5142434987732827 ) ) ;
#24046 = CARTESIAN_POINT ( 'NONE',  ( 160.7988830095787876, 220.5294184113604103, -205.1624142897960041 ) ) ;
#24047 = CARTESIAN_POINT ( 'NONE',  ( -83.93836615091302633, -275.6916119227558397, -329.1952503178288225 ) ) ;
#24048 = CARTESIAN_POINT ( 'NONE',  ( 30.38850688036680125, -295.4372827684630920, -305.7337818621584802 ) ) ;
#24049 = DIRECTION ( 'NONE',  ( -0.000000000000000000, -0.000000000000000000, 1.000000000000000000 ) ) ;
#24050 = VECTOR ( 'NONE', #12462, 1000.000000000000000 ) ;
#24051 = DIRECTION ( 'NONE',  ( 0.000000000000000000, 0.000000000000000000, 1.000000000000000000 ) ) ;
#24052 = CARTESIAN_POINT ( 'NONE',  ( -108.3314206663945072, -285.8723084710375133, -252.0667021042178817 ) ) ;
#24053 = CARTESIAN_POINT ( 'NONE',  ( -35.89570210073392786, -284.7944193386777556, -346.3469723819573005 ) ) ;
#24054 = CARTESIAN_POINT ( 'NONE',  ( 9.101633486965683417, -286.0582559666873976, -213.9083994426079585 ) ) ;
#24055 = CARTESIAN_POINT ( 'NONE',  ( 26.05247062488065524, -274.4658794630133229, -308.1449707306840651 ) ) ;
#24056 = CARTESIAN_POINT ( 'NONE',  ( -21.09519838463042163, -284.7020652081021694, -342.8496178439958726 ) ) ;
#24057 = CARTESIAN_POINT ( 'NONE',  ( -96.95528110235694896, -277.6326687465584655, -227.0375826116616906 ) ) ;
#24058 = CARTESIAN_POINT ( 'NONE',  ( -8.604888092625166962, -277.7466936344683290, -337.8167068637942521 ) ) ;
#24059 = CARTESIAN_POINT ( 'NONE',  ( 150.6539576904058606, 293.9636489450775230, 0.000000000000000000 ) ) ;
#24060 = CARTESIAN_POINT ( 'NONE',  ( -29.98990376932585633, -274.6400607751372149, -197.6704065268607735 ) ) ;
#24061 = CARTESIAN_POINT ( 'NONE',  ( 24.45577590054008965, -281.7468264399373084, -224.6967907960918751 ) ) ;
#24062 = CARTESIAN_POINT ( 'NONE',  ( 31.96330624505919360, -281.6141370065750493, -236.8268511722395715 ) ) ;
#24063 = ORIENTED_EDGE ( 'NONE', *, *, #83965, .F. ) ;
#24064 = ORIENTED_EDGE ( 'NONE', *, *, #46511, .T. ) ;
#24065 = CARTESIAN_POINT ( 'NONE',  ( 197.0984808611934795, 19.93437704977705494, -12.12215979493057638 ) ) ;
#24066 = CARTESIAN_POINT ( 'NONE',  ( 6.804669258927659392, -288.5056494202891599, -208.7221413189987516 ) ) ;
#24067 = CARTESIAN_POINT ( 'NONE',  ( -90.15536508354232126, -296.4790531619310059, -219.6594025006754407 ) ) ;
#24068 = CARTESIAN_POINT ( 'NONE',  ( -90.70921547136478580, -290.6682294340274098, -214.9227848401430094 ) ) ;
#24069 = CARTESIAN_POINT ( 'NONE',  ( 34.68423810131464791, -286.2364437076421382, -286.0077860441973598 ) ) ;
#24070 = CARTESIAN_POINT ( 'NONE',  ( -58.87877431507047277, -287.9108690292268875, -340.7814571186216881 ) ) ;
#24071 = CARTESIAN_POINT ( 'NONE',  ( -33.23168645308187052, -287.3099947028100587, -197.0291167287993517 ) ) ;
#24072 = CARTESIAN_POINT ( 'NONE',  ( -108.7699542241383739, -276.2548504244458627, -293.3978189630082625 ) ) ;
#24073 = CARTESIAN_POINT ( 'NONE',  ( -38.92420283273519743, -287.4715737141797263, -346.5446864407430780 ) ) ;
#24074 = CARTESIAN_POINT ( 'NONE',  ( -51.81299776773756349, -287.8672905748318271, -196.7174977352765097 ) ) ;
#24075 = CARTESIAN_POINT ( 'NONE',  ( -62.18240498515375947, -287.3741381022549604, -341.3595797603300070 ) ) ;
#24076 = CARTESIAN_POINT ( 'NONE',  ( 31.58009454605360844, -282.8239079437940404, -295.2738956358620612 ) ) ;
#24077 = CARTESIAN_POINT ( 'NONE',  ( -63.76868395764510922, -293.7087111566713133, -199.9383623610897587 ) ) ;
#24078 = DIRECTION ( 'NONE',  ( 0.000000000000000000, 1.000000000000000000, 0.000000000000000000 ) ) ;
#24079 = EDGE_CURVE ( 'NONE', #68325, #35152, #12497, .T. ) ;
#24080 = DIRECTION ( 'NONE',  ( 0.000000000000000000, 0.000000000000000000, -1.000000000000000000 ) ) ;
#24081 = CARTESIAN_POINT ( 'NONE',  ( -101.1143957367595902, -299.0135756114960373, -229.8351079163101076 ) ) ;
#24082 = CARTESIAN_POINT ( 'NONE',  ( 9.387514357973238077, -279.9105285566134853, -214.0013558451431663 ) ) ;
#24083 = CARTESIAN_POINT ( 'NONE',  ( 32.95352943092358089, -279.2108490648196835, -244.0665967520644415 ) ) ;
#24084 = CARTESIAN_POINT ( 'NONE',  ( 27.96328084532138902, -293.2811028027144857, -310.9507902760603315 ) ) ;
#24085 = CARTESIAN_POINT ( 'NONE',  ( -111.3550334602798841, -270.7922941965885570, -270.3387588715830248 ) ) ;
#24086 = CARTESIAN_POINT ( 'NONE',  ( 37.08310203119101089, -273.6125308602656219, -268.8567847437584533 ) ) ;
#24087 = CARTESIAN_POINT ( 'NONE',  ( -93.44810510923574043, -297.1969993751604306, -317.8497011250556170 ) ) ;
#24088 = CARTESIAN_POINT ( 'NONE',  ( -109.5391439510883345, -271.4447933644419777, -245.3384203335399150 ) ) ;
#24089 = CARTESIAN_POINT ( 'NONE',  ( -71.63701261007109622, -293.7388975568979959, -338.1682382464410352 ) ) ;
#24090 = CARTESIAN_POINT ( 'NONE',  ( 15.28429262419472501, -294.2384285814295026, -218.8500356984787345 ) ) ;
#24091 = CARTESIAN_POINT ( 'NONE',  ( 179.1465552314772083, 8.542400036368780647, -9.000000000000001776 ) ) ;
#24092 = CARTESIAN_POINT ( 'NONE',  ( 16.85092222879885071, -293.6515628917910021, -221.1364317592264968 ) ) ;
#24093 = DIRECTION ( 'NONE',  ( 0.5335274993778010844, -0.8457827187922856149, 0.000000000000000000 ) ) ;
#24095 = CARTESIAN_POINT ( 'NONE',  ( -63.56899361707755958, -295.4036097707765975, -338.5405087687711330 ) ) ;
#24094 = CARTESIAN_POINT ( 'NONE',  ( -111.3773302825175335, -282.7551080707198707, -256.0497324981460565 ) ) ;
#24096 = CARTESIAN_POINT ( 'NONE',  ( 23.40291776680545155, -282.1845285084945658, -317.7014633831005312 ) ) ;
#24097 = CARTESIAN_POINT ( 'NONE',  ( 37.97436862015810277, -283.3949895945349340, -264.2944892374715664 ) ) ;
#24098 = CARTESIAN_POINT ( 'NONE',  ( -30.88139700416046907, -285.7983820696040311, -193.6405339634017650 ) ) ;
#24099 = CARTESIAN_POINT ( 'NONE',  ( -92.08334897910739869, -289.2679089808933668, -219.3188481302005641 ) ) ;
#24100 = CARTESIAN_POINT ( 'NONE',  ( 37.98031237521716008, -280.1872657929903312, -282.6615398329582263 ) ) ;
#24101 = CARTESIAN_POINT ( 'NONE',  ( 15.39495156249690488, -285.5019081419919758, -219.1743125896222466 ) ) ;
#24102 = CARTESIAN_POINT ( 'NONE',  ( -3.210702582081981227, -287.5323454636259726, -339.0529575108198514 ) ) ;
#24103 = DIRECTION ( 'NONE',  ( -0.000000000000000000, -1.000000000000000000, -0.000000000000000000 ) ) ;
#24104 = CARTESIAN_POINT ( 'NONE',  ( -20.64761206647024849, -296.4345130589201176, -342.3008465266025269 ) ) ;
#24105 = CARTESIAN_POINT ( 'NONE',  ( -102.9153380359032894, -280.4940004957827000, -231.0318765051935088 ) ) ;
#24107 = CARTESIAN_POINT ( 'NONE',  ( -41.04801483223821634, -279.6709406116780201, -197.4340947460692348 ) ) ;
#24106 = CARTESIAN_POINT ( 'NONE',  ( -41.87242274252311347, -293.1289512496367706, -345.6312679145259494 ) ) ;
#24108 = CARTESIAN_POINT ( 'NONE',  ( 39.22589159581952600, -293.6108102615382904, -261.7238101312024696 ) ) ;
#24109 = CARTESIAN_POINT ( 'NONE',  ( -49.09613425688456090, -283.9834865030073843, -195.6682691328664134 ) ) ;
#24110 = CARTESIAN_POINT ( 'NONE',  ( -104.5417644539270299, -280.1114965846896894, -303.7818189914986533 ) ) ;
#24112 = CARTESIAN_POINT ( 'NONE',  ( -71.04973375405431568, -294.5671396668164448, -335.3918917136205664 ) ) ;
#24111 = CIRCLE ( 'NONE', #89112, 1.000000000000000888 ) ;
#24113 = CARTESIAN_POINT ( 'NONE',  ( -37.57518916095028061, -296.0490714493265045, -195.3614770738068387 ) ) ;
#24114 = ORIENTED_EDGE ( 'NONE', *, *, #33104, .F. ) ;
#24115 = DIRECTION ( 'NONE',  ( -0.000000000000000000, -1.000000000000000000, -0.000000000000000000 ) ) ;
#24116 = CARTESIAN_POINT ( 'NONE',  ( 23.94941473222153761, -284.1127613472592657, -312.9668223289573916 ) ) ;
#24117 = CARTESIAN_POINT ( 'NONE',  ( -88.54944952712649808, -295.3015085682924337, -322.5451279973512442 ) ) ;
#24118 = CARTESIAN_POINT ( 'NONE',  ( 10.41963433625062230, -229.5268262511776527, 22.50000000000000000 ) ) ;
#24119 = TOROIDAL_SURFACE ( 'NONE', #80094, 24.00000000000002132, 2.046895004029262388 ) ;
#24120 = CARTESIAN_POINT ( 'NONE',  ( 35.78497577281001440, -278.8380690714489560, -253.7030783399848985 ) ) ;
#24121 = CARTESIAN_POINT ( 'NONE',  ( -34.09975461072447445, -273.2891254431398238, -193.5910156633567567 ) ) ;
#24122 = CARTESIAN_POINT ( 'NONE',  ( -8.404038286393724633, -289.9963363167768193, -341.1983837932966139 ) ) ;
#24123 = CARTESIAN_POINT ( 'NONE',  ( -90.59421059806915366, -289.6662681520369347, -320.3665941199759573 ) ) ;
#24124 = CARTESIAN_POINT ( 'NONE',  ( -8.998403965952357808, -281.9498526219713881, -202.3363775124014410 ) ) ;
#24125 = CARTESIAN_POINT ( 'NONE',  ( -102.7488135132294644, -274.6137010119094839, -236.0692410952486568 ) ) ;
#24126 = CARTESIAN_POINT ( 'NONE',  ( -57.20601436142635521, -278.5849814165087537, -199.7032130898164439 ) ) ;
#24127 = ORIENTED_EDGE ( 'NONE', *, *, #6444, .F. ) ;
#24128 = CARTESIAN_POINT ( 'NONE',  ( -101.2073588118438323, -272.9532307374003608, -227.2525068493970082 ) ) ;
#24129 = CARTESIAN_POINT ( 'NONE',  ( 3.000762344979050589, -294.5181086247619646, -207.7396978107178711 ) ) ;
#24130 = FACE_BOUND ( 'NONE', #61458, .T. ) ;
#24131 = CARTESIAN_POINT ( 'NONE',  ( -108.5286334908166737, -291.4232610434195294, -253.6838318876198457 ) ) ;
#24132 = DIRECTION ( 'NONE',  ( -1.000000000000000000, -0.000000000000000000, -0.000000000000000000 ) ) ;
#24133 = CARTESIAN_POINT ( 'NONE',  ( -58.56953896801237391, -289.9201061846744665, -197.6309018657443914 ) ) ;
#24134 = CARTESIAN_POINT ( 'NONE',  ( -70.47334986065760631, -297.2695722315889952, -205.2750790525290654 ) ) ;
#24135 = LINE ( 'NONE', #8072, #15278 ) ;
#24136 = CARTESIAN_POINT ( 'NONE',  ( -98.65911243411574105, -292.6817630445017926, -224.9202536514419819 ) ) ;
#24137 = CARTESIAN_POINT ( 'NONE',  ( -119.3990491898856732, -299.0519495502701943, -270.3937649182068412 ) ) ;
#24138 = CARTESIAN_POINT ( 'NONE',  ( 37.09547970612607060, -289.4533585897438002, -262.6712100871828852 ) ) ;
#24139 = CARTESIAN_POINT ( 'NONE',  ( 19.68949475164547280, -274.2240834885686240, -318.8118273691307536 ) ) ;
#24140 = CARTESIAN_POINT ( 'NONE',  ( 3.703958444967716535, -276.5289197830974217, -208.1982527677516828 ) ) ;
#24141 = CARTESIAN_POINT ( 'NONE',  ( 17.82142236992688922, -290.9290158271220434, -220.3020482852665509 ) ) ;
#24142 = CARTESIAN_POINT ( 'NONE',  ( -71.96384143193522220, -281.4598290435216654, -202.9552106530227604 ) ) ;
#24143 = ORIENTED_EDGE ( 'NONE', *, *, #22580, .T. ) ;
#24144 = CARTESIAN_POINT ( 'NONE',  ( 33.05537322495047903, -281.1607716488837241, -290.0625070634780514 ) ) ;
#24145 = CARTESIAN_POINT ( 'NONE',  ( -54.05045401314183806, -278.3413657381316852, -345.2641178048867800 ) ) ;
#24146 = CARTESIAN_POINT ( 'NONE',  ( -3.084253864379969734, -281.4046670687133656, -338.8916495060582292 ) ) ;
#24147 = CARTESIAN_POINT ( 'NONE',  ( -64.99907447057177023, -278.3458907325305063, -342.0265140400529731 ) ) ;
#24148 = CARTESIAN_POINT ( 'NONE',  ( 0.000000000000000000, 0.000000000000000000, 0.000000000000000000 ) ) ;
#24149 = CARTESIAN_POINT ( 'NONE',  ( -52.42766400724116238, -275.3825835483822289, -195.5066199320201008 ) ) ;
#24150 = CARTESIAN_POINT ( 'NONE',  ( -82.08285599513421005, -280.1948066931273615, -326.5171145203363494 ) ) ;
#24151 = ORIENTED_EDGE ( 'NONE', *, *, #39969, .F. ) ;
#24152 = ORIENTED_EDGE ( 'NONE', *, *, #49321, .T. ) ;
#24153 = CARTESIAN_POINT ( 'NONE',  ( -111.1046351201329969, -298.3772169364756905, -283.9979007281625627 ) ) ;
#24154 = CARTESIAN_POINT ( 'NONE',  ( -37.25390324154415111, -290.1307009779644659, -343.6701785853040860 ) ) ;
#24155 = CARTESIAN_POINT ( 'NONE',  ( 5.011349368260566095, -290.2482910822479312, -333.4498904414700746 ) ) ;
#24156 = CARTESIAN_POINT ( 'NONE',  ( -32.14176661739875840, -291.4680244683075330, -197.4317236692579343 ) ) ;
#24157 = CARTESIAN_POINT ( 'NONE',  ( 38.61320028161129159, -287.2173468159307959, -282.9478121757559279 ) ) ;
#24158 = CARTESIAN_POINT ( 'NONE',  ( 152.5990036449066736, 20.65770287760360446, -10.64853154254647549 ) ) ;
#24159 = CARTESIAN_POINT ( 'NONE',  ( -101.1024427810556148, -282.4475416280000104, -307.5230354533509285 ) ) ;
#24160 = CARTESIAN_POINT ( 'NONE',  ( -111.5719011644520862, -292.4013956106432488, -271.2229367236711823 ) ) ;
#24161 = CARTESIAN_POINT ( 'NONE',  ( -94.64910958572320965, -283.6813277305129191, -224.0100495101620481 ) ) ;
#24162 = CARTESIAN_POINT ( 'NONE',  ( -19.43047097031776715, -281.6024504666851840, -199.0313334681027300 ) ) ;
#24163 = CARTESIAN_POINT ( 'NONE',  ( -3.154718925215548531, -289.5529418247576814, -339.1075769570591092 ) ) ;
#24164 = CARTESIAN_POINT ( 'NONE',  ( -109.6836514192032155, -279.1839540675258036, -259.7809594759498282 ) ) ;
#24165 = CARTESIAN_POINT ( 'NONE',  ( -73.23401242778071207, -290.3819992879446659, -202.6724414925973292 ) ) ;
#24166 = CARTESIAN_POINT ( 'NONE',  ( 5.081986803286600463, -287.4124233823784493, -206.2322390820201292 ) ) ;
#24167 = CARTESIAN_POINT ( 'NONE',  ( -97.53617769424801054, -285.6865395604866080, -222.4429400733428963 ) ) ;
#24168 = CARTESIAN_POINT ( 'NONE',  ( -69.00724396369996327, -283.6472497812994789, -336.1494852067335728 ) ) ;
#24169 = EDGE_LOOP ( 'NONE', ( #6253, #499, #39864, #87621 ) ) ;
#24170 = CARTESIAN_POINT ( 'NONE',  ( 207.2825244649536955, 35.50712927932389107, 14.50000000000000178 ) ) ;
#24171 = CARTESIAN_POINT ( 'NONE',  ( -19.69779548106202682, -294.1369444681128584, -196.6254443763347979 ) ) ;
#24172 = CARTESIAN_POINT ( 'NONE',  ( 39.16350184510627486, -292.2006147227178872, -267.4720409403039980 ) ) ;
#24173 = CARTESIAN_POINT ( 'NONE',  ( -41.88311313187436014, -276.1694909777545490, -343.4681050640111266 ) ) ;
#24174 = EDGE_CURVE ( 'NONE', #72125, #40992, #93033, .T. ) ;
#24175 = CARTESIAN_POINT ( 'NONE',  ( -60.10998323911704233, -297.1133091972114357, -196.8555655907056803 ) ) ;
#24176 = AXIS2_PLACEMENT_3D ( 'NONE', #42155, #55924, #42630 ) ;
#24177 = CARTESIAN_POINT ( 'NONE',  ( 32.46398070410751302, -291.7192834577892881, -246.5827713165533339 ) ) ;
#24178 = CARTESIAN_POINT ( 'NONE',  ( -78.05088637139978403, -295.7369702212350830, -208.4874396830663272 ) ) ;
#24179 = CARTESIAN_POINT ( 'NONE',  ( -92.86688826628117965, -292.4374696092740464, -222.3602431167188911 ) ) ;
#24180 = CARTESIAN_POINT ( 'NONE',  ( 22.04708407315842322, -294.0328264091616575, -227.3607306866663293 ) ) ;
#24181 = CARTESIAN_POINT ( 'NONE',  ( 191.4749582765727212, 14.19731191252289015, 13.00000000000000178 ) ) ;
#24182 = CARTESIAN_POINT ( 'NONE',  ( 16.23645552972213224, -292.2941826334723601, -323.1552297913313510 ) ) ;
#24183 = TOROIDAL_SURFACE ( 'NONE', #55965, 24.16304133878946558, 4.003189038634632269 ) ;
#24184 = CARTESIAN_POINT ( 'NONE',  ( -112.3201108662026400, -298.5947487997715939, -267.0564237451849294 ) ) ;
#24185 = CARTESIAN_POINT ( 'NONE',  ( 35.91539534603148809, -288.4662274997117493, -268.2938975531151300 ) ) ;
#24186 = CARTESIAN_POINT ( 'NONE',  ( 21.37558129910982174, -278.1790031429999317, -317.6116938469855882 ) ) ;
#24187 = CARTESIAN_POINT ( 'NONE',  ( -88.95595053112002404, -276.5535686918682359, -326.9648093196621517 ) ) ;
#24188 = CARTESIAN_POINT ( 'NONE',  ( -38.34774694635147796, -273.3884413390801456, -193.4696317380877133 ) ) ;
#24189 = CARTESIAN_POINT ( 'NONE',  ( 34.85812525177245647, -279.3968261568018647, -252.1847070104660702 ) ) ;
#24190 = CARTESIAN_POINT ( 'NONE',  ( -38.55289252647968112, -275.4669799786212252, -346.5514942191414889 ) ) ;
#24191 = EDGE_CURVE ( 'NONE', #63777, #72522, #17016, .T. ) ;
#24192 = CARTESIAN_POINT ( 'NONE',  ( -82.67709312739731331, -294.3711659101185205, -328.2701625731981494 ) ) ;
#24193 = CARTESIAN_POINT ( 'NONE',  ( -75.83866562722688798, -275.5387618305366573, -205.9355391194186780 ) ) ;
#24194 = CARTESIAN_POINT ( 'NONE',  ( -34.48223376678599550, -298.8916831039321664, -197.1992380068014370 ) ) ;
#24195 = DIRECTION ( 'NONE',  ( -0.000000000000000000, -0.000000000000000000, -1.000000000000000000 ) ) ;
#24197 = CARTESIAN_POINT ( 'NONE',  ( 31.11905179698761259, -275.0475697052659712, -245.0209236197029554 ) ) ;
#24196 = CARTESIAN_POINT ( 'NONE',  ( -94.23343959948523718, -287.8898220745959406, -319.7750510876022076 ) ) ;
#24198 = CARTESIAN_POINT ( 'NONE',  ( 38.67497842921257245, -287.7096145223900407, -282.9516801271768713 ) ) ;
#24199 = CARTESIAN_POINT ( 'NONE',  ( -108.3778075964839189, -274.8696739443033721, -245.7867439049370546 ) ) ;
#24200 = CARTESIAN_POINT ( 'NONE',  ( -83.51042277272051706, -293.6862896706013544, -329.3209835028397379 ) ) ;
#24201 = CARTESIAN_POINT ( 'NONE',  ( -83.79373517715774256, -282.8685375476570698, -331.6355378381636001 ) ) ;
#24202 = CARTESIAN_POINT ( 'NONE',  ( 113.5000000000000568, -192.7866584945343504, -447.4016117689005796 ) ) ;
#24203 = CARTESIAN_POINT ( 'NONE',  ( 35.74198568589435610, -279.3350511499395452, -253.4595420684386795 ) ) ;
#24204 = CARTESIAN_POINT ( 'NONE',  ( 189.4188515237862589, 293.9636489450775798, -9.103929867429222611 ) ) ;
#24205 = CARTESIAN_POINT ( 'NONE',  ( -100.6541973942827042, -288.8388165928553803, -307.5915418789282967 ) ) ;
#24206 = CARTESIAN_POINT ( 'NONE',  ( -100.0875395593015469, -282.1515326856607544, -310.1288638457169782 ) ) ;
#24207 = DIRECTION ( 'NONE',  ( 0.000000000000000000, 0.000000000000000000, 1.000000000000000000 ) ) ;
#24208 = ADVANCED_FACE ( 'NONE', ( #56126 ), #84979, .T. ) ;
#24209 = SURFACE_STYLE_USAGE ( .BOTH. , #2457 ) ;
#24210 = CARTESIAN_POINT ( 'NONE',  ( -111.6068545495161146, -288.4163302950433376, -280.9266537294239470 ) ) ;
#24211 = CARTESIAN_POINT ( 'NONE',  ( -74.64086251223216095, -275.0666614153669229, -206.7450917909235102 ) ) ;
#24212 = CARTESIAN_POINT ( 'NONE',  ( -30.23636762041420312, -284.1692178395238102, -346.6338062024674400 ) ) ;
#24214 = CARTESIAN_POINT ( 'NONE',  ( -73.79679229502430360, -283.5503328884254870, -333.6644825090182849 ) ) ;
#24213 = CARTESIAN_POINT ( 'NONE',  ( -64.36186634220776170, -271.7821386223063200, -199.7835771281365567 ) ) ;
#24215 = CARTESIAN_POINT ( 'NONE',  ( 35.20348540882881849, -276.8148124321920136, -257.9344166695875629 ) ) ;
#24216 = CARTESIAN_POINT ( 'NONE',  ( 28.17966191647327889, -276.7967436675832573, -303.0261309458548453 ) ) ;
#24217 = CARTESIAN_POINT ( 'NONE',  ( 1.091704864048238521, -284.5392268195603265, -334.7651087697895491 ) ) ;
#24218 = ORIENTED_EDGE ( 'NONE', *, *, #20150, .F. ) ;
#24219 = DIRECTION ( 'NONE',  ( 0.9999189529070979798, -0.01273136352371030157, 0.000000000000000000 ) ) ;
#24220 = CARTESIAN_POINT ( 'NONE',  ( -114.3662701192796902, -296.3591270630996064, -272.4676747528282021 ) ) ;
#24221 = CARTESIAN_POINT ( 'NONE',  ( 30.28981536891485504, -289.1148842548566336, -238.7727512765025608 ) ) ;
#24222 = DIRECTION ( 'NONE',  ( 0.6023974895724104606, -0.000000000000000000, 0.7981962569173435273 ) ) ;
#24223 = CARTESIAN_POINT ( 'NONE',  ( 44.71564893372296723, -291.0523547857347353, -270.3937649182068412 ) ) ;
#24224 = CARTESIAN_POINT ( 'NONE',  ( -50.87153719638330784, -278.8034896274349421, -194.8731320652599948 ) ) ;
#24225 = CARTESIAN_POINT ( 'NONE',  ( -40.57783604249069498, -290.4120001036104668, -194.2168185693909379 ) ) ;
#24226 = CARTESIAN_POINT ( 'NONE',  ( -109.3464679038811340, -286.2780121446183443, -254.6170723644917757 ) ) ;
#24227 = CARTESIAN_POINT ( 'NONE',  ( -54.75261396379869439, -281.5855864304346596, -198.3718723131606794 ) ) ;
#24228 = CARTESIAN_POINT ( 'NONE',  ( -104.9195258151892887, -286.4426988563691339, -234.5848582629495525 ) ) ;
#24229 = CARTESIAN_POINT ( 'NONE',  ( 19.12703919101086569, -284.2377290810115369, -319.7198267435823027 ) ) ;
#24230 = CARTESIAN_POINT ( 'NONE',  ( 35.20168651080174982, -276.0464200419949066, -296.3341210845319438 ) ) ;
#24231 = CARTESIAN_POINT ( 'NONE',  ( -109.7065170970319627, -270.7998507873303424, -251.1006153585047969 ) ) ;
#24232 = CARTESIAN_POINT ( 'NONE',  ( -108.5118480687430065, -278.7590219587250431, -240.9704724198646204 ) ) ;
#24233 = CARTESIAN_POINT ( 'NONE',  ( -89.14507455184212859, -299.2372652091091823, -216.8314382558901343 ) ) ;
#24234 = CARTESIAN_POINT ( 'NONE',  ( 196.0143093133015384, 20.19615242270663913, 11.99999999999998757 ) ) ;
#24235 = CARTESIAN_POINT ( 'NONE',  ( -54.49178911615187815, -282.3376638359844719, -195.3683826091709363 ) ) ;
#24236 = AXIS2_PLACEMENT_3D ( 'NONE', #84201, #54854, #83736 ) ;
#24237 = CARTESIAN_POINT ( 'NONE',  ( -54.29536025777959907, -295.9762185724656547, -196.5175069794742342 ) ) ;
#24238 = CARTESIAN_POINT ( 'NONE',  ( 219.8344101925596021, 35.72494958537217968, -7.000000000000000000 ) ) ;
#24239 = B_SPLINE_CURVE_WITH_KNOTS ( 'NONE', 3,
 ( #19103, #4416, #33770, #18626, #47958, #5381, #76862, #69755 ),
 .UNSPECIFIED., .F., .F.,
 ( 4, 2, 2, 4 ),
 ( 0.000000000000000000, 0.0009268394340039029598, 0.001390259151005891845, 0.001853678868007880729 ),
 .UNSPECIFIED. ) ;
#24240 = CARTESIAN_POINT ( 'NONE',  ( -68.06900606460516201, -276.9744843056770947, -336.6607821356309955 ) ) ;
#24241 = CARTESIAN_POINT ( 'NONE',  ( -1.500932584042229401, -275.7217004739361528, -202.6599503314498349 ) ) ;
#24242 = AXIS2_PLACEMENT_3D ( 'NONE', #5853, #91037, #26209 ) ;
#24243 = CARTESIAN_POINT ( 'NONE',  ( 21.42214121125835646, -281.2780248760547579, -319.7537405569395332 ) ) ;
#24244 = CARTESIAN_POINT ( 'NONE',  ( 25.10518689917867974, -289.8540604609663092, -310.0897010612146687 ) ) ;
#24245 = CARTESIAN_POINT ( 'NONE',  ( -111.9233616223406926, -297.8686651190229213, -286.4944227929585168 ) ) ;
#24246 = CARTESIAN_POINT ( 'NONE',  ( -112.2137909009417740, -297.5536698762014112, -286.5530525055098678 ) ) ;
#24247 = CARTESIAN_POINT ( 'NONE',  ( -60.85868035426064893, -293.7465757129684221, -199.2646379196514488 ) ) ;
#24248 = CARTESIAN_POINT ( 'NONE',  ( -1.574256382571885382, -280.5767895285446798, -336.1079355108132063 ) ) ;
#24249 = CARTESIAN_POINT ( 'NONE',  ( -7.443080109860269467, -282.3673964200521027, -202.1754339639073521 ) ) ;
#24250 = CARTESIAN_POINT ( 'NONE',  ( -94.70793355536595470, -295.2917258644264393, -222.9026038185263587 ) ) ;
#24251 = CARTESIAN_POINT ( 'NONE',  ( -96.96728401389962926, -286.7941413610985251, -222.9139877716735612 ) ) ;
#24252 = CARTESIAN_POINT ( 'NONE',  ( 33.37644657516987223, -286.7288443741358606, -289.8669640452080785 ) ) ;
#24253 = CARTESIAN_POINT ( 'NONE',  ( 204.9738417247596658, 294.2970692423710375, -68.59889679756817316 ) ) ;
#24254 = ORIENTED_EDGE ( 'NONE', *, *, #62073, .F. ) ;
#24255 = CARTESIAN_POINT ( 'NONE',  ( 25.35773390008506922, -286.7095393058192485, -314.1255814434051103 ) ) ;
#24256 = CARTESIAN_POINT ( 'NONE',  ( 31.86198634145748798, -286.9094217880578981, -247.0601037174077703 ) ) ;
#24257 = EDGE_LOOP ( 'NONE', ( #45765, #85180, #47173, #19244 ) ) ;
#24258 = CARTESIAN_POINT ( 'NONE',  ( -10.79607422713366738, -283.7937614361280794, -342.3676783022263521 ) ) ;
#24259 = CARTESIAN_POINT ( 'NONE',  ( 34.18613133314459418, -276.0791910466108448, -285.0531843216789980 ) ) ;
#24260 = CARTESIAN_POINT ( 'NONE',  ( -40.60544878184765594, -290.9323729833776611, -193.7265787106126425 ) ) ;
#24261 = CARTESIAN_POINT ( 'NONE',  ( 39.60839370530543846, -282.1980721830683478, -269.9225583204415102 ) ) ;
#24262 = CARTESIAN_POINT ( 'NONE',  ( -11.76019300876496132, -281.8992612281266474, -198.4147965194464973 ) ) ;
#24263 = CARTESIAN_POINT ( 'NONE',  ( 26.70664902961420850, -282.4476660923110671, -313.0642005608113436 ) ) ;
#24264 = CARTESIAN_POINT ( 'NONE',  ( -19.53455508040201138, -280.2874880685394032, -199.5140147040914940 ) ) ;
#24265 = CARTESIAN_POINT ( 'NONE',  ( -95.99890600148557951, -275.4094976428775681, -317.0979686699210447 ) ) ;
#24266 = CARTESIAN_POINT ( 'NONE',  ( 161.9590788367351024, 220.0586530115249673, -205.3424623035032539 ) ) ;
#24267 = VERTEX_POINT ( 'NONE', #28189 ) ;
#24268 = CARTESIAN_POINT ( 'NONE',  ( 28.23101078672630493, -277.0705438268601597, -234.1942328955582298 ) ) ;
#24269 = CARTESIAN_POINT ( 'NONE',  ( -100.5620283310121010, -247.3436685628221312, -333.7792060084481136 ) ) ;
#24270 = CARTESIAN_POINT ( 'NONE',  ( 19.22715532734573074, -278.8937998667427678, -221.6402424963064846 ) ) ;
#24271 = CARTESIAN_POINT ( 'NONE',  ( -33.79758114230445187, -297.4462576118440893, -197.2595890160661440 ) ) ;
#24272 = CARTESIAN_POINT ( 'NONE',  ( 6.466340202544196281, -292.1377740889748793, -207.1125408801742367 ) ) ;
#24273 = CARTESIAN_POINT ( 'NONE',  ( 103.6749136203638813, 114.2737147223544980, -279.7089131145189640 ) ) ;
#24275 = CARTESIAN_POINT ( 'NONE',  ( -102.3574731148658685, -288.4797317077532739, -305.3892826583979740 ) ) ;
#24274 = CARTESIAN_POINT ( 'NONE',  ( -95.11359383969195846, -295.8083714035957996, -220.2720288792392580 ) ) ;
#24276 = CARTESIAN_POINT ( 'NONE',  ( -109.1586195450475287, -298.1679774236464482, -289.2048122262592074 ) ) ;
#24277 = CARTESIAN_POINT ( 'NONE',  ( 26.78958423513960341, -288.3783803064957283, -234.3624424061470677 ) ) ;
#24278 = ORIENTED_EDGE ( 'NONE', *, *, #50050, .F. ) ;
#24279 = CARTESIAN_POINT ( 'NONE',  ( 17.31363320724381083, -293.7501166772028114, -216.3825256813565545 ) ) ;
#24280 = CARTESIAN_POINT ( 'NONE',  ( -93.30627762578858153, -285.7109073314539955, -223.3935280152225289 ) ) ;
#24281 = CARTESIAN_POINT ( 'NONE',  ( -77.97875646948075712, -296.3137849303000166, -205.4254700686850299 ) ) ;
#24282 = CARTESIAN_POINT ( 'NONE',  ( -13.92541250117955443, -293.1511306104014238, -197.1216835612295313 ) ) ;
#24283 = CARTESIAN_POINT ( 'NONE',  ( 11.07519197877918771, -293.1939908009152873, -210.4985030882643287 ) ) ;
#24284 = CARTESIAN_POINT ( 'NONE',  ( -26.47279292304417808, -289.0768105271383774, -342.5985018234167114 ) ) ;
#24285 = ORIENTED_EDGE ( 'NONE', *, *, #54972, .F. ) ;
#24286 = CARTESIAN_POINT ( 'NONE',  ( 157.1249521815137484, 17.17215575532202010, 9.360165637272318762 ) ) ;
#24287 = CARTESIAN_POINT ( 'NONE',  ( -36.58036543080844893, -299.9219959840034448, -194.5960722939407788 ) ) ;
#24288 = CARTESIAN_POINT ( 'NONE',  ( -92.87368841189365298, -272.0721504827067747, -217.5763947807699594 ) ) ;
#24289 = CARTESIAN_POINT ( 'NONE',  ( 33.18280814012359770, -280.8709796995106558, -290.1019939021576874 ) ) ;
#24290 = ORIENTED_EDGE ( 'NONE', *, *, #73275, .F. ) ;
#24291 = ADVANCED_FACE ( 'NONE', ( #42836 ), #86380, .T. ) ;
#24292 = CARTESIAN_POINT ( 'NONE',  ( -82.51521924894002780, -277.1586896621950586, -332.6417736735991184 ) ) ;
#24293 = CARTESIAN_POINT ( 'NONE',  ( -110.6784991410187757, -271.0597417575163490, -262.1055547055786406 ) ) ;
#24294 = CARTESIAN_POINT ( 'NONE',  ( -111.5873350432268722, -280.4446259531778196, -267.8903948359456990 ) ) ;
#24295 = CARTESIAN_POINT ( 'NONE',  ( 12.56080270789499487, -274.4878402604188636, -325.3908880768925656 ) ) ;
#24296 = CARTESIAN_POINT ( 'NONE',  ( -98.78835777911763216, -298.3116221860647101, -230.1263875913131187 ) ) ;
#24297 = CARTESIAN_POINT ( 'NONE',  ( -103.4225237095337206, -273.9189986462070010, -238.7900362436460000 ) ) ;
#24298 = CARTESIAN_POINT ( 'NONE',  ( -62.59928861108281239, -299.3289698360263174, -198.4688747391317634 ) ) ;
#24299 = CARTESIAN_POINT ( 'NONE',  ( 6.303319244628854179, -272.6612211715428771, -208.8680902416132596 ) ) ;
#24300 = CARTESIAN_POINT ( 'NONE',  ( 29.94632766610666508, -293.8189749331306757, -241.6621893811352777 ) ) ;
#24301 = CARTESIAN_POINT ( 'NONE',  ( -37.53340930219462024, -290.6244680464102998, -196.7595922293898525 ) ) ;
#24302 = CARTESIAN_POINT ( 'NONE',  ( 193.9153122143737562, 214.9910457053126720, 17.21343741151142481 ) ) ;
#24303 = CARTESIAN_POINT ( 'NONE',  ( -74.06195589420678971, -278.0189512674766092, -337.9863856052576239 ) ) ;
#24304 = CARTESIAN_POINT ( 'NONE',  ( 51.69745723989969832, -299.5303143563324966, -197.3348114162781428 ) ) ;
#24305 = CARTESIAN_POINT ( 'NONE',  ( -1.877699816360418383, -281.2771417231817850, -338.1519946243802792 ) ) ;
#24306 = CARTESIAN_POINT ( 'NONE',  ( -64.90689019827060235, -297.4114969678361717, -340.3048835006177910 ) ) ;
#24307 = DIRECTION ( 'NONE',  ( -0.000000000000000000, -1.000000000000000000, -0.000000000000000000 ) ) ;
#24308 = CARTESIAN_POINT ( 'NONE',  ( -76.22157757107966347, -282.7831746026973860, -332.3964905384666508 ) ) ;
#24309 = CARTESIAN_POINT ( 'NONE',  ( -84.96106770288503185, -281.7072597180340949, -328.5197308893282866 ) ) ;
#24310 = EDGE_CURVE ( 'NONE', #19733, #1988, #54851, .T. ) ;
#24311 = CARTESIAN_POINT ( 'NONE',  ( 30.72670629406963627, -273.7534867197089170, -242.2617713174311689 ) ) ;
#24312 = CARTESIAN_POINT ( 'NONE',  ( 21.43851144482888316, -282.9121620262820898, -223.7588380462409816 ) ) ;
#24313 = DIRECTION ( 'NONE',  ( 0.000000000000000000, 0.000000000000000000, -1.000000000000000000 ) ) ;
#24314 = DIRECTION ( 'NONE',  ( 0.7957555401921962979, 0.6056179655966504871, 0.000000000000000000 ) ) ;
#24315 = CARTESIAN_POINT ( 'NONE',  ( -98.90851247555033865, -271.5552406034108799, -225.3741209302029347 ) ) ;
#24316 = AXIS2_PLACEMENT_3D ( 'NONE', #87698, #87243, #43246 ) ;
#24317 = CARTESIAN_POINT ( 'NONE',  ( -42.65064294726608551, -279.1191573723599504, -345.3400720521835296 ) ) ;
#24318 = DIRECTION ( 'NONE',  ( 1.000000000000000000, 0.000000000000000000, 0.000000000000000000 ) ) ;
#24319 = CARTESIAN_POINT ( 'NONE',  ( -51.91986632276809388, -287.7872970238780113, -196.1673931677192968 ) ) ;
#24320 = CARTESIAN_POINT ( 'NONE',  ( 157.2348298300751708, 18.48484813927241177, -11.40642999294778015 ) ) ;
#24321 = CARTESIAN_POINT ( 'NONE',  ( -111.8195757655022362, -288.4331562028644385, -279.6161404091726581 ) ) ;
#24322 = CARTESIAN_POINT ( 'NONE',  ( 140.6539576904058606, 275.0000000000000568, 11.50000000000000000 ) ) ;
#24323 = CARTESIAN_POINT ( 'NONE',  ( -97.19771252494237501, -295.9370350467070239, -227.8830261546357008 ) ) ;
#24324 = CARTESIAN_POINT ( 'NONE',  ( 18.74342339430308613, -286.3740383488456018, -319.0726523023352001 ) ) ;
#24325 = CARTESIAN_POINT ( 'NONE',  ( -104.1716275211822733, -250.7505522545870349, -322.2422935457555582 ) ) ;
#24326 = CARTESIAN_POINT ( 'NONE',  ( -110.1093869337224476, -294.7858889324204483, -252.1464442234635044 ) ) ;
#24327 = CARTESIAN_POINT ( 'NONE',  ( 38.91045972137419540, -286.0830735237381646, -274.4056629616819123 ) ) ;
#24328 = CARTESIAN_POINT ( 'NONE',  ( 35.49638471936595607, -283.3072586647704725, -282.2377257329421809 ) ) ;
#24329 = CARTESIAN_POINT ( 'NONE',  ( -58.22999750475583625, -281.5581957003898310, -343.4751341312302770 ) ) ;
#24330 = CARTESIAN_POINT ( 'NONE',  ( -52.36976945815977302, -291.8544398752798656, -198.8728319199562691 ) ) ;
#24331 = CARTESIAN_POINT ( 'NONE',  ( 35.61450675344872963, -282.8464425558232165, -260.3514056018166229 ) ) ;
#24332 = CARTESIAN_POINT ( 'NONE',  ( 35.30138319815173986, -282.4748614151007473, -279.4682145734781784 ) ) ;
#24333 = CARTESIAN_POINT ( 'NONE',  ( 32.32887229441965360, -289.1576213026174855, -241.5122298157696434 ) ) ;
#24334 = CARTESIAN_POINT ( 'NONE',  ( -102.7033263310560613, -273.4175613933858813, -229.6966112035494518 ) ) ;
#24335 = EDGE_LOOP ( 'NONE', ( #24254, #54781, #49576, #39692 ) ) ;
#24336 = ORIENTED_EDGE ( 'NONE', *, *, #35942, .T. ) ;
#24337 = CARTESIAN_POINT ( 'NONE',  ( -15.39432758174546834, -286.8502131026759230, -342.7181516561406056 ) ) ;
#24338 = CARTESIAN_POINT ( 'NONE',  ( 34.72175344733467739, -275.2089597335130406, -243.2344031283086849 ) ) ;
#24339 = CARTESIAN_POINT ( 'NONE',  ( 5.425844954331937586, -294.6136720717660751, -209.1194750718689761 ) ) ;
#24340 = DIRECTION ( 'NONE',  ( -0.000000000000000000, 1.000000000000000000, 0.000000000000000000 ) ) ;
#24341 = CARTESIAN_POINT ( 'NONE',  ( 39.58706461736021254, -284.0519495502703080, -270.3284710469133074 ) ) ;
#24342 = CARTESIAN_POINT ( 'NONE',  ( -9.905297844479640901, -274.6945206840613309, -340.3416313900506225 ) ) ;
#24343 = LINE ( 'NONE', #82099, #23174 ) ;
#24344 = CARTESIAN_POINT ( 'NONE',  ( -99.25948310422523946, -295.5467948971788701, -225.9468346075454406 ) ) ;
#24345 = CARTESIAN_POINT ( 'NONE',  ( -73.03150804686684694, -293.1713289379279104, -205.7074153091119513 ) ) ;
#24346 = CARTESIAN_POINT ( 'NONE',  ( -46.18289457702470457, -273.2856150381182943, -197.7957960390364462 ) ) ;
#24347 = CARTESIAN_POINT ( 'NONE',  ( -91.08525879867467268, -291.3527980317498418, -320.8572153504027824 ) ) ;
#24348 = CARTESIAN_POINT ( 'NONE',  ( -91.85629734562050430, -292.1911997559498673, -221.4387056104807812 ) ) ;
#24349 = CARTESIAN_POINT ( 'NONE',  ( -100.4853845514942776, -286.8381779065268233, -231.6519090120511066 ) ) ;
#24350 = CARTESIAN_POINT ( 'NONE',  ( -36.40397259429063581, -293.4889587330746394, -193.9431664607276673 ) ) ;
#24351 = CARTESIAN_POINT ( 'NONE',  ( -8.711406675527110011, -293.7342261557831193, -199.4132175916119536 ) ) ;
#24352 = CARTESIAN_POINT ( 'NONE',  ( -45.09284468568896642, -294.9862212372054842, -342.9989198077045103 ) ) ;
#24353 = CARTESIAN_POINT ( 'NONE',  ( 21.08719573798560276, -290.1993422423867059, -317.3830786111255406 ) ) ;
#24354 = CARTESIAN_POINT ( 'NONE',  ( 38.25428318341963063, -281.5357731262338916, -255.7239286454167200 ) ) ;
#24355 = CARTESIAN_POINT ( 'NONE',  ( -94.46608116275987754, -295.3135696117554971, -220.8248032016122977 ) ) ;
#24356 = CARTESIAN_POINT ( 'NONE',  ( -113.1373569456931847, -284.2121577861798869, -284.2192529820676441 ) ) ;
#24357 = CARTESIAN_POINT ( 'NONE',  ( 8.612400029370858690, -278.3993572042601272, -329.2493368985307711 ) ) ;
#24358 = CARTESIAN_POINT ( 'NONE',  ( -95.44011067312165153, -282.7188007381790840, -315.2336758597690505 ) ) ;
#24359 = CARTESIAN_POINT ( 'NONE',  ( 34.85213977616518832, -285.8140253508835826, -290.7317924749037275 ) ) ;
#24360 = CARTESIAN_POINT ( 'NONE',  ( -20.42531841213682142, -274.9768567483539528, -344.2671146811232461 ) ) ;
#24361 = DIRECTION ( 'NONE',  ( 0.000000000000000000, 1.000000000000000000, 0.000000000000000000 ) ) ;
#24362 = CARTESIAN_POINT ( 'NONE',  ( -64.08372878085729951, -282.9183100446239791, -338.3526788209623533 ) ) ;
#24363 = CARTESIAN_POINT ( 'NONE',  ( -67.22180021340106748, -280.8740381786061562, -199.8261030034607302 ) ) ;
#24364 = CARTESIAN_POINT ( 'NONE',  ( 16.51231838533912821, -287.3683010807159235, -325.1393639240641846 ) ) ;
#24365 = CARTESIAN_POINT ( 'NONE',  ( 15.04920196383539910, -296.0611896813401245, -322.7129060200044250 ) ) ;
#24366 = CARTESIAN_POINT ( 'NONE',  ( 31.81832029625696734, -276.7372646615794451, -238.2459767620450179 ) ) ;
#24367 = CARTESIAN_POINT ( 'NONE',  ( -5.335921001910500117, -275.7797282813993434, -200.8706267114634159 ) ) ;
#24368 = CARTESIAN_POINT ( 'NONE',  ( -85.10684501570408145, -277.5663644770924634, -325.6321643212310732 ) ) ;
#24369 = CARTESIAN_POINT ( 'NONE',  ( -103.4996737246296306, -274.9934036946292508, -235.6807659431107709 ) ) ;
#24370 = CARTESIAN_POINT ( 'NONE',  ( 36.56595996537395621, -285.7040377118107699, -282.1765833907036267 ) ) ;
#24371 = CARTESIAN_POINT ( 'NONE',  ( -111.4795524898663501, -291.9290519155388210, -288.0242503932797149 ) ) ;
#24372 = CARTESIAN_POINT ( 'NONE',  ( -58.51058166895605694, -294.2527064381346236, -340.5473312100658632 ) ) ;
#24373 = EDGE_LOOP ( 'NONE', ( #60077, #42239, #11123, #14160 ) ) ;
#24374 = CARTESIAN_POINT ( 'NONE',  ( -65.33114033562596035, -291.3426767237926924, -202.9037071871791227 ) ) ;
#24375 = VERTEX_POINT ( 'NONE', #77913 ) ;
#24376 = CARTESIAN_POINT ( 'NONE',  ( -5.741253553265432963, -289.7259302266780310, -340.2388990512517921 ) ) ;
#24377 = CARTESIAN_POINT ( 'NONE',  ( -94.02481673644157922, -279.8560606211833601, -224.1992618660642336 ) ) ;
#24378 = EDGE_CURVE ( 'NONE', #59329, #45702, #21618, .T. ) ;
#24379 = CARTESIAN_POINT ( 'NONE',  ( -114.0000852372007785, -295.5180006597656757, -266.7361233282131820 ) ) ;
#24380 = CARTESIAN_POINT ( 'NONE',  ( 12.35627453661135178, -289.0322970860686382, -329.0418141313459159 ) ) ;
#24381 = CARTESIAN_POINT ( 'NONE',  ( -26.62824829141964855, -286.5180321343456171, -194.0779399989860394 ) ) ;
#24382 = CARTESIAN_POINT ( 'NONE',  ( -102.2591279873634136, -285.3398042651627406, -236.9273768395715365 ) ) ;
#24383 = CARTESIAN_POINT ( 'NONE',  ( 138.6955843366410477, 180.6821896333715642, -241.4130191322238090 ) ) ;
#24384 = CARTESIAN_POINT ( 'NONE',  ( -14.30945429173846861, -91.08059216271270486, -358.4537093730789934 ) ) ;
#24385 = CARTESIAN_POINT ( 'NONE',  ( 102.5375343959159409, 114.7846795236941801, -279.4961139801552008 ) ) ;
#24386 = AXIS2_PLACEMENT_3D ( 'NONE', #46251, #31601, #82247 ) ;
#24387 = CARTESIAN_POINT ( 'NONE',  ( -96.22904551800844786, -277.1419397117301173, -313.7973516018416262 ) ) ;
#24388 = CARTESIAN_POINT ( 'NONE',  ( -73.00435616091196778, -276.4568957866198957, -334.4255505339396564 ) ) ;
#24389 = CARTESIAN_POINT ( 'NONE',  ( -81.23484655183182213, -273.1404642512579812, -207.0578043764131166 ) ) ;
#24390 = CARTESIAN_POINT ( 'NONE',  ( -81.50421288696699662, -219.8904477667203423, -350.0058313318409091 ) ) ;
#24391 = CARTESIAN_POINT ( 'NONE',  ( -20.25265699324641488, -275.5220109419201435, -344.9893587204326195 ) ) ;
#24392 = VERTEX_POINT ( 'NONE', #49015 ) ;
#24393 = CARTESIAN_POINT ( 'NONE',  ( -98.89023426883694867, -290.5004214998705834, -309.7281903496019027 ) ) ;
#24394 = CARTESIAN_POINT ( 'NONE',  ( -26.24898243239163165, -298.9905479402500532, -193.5211247304686424 ) ) ;
#24395 = CARTESIAN_POINT ( 'NONE',  ( 34.48149372902969390, -286.0328558528602798, -254.7831751228318922 ) ) ;
#24396 = CARTESIAN_POINT ( 'NONE',  ( -112.9695772163608609, -273.3814310284679436, -256.1577181962400118 ) ) ;
#24397 = CARTESIAN_POINT ( 'NONE',  ( -0.7561117800409273837, -294.7186870207760307, -333.5891748917225073 ) ) ;
#24398 = ORIENTED_EDGE ( 'NONE', *, *, #74108, .F. ) ;
#24399 = CARTESIAN_POINT ( 'NONE',  ( -9.715114130673581982, -278.6142025350492872, -340.6895328978299631 ) ) ;
#24400 = CARTESIAN_POINT ( 'NONE',  ( 38.08397996782814943, -281.2498314348806616, -285.5431364755187360 ) ) ;
#24401 = CARTESIAN_POINT ( 'NONE',  ( -77.00059252077886640, -280.5871340552306492, -208.6451161851530287 ) ) ;
#24402 = CARTESIAN_POINT ( 'NONE',  ( -64.70890802028478106, -279.1646478538789324, -341.3039601053520187 ) ) ;
#24403 = CARTESIAN_POINT ( 'NONE',  ( -55.42100330385038376, -296.3898035015602090, -198.9745699923344944 ) ) ;
#24404 = DIRECTION ( 'NONE',  ( -1.000000000000000000, 0.000000000000000000, 0.000000000000000000 ) ) ;
#24405 = CARTESIAN_POINT ( 'NONE',  ( 7.140644628064522159, -280.8438686885869515, -212.4152043230975835 ) ) ;
#24406 = CARTESIAN_POINT ( 'NONE',  ( -5.191159919539834355, -275.2674697424185979, -200.5721390139836160 ) ) ;
#24407 = CARTESIAN_POINT ( 'NONE',  ( 3.745638410918268768, -276.6048393869630218, -207.5553387367040727 ) ) ;
#24408 = CARTESIAN_POINT ( 'NONE',  ( 22.17056912219155862, -274.7743899400160217, -318.3077515418177086 ) ) ;
#24409 = LINE ( 'NONE', #35266, #21616 ) ;
#24410 = CARTESIAN_POINT ( 'NONE',  ( -37.54014644930101241, -291.2468069710749319, -197.1874386311807257 ) ) ;
#24411 = CARTESIAN_POINT ( 'NONE',  ( -106.9169477159257298, -283.4806887771613333, -303.1116555256169818 ) ) ;
#24412 = CARTESIAN_POINT ( 'NONE',  ( 24.54194855393093277, -279.2357613747554410, -229.6683071991789689 ) ) ;
#24414 = CARTESIAN_POINT ( 'NONE',  ( -42.75491583615490043, -284.0631926679507160, -196.1053225074954014 ) ) ;
#24413 = CARTESIAN_POINT ( 'NONE',  ( -2.857032426758452814, -279.0920222158111983, -205.3377278435614244 ) ) ;
#24415 = CARTESIAN_POINT ( 'NONE',  ( -90.32403512216293962, -291.8014999248620711, -323.5171117343874130 ) ) ;
#24416 = CARTESIAN_POINT ( 'NONE',  ( 0.5920990663355960582, -281.7747204122753715, -207.4679266904495307 ) ) ;
#24417 = CARTESIAN_POINT ( 'NONE',  ( -90.47617882071700990, -230.2765427179325286, -347.7368260604238799 ) ) ;
#24418 = CARTESIAN_POINT ( 'NONE',  ( 15.18715772473031045, -280.7251099493178685, -325.5622004605534698 ) ) ;
#24419 = CARTESIAN_POINT ( 'NONE',  ( 29.14154204925274527, -296.0120784346138407, -305.0739276553849209 ) ) ;
#24420 = CARTESIAN_POINT ( 'NONE',  ( -113.2213105307398706, -276.7409103644632182, -274.3933303680112772 ) ) ;
#24421 = CARTESIAN_POINT ( 'NONE',  ( -78.14269652366500907, -285.5995863300524888, -333.4904068913745050 ) ) ;
#24422 = DIRECTION ( 'NONE',  ( 0.9951408606192336803, 0.000000000000000000, -0.09846150276128748380 ) ) ;
#24423 = CARTESIAN_POINT ( 'NONE',  ( -22.50100615812577942, -294.1607292567056220, -196.2195660561077091 ) ) ;
#24424 = CARTESIAN_POINT ( 'NONE',  ( 36.34306764750854768, -273.3724385934021370, -256.3769966574627688 ) ) ;
#24425 = EDGE_CURVE ( 'NONE', #31737, #14834, #89578, .T. ) ;
#24426 = CARTESIAN_POINT ( 'NONE',  ( -23.80428531193216557, -285.4179281268925479, -194.6704006844306605 ) ) ;
#24427 = CARTESIAN_POINT ( 'NONE',  ( -88.47030150166332874, -289.7211053199843604, -217.0710952870387302 ) ) ;
#24428 = CARTESIAN_POINT ( 'NONE',  ( -43.27399328867051054, -275.1182110581578968, -431.5594140723246142 ) ) ;
#24429 = CARTESIAN_POINT ( 'NONE',  ( 34.37080563932354949, -274.4484211837949488, -286.4980869032250439 ) ) ;
#24430 = CARTESIAN_POINT ( 'NONE',  ( -72.73398813780681849, -293.6656382630285975, -335.6309095064376606 ) ) ;
#24431 = CARTESIAN_POINT ( 'NONE',  ( -108.8262173792317071, -291.6437048250788280, -287.4259142884952780 ) ) ;
#24432 =( LENGTH_UNIT ( ) NAMED_UNIT ( * ) SI_UNIT ( .MILLI., .METRE. ) );
#24433 = DIRECTION ( 'NONE',  ( 0.9167375550253600291, 0.000000000000000000, -0.3994899938748465162 ) ) ;
#24434 = CARTESIAN_POINT ( 'NONE',  ( 32.77178717436432009, -292.4205988863936341, -300.6077110494586577 ) ) ;
#24435 = CARTESIAN_POINT ( 'NONE',  ( 35.35184890735979479, -288.9824010763321667, -257.3419091747679204 ) ) ;
#24436 = CARTESIAN_POINT ( 'NONE',  ( -68.95641830046618281, -287.7020170022026946, -339.4729923134647720 ) ) ;
#24437 = CARTESIAN_POINT ( 'NONE',  ( -25.06121472957277518, -287.6369597817675867, -197.7520880520980313 ) ) ;
#24438 = EDGE_CURVE ( 'NONE', #60939, #44442, #48773, .T. ) ;
#24439 = FACE_OUTER_BOUND ( 'NONE', #33451, .T. ) ;
#24440 = CARTESIAN_POINT ( 'NONE',  ( 35.71321976717246827, -288.2918730419319218, -265.5659547483629694 ) ) ;
#24441 = CARTESIAN_POINT ( 'NONE',  ( 10.18099072548088024, -296.3808755274444593, -328.9091508831531314 ) ) ;
#24442 = CARTESIAN_POINT ( 'NONE',  ( 189.4188515237862589, 293.9636489450775798, -40.00000000000000711 ) ) ;
#24443 = CARTESIAN_POINT ( 'NONE',  ( 2.521216304964259525, -287.7791631970455342, -204.9473838612087206 ) ) ;
#24444 = CARTESIAN_POINT ( 'NONE',  ( -56.58142202532947351, -275.3779631582436309, -343.4846152209454431 ) ) ;
#24445 = AXIS2_PLACEMENT_3D ( 'NONE', #316, #78925, #29200 ) ;
#24446 = CARTESIAN_POINT ( 'NONE',  ( -31.44764903199635242, -277.3130646882670476, -347.1666058702533064 ) ) ;
#24447 = AXIS2_PLACEMENT_3D ( 'NONE', #56017, #34244, #6773 ) ;
#24448 = CARTESIAN_POINT ( 'NONE',  ( -96.79839363741176328, -278.8760408989688813, -221.4463899661410835 ) ) ;
#24449 = CARTESIAN_POINT ( 'NONE',  ( -98.23889027957277165, -299.1214885582957663, -227.1942436946234807 ) ) ;
#24450 = CARTESIAN_POINT ( 'NONE',  ( -91.07853552446604795, -283.2891324063336924, -217.9668976538289940 ) ) ;
#24451 = CARTESIAN_POINT ( 'NONE',  ( -48.18343439339133027, -254.1872365014070567, -480.9328361744650806 ) ) ;
#24452 = CARTESIAN_POINT ( 'NONE',  ( -35.61063931487311862, -278.2136496439624125, -196.1334875865333345 ) ) ;
#24453 = CARTESIAN_POINT ( 'NONE',  ( -63.24577554830538872, -281.3894433031443327, -340.7456299500937007 ) ) ;
#24454 = DIRECTION ( 'NONE',  ( 0.000000000000000000, 1.000000000000000000, 0.000000000000000000 ) ) ;
#24455 = CARTESIAN_POINT ( 'NONE',  ( 18.38353865410130084, -274.7495234025461741, -322.4898578038768164 ) ) ;
#24456 = CIRCLE ( 'NONE', #48721, 7.999911143031724237 ) ;
#24457 = CARTESIAN_POINT ( 'NONE',  ( -108.5102420067338613, -298.3230722891153164, -251.1879456888849802 ) ) ;
#24458 = CARTESIAN_POINT ( 'NONE',  ( -1.789691986299157600, -281.5126062630589558, -338.3136545627217515 ) ) ;
#24459 = CARTESIAN_POINT ( 'NONE',  ( -86.26635031143904087, -298.2943618780874999, -215.8653653777751913 ) ) ;
#24460 = CARTESIAN_POINT ( 'NONE',  ( -82.69181694050016063, -298.7622603900347258, -208.6781987236896327 ) ) ;
#24461 = CARTESIAN_POINT ( 'NONE',  ( -27.28306850219224344, -273.8500880996937212, -197.9851644768884000 ) ) ;
#24462 = CARTESIAN_POINT ( 'NONE',  ( 29.25097073197279585, -295.0955987860050413, -235.8587001906870455 ) ) ;
#24463 = CARTESIAN_POINT ( 'NONE',  ( 38.97498825534740519, -287.5908240312026010, -260.1257343214477942 ) ) ;
#24464 = CARTESIAN_POINT ( 'NONE',  ( -17.34902550193605819, -278.3880463476678528, -197.4940667407226158 ) ) ;
#24465 = CARTESIAN_POINT ( 'NONE',  ( -113.1336791305963629, -290.2146312597466249, -284.0214761722375556 ) ) ;
#24466 = CARTESIAN_POINT ( 'NONE',  ( -5.701593651523235273, -287.6842543087848298, -336.4089196955332568 ) ) ;
#24467 = CARTESIAN_POINT ( 'NONE',  ( -22.56231309923966677, -290.2410455669007661, -196.7788155332748659 ) ) ;
#24468 = ORIENTED_EDGE ( 'NONE', *, *, #44600, .F. ) ;
#24469 = CARTESIAN_POINT ( 'NONE',  ( 64.33209501061345748, 48.33985520751024723, -319.1928417150128325 ) ) ;
#24470 = CARTESIAN_POINT ( 'NONE',  ( 34.81901371492742214, -287.2116075843571252, -281.8784526811728028 ) ) ;
#24471 = DIRECTION ( 'NONE',  ( 0.000000000000000000, 1.000000000000000000, -0.000000000000000000 ) ) ;
#24472 = CARTESIAN_POINT ( 'NONE',  ( -111.2616508970563700, -285.2331650046268692, -291.0652502186668471 ) ) ;
#24473 = B_SPLINE_CURVE_WITH_KNOTS ( 'NONE', 3,
 ( #53908, #16991, #80927, #73826, #45856, #38287 ),
 .UNSPECIFIED., .F., .F.,
 ( 4, 2, 4 ),
 ( 0.000000000000000000, 0.0009305040472776272007, 0.001861008094555254401 ),
 .UNSPECIFIED. ) ;
#24474 = CARTESIAN_POINT ( 'NONE',  ( 39.42117042560284546, -292.5744765684802928, -267.4574972070860213 ) ) ;
#24475 = CARTESIAN_POINT ( 'NONE',  ( -14.39175285408332527, -281.6586652991696837, -197.3220325178714347 ) ) ;
#24476 = CARTESIAN_POINT ( 'NONE',  ( -33.49834767716119899, -282.8357820932210416, -343.2724466855644323 ) ) ;
#24477 = CARTESIAN_POINT ( 'NONE',  ( -95.57109836026283745, -297.2334133979523472, -219.8996278501121537 ) ) ;
#24478 = CARTESIAN_POINT ( 'NONE',  ( 3.188035407583913461, -275.9240371819360007, -208.9930138490575757 ) ) ;
#24479 = CARTESIAN_POINT ( 'NONE',  ( 33.36706195070001257, -291.2595873517217910, -246.2810699170521502 ) ) ;
#24480 = CARTESIAN_POINT ( 'NONE',  ( -51.62378165303672972, -272.6604384965845043, -198.3149335167148877 ) ) ;
#24481 = EDGE_LOOP ( 'NONE', ( #19524, #61524, #78205, #44190 ) ) ;
#24482 = CYLINDRICAL_SURFACE ( 'NONE', #12292, 4.000000000000003553 ) ;
#24483 = CARTESIAN_POINT ( 'NONE',  ( 12.07202850344957490, -288.6653354229004549, -214.6178517937098889 ) ) ;
#24484 = CARTESIAN_POINT ( 'NONE',  ( -41.91333471279364886, -296.1880208556428329, -346.9678092934881874 ) ) ;
#24485 = CARTESIAN_POINT ( 'NONE',  ( -109.2948325731119468, -285.3745483237959206, -257.3817654379772648 ) ) ;
#24486 = CARTESIAN_POINT ( 'NONE',  ( 38.50137692911469856, -274.7638586038412427, -282.5539144076752791 ) ) ;
#24487 = CARTESIAN_POINT ( 'NONE',  ( 39.50532147334272537, -294.2386464028530781, -273.1625564121264915 ) ) ;
#24488 = CARTESIAN_POINT ( 'NONE',  ( 38.40565889229098673, -285.6710715229108928, -268.7353629995159849 ) ) ;
#24489 = CARTESIAN_POINT ( 'NONE',  ( -8.392049326693530986, -295.0167837230858368, -341.7454343499975948 ) ) ;
#24490 = CARTESIAN_POINT ( 'NONE',  ( -82.55603613438269406, -290.0230144106735111, -327.7000341406693451 ) ) ;
#24491 = DIRECTION ( 'NONE',  ( 0.000000000000000000, 0.000000000000000000, -1.000000000000000000 ) ) ;
#24492 = CARTESIAN_POINT ( 'NONE',  ( 29.33919985515026596, -277.8906705383787994, 30.50000000000000000 ) ) ;
#24493 = CARTESIAN_POINT ( 'NONE',  ( 25.94973956712686558, -24.33012855057486235, -341.4681489864074138 ) ) ;
#24494 = CARTESIAN_POINT ( 'NONE',  ( -113.6608146783961644, -286.0409121809512385, -272.8461437193658412 ) ) ;
#24495 = CARTESIAN_POINT ( 'NONE',  ( -115.3288506153726871, -276.2666405000204009, -252.5284128619063608 ) ) ;
#24496 = EDGE_LOOP ( 'NONE', ( #46361, #93472 ) ) ;
#24497 = EDGE_CURVE ( 'NONE', #70758, #65093, #7955, .T. ) ;
#24498 = CARTESIAN_POINT ( 'NONE',  ( -105.5064114206802657, -283.1114868663364064, -297.4771022698009233 ) ) ;
#24499 = CARTESIAN_POINT ( 'NONE',  ( 23.31248646181306938, -284.1506537662010601, -314.2134007783670313 ) ) ;
#24500 = CARTESIAN_POINT ( 'NONE',  ( 203.6509206358264521, 291.0907986494672741, -82.86876765886761120 ) ) ;
#24501 = ADVANCED_FACE ( 'NONE', ( #49483 ), #42361, .T. ) ;
#24502 = CARTESIAN_POINT ( 'NONE',  ( -16.32148925057807531, -281.3604953158954913, -343.8785997295915422 ) ) ;
#24503 = CARTESIAN_POINT ( 'NONE',  ( 32.52278763216855140, -285.2275562111103682, -243.9319973170634626 ) ) ;
#24504 = CARTESIAN_POINT ( 'NONE',  ( 10.97939469670758150, -276.5726148857862086, -211.9373512105311477 ) ) ;
#24505 = CARTESIAN_POINT ( 'NONE',  ( -108.3573470856543395, -296.8175114242272912, -287.5826178669811384 ) ) ;
#24506 = ORIENTED_EDGE ( 'NONE', *, *, #84781, .F. ) ;
#24507 = CARTESIAN_POINT ( 'NONE',  ( -22.62562070889749322, -290.9293031027489178, -198.3563925603052667 ) ) ;
#24508 = CARTESIAN_POINT ( 'NONE',  ( -93.25416783655521158, -278.4810490424109730, -323.2305926496774191 ) ) ;
#24509 = CARTESIAN_POINT ( 'NONE',  ( 11.54652308041554853, -274.7527793088335102, -216.0810473614639022 ) ) ;
#24510 = CARTESIAN_POINT ( 'NONE',  ( 37.64605842034517025, -274.2698856891760784, -254.2263815589945750 ) ) ;
#24511 = PLANE ( 'NONE',  #12882 ) ;
#24512 = CARTESIAN_POINT ( 'NONE',  ( -17.11433242423346712, -272.3129813812006432, -198.0870943656183272 ) ) ;
#24513 = CARTESIAN_POINT ( 'NONE',  ( -33.44658098662642232, -296.4293190687830020, -346.6855667789506583 ) ) ;
#24514 = DIRECTION ( 'NONE',  ( -0.000000000000000000, -0.000000000000000000, 1.000000000000000000 ) ) ;
#24515 = CIRCLE ( 'NONE', #15462, 0.4999999999999998335 ) ;
#24516 = CARTESIAN_POINT ( 'NONE',  ( 196.5385635022496444, 69.63708600450605957, 11.34458575897557964 ) ) ;
#24517 = AXIS2_PLACEMENT_3D ( 'NONE', #17831, #10708, #39564 ) ;
#24518 = CARTESIAN_POINT ( 'NONE',  ( -69.13081775439476928, -284.5600932693857317, -336.4331194644827860 ) ) ;
#24519 = CARTESIAN_POINT ( 'NONE',  ( -27.48109341731289135, -284.6887971079321460, -345.7579379232313386 ) ) ;
#24520 = CARTESIAN_POINT ( 'NONE',  ( -83.70612531882298413, -284.7450988206101101, -213.7778097407478128 ) ) ;
#24521 = CARTESIAN_POINT ( 'NONE',  ( -43.29168214279628302, -275.5284090766885470, -343.9208768822827551 ) ) ;
#24522 = CARTESIAN_POINT ( 'NONE',  ( -29.28748367663341057, -284.8095956700114471, -344.2094622355289175 ) ) ;
#24523 = CARTESIAN_POINT ( 'NONE',  ( -97.46244542330643412, -276.4423202433099505, -312.9999833993916809 ) ) ;
#24524 = CARTESIAN_POINT ( 'NONE',  ( 17.67628227916047834, -277.3208827556949245, -318.8284625850415637 ) ) ;
#24525 = CARTESIAN_POINT ( 'NONE',  ( 207.3218713672209219, 35.53307536961114721, 15.03205023726508038 ) ) ;
#24526 = VECTOR ( 'NONE', #90224, 1000.000000000000000 ) ;
#24527 = CARTESIAN_POINT ( 'NONE',  ( -110.3993511451267153, -279.6570038845173940, -246.3859047144919145 ) ) ;
#24528 = CARTESIAN_POINT ( 'NONE',  ( 29.23019569692301900, -281.5424973701628915, -231.7902793948342435 ) ) ;
#24529 = ORIENTED_EDGE ( 'NONE', *, *, #91068, .T. ) ;
#24530 = CARTESIAN_POINT ( 'NONE',  ( 195.2847367049472780, 40.73792109368745429, 14.92657523498152550 ) ) ;
#24531 = CARTESIAN_POINT ( 'NONE',  ( 24.52261197436325091, -288.8240242273793683, -226.5996191902540886 ) ) ;
#24532 = CARTESIAN_POINT ( 'NONE',  ( -109.3028118137348201, -295.5746768557292512, -283.6290598565807386 ) ) ;
#24533 = CARTESIAN_POINT ( 'NONE',  ( -107.6415570050170203, -289.5010397780856692, -301.6568865569068976 ) ) ;
#24535 = CARTESIAN_POINT ( 'NONE',  ( -106.9936658628939483, -288.4632050414346622, -295.3926517285303248 ) ) ;
#24534 = CARTESIAN_POINT ( 'NONE',  ( 20.81740448125679777, -285.4969349091684307, -225.2734980637052331 ) ) ;
#24536 = CARTESIAN_POINT ( 'NONE',  ( -57.51819236527136070, -286.9910491959993237, -199.7388187287961330 ) ) ;
#24537 = CARTESIAN_POINT ( 'NONE',  ( -106.8136892883353255, -276.1835217533882769, -298.6213969685122152 ) ) ;
#24538 = CARTESIAN_POINT ( 'NONE',  ( -40.32802213787891787, -287.4889509649636921, -346.5155259750058008 ) ) ;
#24539 = CARTESIAN_POINT ( 'NONE',  ( 36.58114696559802326, -289.3887213930033226, -257.6202747898179837 ) ) ;
#24540 = CARTESIAN_POINT ( 'NONE',  ( 6.495896134586307546, -284.6456944002850946, -209.2372416867640652 ) ) ;
#24541 = CARTESIAN_POINT ( 'NONE',  ( 30.55714785602117445, -282.8597281753982315, -297.8047855580255145 ) ) ;
#24542 = CARTESIAN_POINT ( 'NONE',  ( -99.15803628324634644, -291.9737445070194894, -313.1252269025443411 ) ) ;
#24543 = CARTESIAN_POINT ( 'NONE',  ( 196.1963538710216994, 282.2246705312485915, 13.99999999999999112 ) ) ;
#24544 = DIRECTION ( 'NONE',  ( 0.9531768234071952284, -0.3024135303179549261, 4.196830803964638850E-15 ) ) ;
#24545 = CARTESIAN_POINT ( 'NONE',  ( -110.8786663535923083, -298.6936564199741042, -252.9936541290678349 ) ) ;
#24546 = CARTESIAN_POINT ( 'NONE',  ( 32.13316527907110043, -280.4436783253834164, -247.2700698265574886 ) ) ;
#24547 = CARTESIAN_POINT ( 'NONE',  ( 21.25411053094429903, -278.9083044033890246, -223.5473205831814880 ) ) ;
#24548 = CARTESIAN_POINT ( 'NONE',  ( 26.37212219009155589, -293.3164081720143486, -313.3111781230853126 ) ) ;
#24549 = CARTESIAN_POINT ( 'NONE',  ( 9.587225927570816708, -297.0490521422769916, -196.5741556780902215 ) ) ;
#24550 = CARTESIAN_POINT ( 'NONE',  ( 36.01310505052974520, -280.1779110972923377, -265.8537868321519682 ) ) ;
#24551 = CARTESIAN_POINT ( 'NONE',  ( -13.34385970498185259, -274.8180445878520004, -340.8810177047741377 ) ) ;
#24552 = CARTESIAN_POINT ( 'NONE',  ( -67.48224483111712857, -296.7711727344507722, -337.4032003638750439 ) ) ;
#24553 = CARTESIAN_POINT ( 'NONE',  ( 207.5150553188103970, 0.03396820302666808677, 7.457905934263069803 ) ) ;
#24554 = CARTESIAN_POINT ( 'NONE',  ( -29.13281317927075875, -296.6330465369202329, -194.0565239425416735 ) ) ;
#24555 = CARTESIAN_POINT ( 'NONE',  ( -36.31097824352795556, -293.2792988463515371, -346.3537286391017460 ) ) ;
#24556 = CARTESIAN_POINT ( 'NONE',  ( -66.81661364193982422, -293.0834491804830577, -202.9326047874012886 ) ) ;
#24557 = CARTESIAN_POINT ( 'NONE',  ( 129.4467878515196162, -299.5541904835127980, -190.0176033293537898 ) ) ;
#24558 = CARTESIAN_POINT ( 'NONE',  ( 11.02992459476434028, -293.5446221723825033, -215.4046588239223468 ) ) ;
#24559 = CARTESIAN_POINT ( 'NONE',  ( 194.3594942055387094, 21.00000000000000000, 14.50689422379897842 ) ) ;
#24561 = CARTESIAN_POINT ( 'NONE',  ( 6.062939907231674752, -294.4449065442651658, -329.1185534946128541 ) ) ;
#24560 = CARTESIAN_POINT ( 'NONE',  ( -58.05927619379656335, -281.3384801012228991, -342.8667221965002341 ) ) ;
#24562 = CARTESIAN_POINT ( 'NONE',  ( -8.038885970795169200, -282.6789022912734026, -341.6240128786796504 ) ) ;
#24563 = CARTESIAN_POINT ( 'NONE',  ( 19.03761677933281504, -282.7770412960509248, -220.0357383591631049 ) ) ;
#24564 = CARTESIAN_POINT ( 'NONE',  ( -52.16505365360909963, -285.5342244219547183, -194.7685909183345245 ) ) ;
#24565 = CARTESIAN_POINT ( 'NONE',  ( -64.71919363270384906, -289.6937010159547299, -200.7017069746852087 ) ) ;
#24566 = CARTESIAN_POINT ( 'NONE',  ( 35.80842208123374348, -280.3090922232262869, -292.2629399496255473 ) ) ;
#24567 = CARTESIAN_POINT ( 'NONE',  ( 25.38025973573533278, -285.7127907578231429, -232.0570812730936439 ) ) ;
#24568 = CARTESIAN_POINT ( 'NONE',  ( 39.26965611062281880, -286.4158415773543993, -265.8503387409493826 ) ) ;
#24569 = FACE_OUTER_BOUND ( 'NONE', #90079, .T. ) ;
#24570 = CARTESIAN_POINT ( 'NONE',  ( -26.06528609325096468, -296.5063184386654598, -343.2945321364114193 ) ) ;
#24571 = CARTESIAN_POINT ( 'NONE',  ( 25.59198146615417713, -277.5549636584964333, -313.7881398116021501 ) ) ;
#24573 = CARTESIAN_POINT ( 'NONE',  ( -92.22152547547872814, -278.9063934019443423, -222.1726860815573446 ) ) ;
#24572 = CARTESIAN_POINT ( 'NONE',  ( 21.86339244963379613, -292.2095380956092185, -316.9990176015705856 ) ) ;
#24574 = CARTESIAN_POINT ( 'NONE',  ( 26.49171239844626058, -293.1503722954759041, -227.2057967811639685 ) ) ;
#24575 = CARTESIAN_POINT ( 'NONE',  ( -51.87196184432060875, -283.9476069036426225, -196.1579966918416176 ) ) ;
#24576 = CARTESIAN_POINT ( 'NONE',  ( -105.7413767529537125, -280.1474408796800617, -301.2523875054291125 ) ) ;
#24577 = CARTESIAN_POINT ( 'NONE',  ( -35.65718105549627381, -294.0892826962033837, -343.5895738469998264 ) ) ;
#24578 = VECTOR ( 'NONE', #79317, 1000.000000000000000 ) ;
#24579 = CARTESIAN_POINT ( 'NONE',  ( -112.5074205632657680, -270.5881751876177077, -267.5365165288932303 ) ) ;
#24580 = ORIENTED_EDGE ( 'NONE', *, *, #82014, .T. ) ;
#24581 = DIRECTION ( 'NONE',  ( 0.000000000000000000, 1.000000000000000000, 0.000000000000000000 ) ) ;
#24583 = CARTESIAN_POINT ( 'NONE',  ( 36.98776750836832150, -283.4366165086683509, -262.9638254481876629 ) ) ;
#24582 = AXIS2_PLACEMENT_3D ( 'NONE', #31867, #38947, #45575 ) ;
#24584 = CARTESIAN_POINT ( 'NONE',  ( 35.70320008909624931, -293.1011457798167044, -273.4978605523300530 ) ) ;
#24585 = CARTESIAN_POINT ( 'NONE',  ( 152.4536156746142410, 275.5000000000000568, -12.49999999999999289 ) ) ;
#24586 = CARTESIAN_POINT ( 'NONE',  ( -106.6379572354042296, -276.4809262143061233, -236.9535640164627353 ) ) ;
#24587 = CARTESIAN_POINT ( 'NONE',  ( -75.65204922944118948, -296.6130805981129015, -203.7784113293825783 ) ) ;
#24588 = PRESENTATION_LAYER_ASSIGNMENT (  '', '', ( #88040 ) ) ;
#24589 = CARTESIAN_POINT ( 'NONE',  ( -7.099350016895198401, -289.9787925258967789, -340.6511430220568855 ) ) ;
#24590 = CARTESIAN_POINT ( 'NONE',  ( -39.96017090122298754, -288.9191555172766357, -343.3637195597975165 ) ) ;
#24591 = CIRCLE ( 'NONE', #29137, 12.68950434577434372 ) ;
#24592 = CARTESIAN_POINT ( 'NONE',  ( -77.21310500659924969, -281.0275136554026858, -208.3246462274228179 ) ) ;
#24593 = CARTESIAN_POINT ( 'NONE',  ( -52.86925619265425524, -299.6107202394247224, -197.9422947700795419 ) ) ;
#24594 = CARTESIAN_POINT ( 'NONE',  ( 11.58184918567872934, -279.5441974790371660, -215.6471633970384403 ) ) ;
#24595 = ORIENTED_EDGE ( 'NONE', *, *, #42879, .F. ) ;
#24596 = CARTESIAN_POINT ( 'NONE',  ( -82.95463243587803959, -297.1140705064888152, -208.2851764265907661 ) ) ;
#24597 = CARTESIAN_POINT ( 'NONE',  ( -37.57860526581393401, -293.9693526765320826, -195.9088021524900967 ) ) ;
#24598 = CARTESIAN_POINT ( 'NONE',  ( 27.36216727695034123, -294.6190993635756854, -230.0140987193239823 ) ) ;
#24599 = DIRECTION ( 'NONE',  ( 0.8457827187922972723, 0.5335274993777825436, 0.000000000000000000 ) ) ;
#24600 = ADVANCED_FACE ( 'NONE', ( #21068 ), #64665, .F. ) ;
#24601 = CARTESIAN_POINT ( 'NONE',  ( -109.8022962453835589, -291.3357990970879996, -260.3233275407024507 ) ) ;
#24602 = PLANE ( 'NONE',  #7363 ) ;
#24603 = ORIENTED_EDGE ( 'NONE', *, *, #31259, .T. ) ;
#24604 = CARTESIAN_POINT ( 'NONE',  ( 29.81522044529832982, -291.2305622138032390, -235.1731391212427980 ) ) ;
#24605 = CARTESIAN_POINT ( 'NONE',  ( -91.85785198755580439, -296.9133678216314820, -221.7804976360504838 ) ) ;
#24606 = PLANE ( 'NONE',  #21584 ) ;
#24607 = CARTESIAN_POINT ( 'NONE',  ( 82.64890176555634582, -299.5541904835127980, -201.5153591320744226 ) ) ;
#24608 = CARTESIAN_POINT ( 'NONE',  ( -98.46206618453928172, -291.4586878324099644, -316.0665081189857233 ) ) ;
#24609 = CARTESIAN_POINT ( 'NONE',  ( -19.05039376806008633, -291.3376638359844719, -350.3538533559490702 ) ) ;
#24610 = EDGE_CURVE ( 'NONE', #67590, #26246, #32158, .T. ) ;
#24611 = CARTESIAN_POINT ( 'NONE',  ( 29.27895320654620903, -289.0992210910067115, -236.1629728259992760 ) ) ;
#24612 = CARTESIAN_POINT ( 'NONE',  ( 21.30785965334448306, -272.9118451287024527, -223.8620334824406655 ) ) ;
#24613 = CIRCLE ( 'NONE', #11023, 1.000000000000002887 ) ;
#24614 = CARTESIAN_POINT ( 'NONE',  ( 33.90152715300260411, -277.7530413340703035, -291.9858260242482970 ) ) ;
#24615 = CARTESIAN_POINT ( 'NONE',  ( -9.160087433827399650, -290.5032175543380504, -201.4069819873276401 ) ) ;
#24616 = CARTESIAN_POINT ( 'NONE',  ( -102.3639107314247951, -280.9290740459282461, -231.3692418883667870 ) ) ;
#24617 = AXIS2_PLACEMENT_3D ( 'NONE', #65961, #22833, #86294 ) ;
#24618 = ORIENTED_EDGE ( 'NONE', *, *, #57248, .F. ) ;
#24619 = CARTESIAN_POINT ( 'NONE',  ( 21.88966573180957909, -281.4995084880939658, -313.2257261522458407 ) ) ;
#24620 = CARTESIAN_POINT ( 'NONE',  ( -113.7372913503885172, -279.7235364212798459, -263.0570966039791756 ) ) ;
#24621 = CARTESIAN_POINT ( 'NONE',  ( -7.676515842864581884, -279.2273385976901636, -199.7212150923375305 ) ) ;
#24622 = CARTESIAN_POINT ( 'NONE',  ( -99.49319086193513328, -245.9241049507712944, -331.6501179397317856 ) ) ;
#24623 = CARTESIAN_POINT ( 'NONE',  ( 32.33444253264642754, -276.0784942870038776, -238.0157100554245346 ) ) ;
#24624 = PRODUCT_CONTEXT ( 'NONE', #51103, 'mechanical' ) ;
#24625 = CARTESIAN_POINT ( 'NONE',  ( -44.00171313750067270, -275.4896595126563170, -194.2928172073101507 ) ) ;
#24626 = CARTESIAN_POINT ( 'NONE',  ( -105.5937364680635966, -275.2662352645559167, -254.8156830097664738 ) ) ;
#24627 = ORIENTED_EDGE ( 'NONE', *, *, #90853, .T. ) ;
#24628 = ORIENTED_EDGE ( 'NONE', *, *, #2847, .T. ) ;
#24629 = CARTESIAN_POINT ( 'NONE',  ( -108.9617681973237495, -291.4255923004792521, -286.0652506203121561 ) ) ;
#24630 = CARTESIAN_POINT ( 'NONE',  ( -77.58053063487280099, -291.3440424408815943, -334.8803065604809603 ) ) ;
#24631 = CARTESIAN_POINT ( 'NONE',  ( -1.199071721370169818, -291.8938201952680629, -206.8044854357036684 ) ) ;
#24632 = CARTESIAN_POINT ( 'NONE',  ( -32.30418216715476376, -285.6217007416620390, -193.5745924145047638 ) ) ;
#24633 = CARTESIAN_POINT ( 'NONE',  ( 197.9931848604286699, 24.71549707027390141, 9.866139269184797556 ) ) ;
#24634 = CARTESIAN_POINT ( 'NONE',  ( -10.70584541269387024, -281.0988842540961627, -339.2409398415281885 ) ) ;
#24635 = CARTESIAN_POINT ( 'NONE',  ( 36.86581336776923479, -289.4571033280300867, -273.7937109067386245 ) ) ;
#24636 = CARTESIAN_POINT ( 'NONE',  ( -66.85485465257420401, -281.9259172915008094, -337.9002333368860604 ) ) ;
#24637 = CARTESIAN_POINT ( 'NONE',  ( -30.23123201532474269, -281.4590228184221701, -197.1620481356565335 ) ) ;
#24638 = CARTESIAN_POINT ( 'NONE',  ( 28.70741423731568887, -289.0046157197702996, -309.4806106176583853 ) ) ;
#24639 = CARTESIAN_POINT ( 'NONE',  ( -109.3456620402249655, -278.8802702776321212, -282.8212280258921965 ) ) ;
#24640 = CARTESIAN_POINT ( 'NONE',  ( -40.60009124559083915, -290.8069889156782892, -193.8144057646714487 ) ) ;
#24641 = CARTESIAN_POINT ( 'NONE',  ( -29.48962446833598605, -286.9520443329085992, -193.9248456496801509 ) ) ;
#24642 = CARTESIAN_POINT ( 'NONE',  ( 0.2482447686448989166, -287.0312046141614246, -203.2154420724936870 ) ) ;
#24643 = CARTESIAN_POINT ( 'NONE',  ( -71.40699958686073501, -283.6819946062201439, -334.9254686515454296 ) ) ;
#24644 = ORIENTED_EDGE ( 'NONE', *, *, #1109, .F. ) ;
#24645 = CARTESIAN_POINT ( 'NONE',  ( 195.4781563537916895, 27.48493576247233605, 14.00000000000009059 ) ) ;
#24646 = CARTESIAN_POINT ( 'NONE',  ( 26.99081124158175271, -294.8793449712281358, -230.2416215306612060 ) ) ;
#24647 = CIRCLE ( 'NONE', #15597, 25.00000000000000000 ) ;
#24648 = CARTESIAN_POINT ( 'NONE',  ( 26.09342928666886507, -292.8041494067347799, -313.1312317169473545 ) ) ;
#24649 = CARTESIAN_POINT ( 'NONE',  ( -13.72081148633105485, -275.7967889308401936, -339.7358635659010133 ) ) ;
#24650 = CARTESIAN_POINT ( 'NONE',  ( -114.0184817785825402, -295.9820185349875601, -263.8707921404442800 ) ) ;
#24651 = CARTESIAN_POINT ( 'NONE',  ( 26.84790489709978090, -291.5399732465593274, -234.0573965944853967 ) ) ;
#24652 = CARTESIAN_POINT ( 'NONE',  ( -83.00233680404967629, -293.9262702997888255, -328.6766287563607989 ) ) ;
#24653 = AXIS2_PLACEMENT_3D ( 'NONE', #59391, #80223, #15837 ) ;
#24654 = CARTESIAN_POINT ( 'NONE',  ( -88.21682213208633527, -292.5258575990554846, -217.3866826588239292 ) ) ;
#24655 = CARTESIAN_POINT ( 'NONE',  ( 9.033799285774296806, -293.7854244400997459, -213.5190648787922498 ) ) ;
#24656 = CARTESIAN_POINT ( 'NONE',  ( 113.5000000000000568, -190.7866584945343504, -447.4016117689005796 ) ) ;
#24657 = AXIS2_PLACEMENT_3D ( 'NONE', #56943, #57854, #86240 ) ;
#24658 = CARTESIAN_POINT ( 'NONE',  ( 23.38962777864315967, -292.1544723382924644, -314.6742588820691822 ) ) ;
#24659 = CARTESIAN_POINT ( 'NONE',  ( -68.01896229583030618, -299.6495877868003959, -201.9082930060563399 ) ) ;
#24660 = CARTESIAN_POINT ( 'NONE',  ( 30.17405039579361414, -288.1123394274220004, -241.8567563461324994 ) ) ;
#24661 = AXIS2_PLACEMENT_3D ( 'NONE', #74732, #9853, #80894 ) ;
#24662 = CIRCLE ( 'NONE', #77595, 0.5000000000000004441 ) ;
#24663 = CARTESIAN_POINT ( 'NONE',  ( 13.78611618818857920, -278.3199921446559415, -325.7887594672816363 ) ) ;
#24664 = CARTESIAN_POINT ( 'NONE',  ( -77.61924689351975815, -276.3746041638488009, -335.5820165320601518 ) ) ;
#24665 = CARTESIAN_POINT ( 'NONE',  ( 2.372469025667470977, -273.9182881610584559, -204.5120666990251266 ) ) ;
#24666 = CARTESIAN_POINT ( 'NONE',  ( 34.12377414469617776, -279.3617425428742536, -249.5284468617801110 ) ) ;
#24667 = CARTESIAN_POINT ( 'NONE',  ( -34.34318743514187844, -275.4149186839528625, -346.5021012867172772 ) ) ;
#24668 = CIRCLE ( 'NONE', #8045, 8.000000000000000000 ) ;
#24669 = CARTESIAN_POINT ( 'NONE',  ( -104.1600173013224406, -295.6483961627992585, -239.6354866054246031 ) ) ;
#24670 = CARTESIAN_POINT ( 'NONE',  ( -98.13078375598314551, -275.1513935303307790, -226.3472614259501370 ) ) ;
#24671 = CARTESIAN_POINT ( 'NONE',  ( -110.2911103016980974, -273.2753242531903766, -264.9141075488202546 ) ) ;
#24672 = DIRECTION ( 'NONE',  ( 0.4878460013594530520, 0.3579938043661777813, 0.7961449082880726058 ) ) ;
#24674 = CARTESIAN_POINT ( 'NONE',  ( -67.05556151812045584, -273.4848093309479395, -203.6684447092223706 ) ) ;
#24673 = CARTESIAN_POINT ( 'NONE',  ( 21.97675669281675681, -286.2072483374698777, -316.8547550167892837 ) ) ;
#24675 = TOROIDAL_SURFACE ( 'NONE', #26167, 4.500000000000002665, 0.5000000000000000000 ) ;
#24676 = CARTESIAN_POINT ( 'NONE',  ( 22.40514260695364612, -288.2040103912519271, -318.9546470363817434 ) ) ;
#24677 = CARTESIAN_POINT ( 'NONE',  ( -29.30464945192607118, -300.1321733035788384, -195.0032134068150924 ) ) ;
#24678 = CARTESIAN_POINT ( 'NONE',  ( -85.68131689089572944, -293.7223037606157732, -327.5545620920422607 ) ) ;
#24679 = CARTESIAN_POINT ( 'NONE',  ( -8.109806667749035469, -281.8761993355265645, -341.4784609991933735 ) ) ;
#24680 = CARTESIAN_POINT ( 'NONE',  ( 199.7657144415678658, 41.62711076580291092, 9.999999999999998224 ) ) ;
#24681 = CARTESIAN_POINT ( 'NONE',  ( 26.99074920872491035, -279.0346744736479536, -231.7090789594859928 ) ) ;
#24682 = AXIS2_PLACEMENT_3D ( 'NONE', #88037, #46353, #75254 ) ;
#24683 = CARTESIAN_POINT ( 'NONE',  ( 195.2403266774578583, 20.74618149458048677, -13.25394924001932395 ) ) ;
#24684 = CARTESIAN_POINT ( 'NONE',  ( -90.09108366828415626, -290.0806083982209884, -219.3255123637784436 ) ) ;
#24685 = CARTESIAN_POINT ( 'NONE',  ( -61.96643003605396416, -281.5151343531188104, -340.4473132351998856 ) ) ;
#24686 = CYLINDRICAL_SURFACE ( 'NONE', #13950, 0.5000000000000004441 ) ;
#24687 = LINE ( 'NONE', #68244, #4996 ) ;
#24688 = CARTESIAN_POINT ( 'NONE',  ( -44.46549000037443733, -289.9619948488783621, -195.6479934131428990 ) ) ;
#24689 = CARTESIAN_POINT ( 'NONE',  ( -31.65039828229472008, -284.1869162433017664, -346.7655330158929132 ) ) ;
#24690 = ADVANCED_FACE ( 'NONE', ( #72209 ), #16745, .T. ) ;
#24692 = CARTESIAN_POINT ( 'NONE',  ( -100.4011321051475960, -284.0474123027393603, -307.1375783713706937 ) ) ;
#24691 = CARTESIAN_POINT ( 'NONE',  ( -84.88288915655664368, -271.4821042943038947, -211.6316573950390136 ) ) ;
#24693 = CARTESIAN_POINT ( 'NONE',  ( -7.250236046530583067, -278.0747882380499618, -337.5167484837006100 ) ) ;
#24694 = CARTESIAN_POINT ( 'NONE',  ( 7.687807447843035824, -277.2224869954009705, -328.0880169124400254 ) ) ;
#24695 = CARTESIAN_POINT ( 'NONE',  ( -55.20060866118232923, -285.2820377749279714, -343.2038254532953374 ) ) ;
#24696 = ORIENTED_EDGE ( 'NONE', *, *, #40031, .T. ) ;
#24697 = CARTESIAN_POINT ( 'NONE',  ( 203.1043581768557544, 295.9636489450775798, -54.00000000006133405 ) ) ;
#24698 = CARTESIAN_POINT ( 'NONE',  ( 38.60593156927643577, -293.5451389178173827, -283.1278884188774327 ) ) ;
#24699 = CARTESIAN_POINT ( 'NONE',  ( 3.322402274760987595, -288.5815596977761288, -207.7649713208833475 ) ) ;
#24700 = DIRECTION ( 'NONE',  ( 0.000000000000000000, 0.000000000000000000, -1.000000000000000000 ) ) ;
#24701 = CARTESIAN_POINT ( 'NONE',  ( 13.84574458161073807, -284.1952119285919025, -206.2264541496106460 ) ) ;
#24702 = CARTESIAN_POINT ( 'NONE',  ( -86.99864850041942077, -276.9200021584703677, -329.0681572795440957 ) ) ;
#24703 = CARTESIAN_POINT ( 'NONE',  ( -7.484683838391472221, -290.8369859948538760, -200.2398893648420710 ) ) ;
#24704 = CARTESIAN_POINT ( 'NONE',  ( -110.9217803883156819, -286.1366146450784527, -265.4379918796040556 ) ) ;
#24705 = CARTESIAN_POINT ( 'NONE',  ( -73.31518544651441971, -279.2962498162957559, -335.0586344776193641 ) ) ;
#24706 = CARTESIAN_POINT ( 'NONE',  ( -15.59863551311802610, -287.7532810431171129, -197.0542228195056111 ) ) ;
#24707 = CARTESIAN_POINT ( 'NONE',  ( 36.45789534525945186, -283.7248411253985978, -283.7981066141067004 ) ) ;
#24708 = CARTESIAN_POINT ( 'NONE',  ( 39.38068138450685751, -275.8005322072798435, -276.8938187662205905 ) ) ;
#24709 = CARTESIAN_POINT ( 'NONE',  ( -38.54708760552509261, -276.9001963808065057, -347.3516826353862257 ) ) ;
#24711 = CARTESIAN_POINT ( 'NONE',  ( -52.96063129269486325, -299.7707073268676368, -197.5252189089472949 ) ) ;
#24710 = AXIS2_PLACEMENT_3D ( 'NONE', #38633, #67536, #46195 ) ;
#24712 = CARTESIAN_POINT ( 'NONE',  ( 152.4536156746142410, 249.5000000000000568, -14.50000000000000000 ) ) ;
#24713 = EDGE_CURVE ( 'NONE', #50286, #21852, #45606, .T. ) ;
#24714 = FACE_OUTER_BOUND ( 'NONE', #77969, .T. ) ;
#24715 = CARTESIAN_POINT ( 'NONE',  ( -108.2132656303867861, -271.1454827044902913, -242.8084543558544794 ) ) ;
#24717 = VECTOR ( 'NONE', #77795, 1000.000000000000000 ) ;
#24716 = DIRECTION ( 'NONE',  ( 1.000000000000000000, -2.081668171172166620E-14, 0.000000000000000000 ) ) ;
#24718 = CARTESIAN_POINT ( 'NONE',  ( -97.70320141073408138, -277.4875943931880329, -311.5251508827892053 ) ) ;
#24719 = AXIS2_PLACEMENT_3D ( 'NONE', #52941, #58675, #80428 ) ;
#24720 = CARTESIAN_POINT ( 'NONE',  ( -89.90163341199982483, -274.5351346334454092, -214.5619929788704496 ) ) ;
#24721 = CARTESIAN_POINT ( 'NONE',  ( 6.779942849266836546, -281.5271455299173340, -333.2441099510151616 ) ) ;
#24722 = CARTESIAN_POINT ( 'NONE',  ( 24.36670301475287914, -288.7519450447548479, -229.4021613922488143 ) ) ;
#24723 = CARTESIAN_POINT ( 'NONE',  ( -70.48902961859327831, -297.0012595590896467, -339.1065829002527039 ) ) ;
#24724 = CARTESIAN_POINT ( 'NONE',  ( -55.95885352305629823, -296.4918233717499447, -344.6673109744356793 ) ) ;
#24725 = ADVANCED_FACE ( 'NONE', ( #46087 ), #37137, .F. ) ;
#24726 = CARTESIAN_POINT ( 'NONE',  ( -27.89965840075808856, -294.1723383278712731, -196.0738197769975955 ) ) ;
#24727 = CARTESIAN_POINT ( 'NONE',  ( 24.07521869012099103, -280.1333512510219066, -313.1161236590361341 ) ) ;
#24728 = CIRCLE ( 'NONE', #39831, 7.999911143031724237 ) ;
#24729 = CARTESIAN_POINT ( 'NONE',  ( 22.47172739582896028, -282.8627267277936994, -226.0263785211912193 ) ) ;
#24730 = CARTESIAN_POINT ( 'NONE',  ( -34.38433971069755302, -296.1692984879676374, -195.9220866594944539 ) ) ;
#24731 = CARTESIAN_POINT ( 'NONE',  ( -93.79265034225470288, -285.4494499547828923, -321.5637684949475670 ) ) ;
#24732 = CARTESIAN_POINT ( 'NONE',  ( 35.26461582477514156, -286.6066990631442764, -280.5790391357471663 ) ) ;
#24733 = CARTESIAN_POINT ( 'NONE',  ( 39.51766203301180269, -280.9312901576506647, -272.8006331946813816 ) ) ;
#24734 = CARTESIAN_POINT ( 'NONE',  ( -108.2955140824691966, -267.5841981642410587, -306.8676081293918401 ) ) ;
#24735 = VERTEX_POINT ( 'NONE', #22921 ) ;
#24736 = CARTESIAN_POINT ( 'NONE',  ( 27.67890005352342442, -286.7661549129841205, -237.0169700876838306 ) ) ;
#24737 = ORIENTED_EDGE ( 'NONE', *, *, #82544, .F. ) ;
#24738 = CARTESIAN_POINT ( 'NONE',  ( -112.8302213716410733, -285.4583078628263024, -284.1792582437713577 ) ) ;
#24739 = AXIS2_PLACEMENT_3D ( 'NONE', #89046, #1966, #23276 ) ;
#24740 = CARTESIAN_POINT ( 'NONE',  ( 23.80888718822457761, -275.3325797938629194, -230.4525580281294879 ) ) ;
#24741 = EDGE_CURVE ( 'NONE', #41734, #17649, #85076, .T. ) ;
#24742 = CARTESIAN_POINT ( 'NONE',  ( -30.71023853656152625, -291.0543217285215292, -193.9049313277316173 ) ) ;
#24743 = CARTESIAN_POINT ( 'NONE',  ( 30.50821717850518411, -282.0270354583017820, -234.3422695862232672 ) ) ;
#24744 =( NAMED_UNIT ( * ) SI_UNIT ( $, .STERADIAN. ) SOLID_ANGLE_UNIT ( ) );
#24745 = CARTESIAN_POINT ( 'NONE',  ( -113.6845556014832113, -280.0923757939359007, -268.7682134599471624 ) ) ;
#24746 = CARTESIAN_POINT ( 'NONE',  ( 38.64765668490923645, -282.0403696980138193, -282.7464096631624102 ) ) ;
#24747 = CARTESIAN_POINT ( 'NONE',  ( 27.36219212280433055, -278.6237833571632905, -239.2376011013261916 ) ) ;
#24748 = ORIENTED_EDGE ( 'NONE', *, *, #22475, .F. ) ;
#24749 = CARTESIAN_POINT ( 'NONE',  ( 15.03218479280689834, -278.3119622110595515, -323.8842667980499073 ) ) ;
#24750 = CARTESIAN_POINT ( 'NONE',  ( 102.2689123659984034, 116.6942946837412904, -282.5096189404233655 ) ) ;
#24751 = AXIS2_PLACEMENT_3D ( 'NONE', #54960, #46899, #83836 ) ;
#24752 = CARTESIAN_POINT ( 'NONE',  ( 21.46146779988145070, -280.2061079429810775, -316.3397461528052759 ) ) ;
#24753 = CARTESIAN_POINT ( 'NONE',  ( -91.91547213405215189, -296.5952871747879840, -221.7237241646326140 ) ) ;
#24754 = CARTESIAN_POINT ( 'NONE',  ( -64.36131451514656021, -291.2166054553856611, -198.2670341956799405 ) ) ;
#24755 = CARTESIAN_POINT ( 'NONE',  ( -93.16763214117450786, -239.2410508537212479, -338.7284373407174485 ) ) ;
#24757 = CARTESIAN_POINT ( 'NONE',  ( 35.79172722745686031, -285.8180008757970541, -260.0905191214313277 ) ) ;
#24756 = CARTESIAN_POINT ( 'NONE',  ( -113.8485494440449344, -271.2371898177336789, -270.3444098319821478 ) ) ;
#24758 = CARTESIAN_POINT ( 'NONE',  ( 19.79877908200473158, -296.0734828437670103, -317.7513186455097411 ) ) ;
#24759 = CARTESIAN_POINT ( 'NONE',  ( -46.80485354134612663, -287.2448096449472246, -197.4286417822142141 ) ) ;
#24760 = CARTESIAN_POINT ( 'NONE',  ( 33.10370670208148169, -294.1035359169013645, -239.8608742318608904 ) ) ;
#24761 = CARTESIAN_POINT ( 'NONE',  ( -109.2547132966462300, -285.2155080094811410, -257.3869451307647296 ) ) ;
#24762 = CARTESIAN_POINT ( 'NONE',  ( -91.34467392772278060, -296.0992853403963068, -216.0316826934763696 ) ) ;
#24763 = CIRCLE ( 'NONE', #83748, 35.00000000000002842 ) ;
#24764 = CARTESIAN_POINT ( 'NONE',  ( -66.96266101010263583, -292.4764972171892055, -199.4614882434732408 ) ) ;
#24765 = CARTESIAN_POINT ( 'NONE',  ( -99.15889336971451939, -291.6541544114275553, -224.5333525818493854 ) ) ;
#24766 = CARTESIAN_POINT ( 'NONE',  ( -92.41032733737503690, -290.0348817327506481, -318.3579071300750911 ) ) ;
#24767 = ORIENTED_EDGE ( 'NONE', *, *, #77420, .T. ) ;
#24768 = CARTESIAN_POINT ( 'NONE',  ( -54.94434090351493438, -285.8906705383787994, 74.50000000000001421 ) ) ;
#24769 = CARTESIAN_POINT ( 'NONE',  ( -30.64497133874975887, -299.9955475955708266, -194.5942148631571911 ) ) ;
#24770 = CARTESIAN_POINT ( 'NONE',  ( -102.3738020741164974, -271.8794524224558700, -229.8785978720527794 ) ) ;
#24771 = CARTESIAN_POINT ( 'NONE',  ( -33.49581723156373414, -282.0613352617378951, -343.5079750332141657 ) ) ;
#24772 = ORIENTED_EDGE ( 'NONE', *, *, #68252, .T. ) ;
#24773 = CARTESIAN_POINT ( 'NONE',  ( 14.83683626251947629, -275.8481508193265199, -326.9749998273502456 ) ) ;
#24774 = CARTESIAN_POINT ( 'NONE',  ( -63.57222284943809854, -272.1043744524579324, -201.3663207359703051 ) ) ;
#24775 = CARTESIAN_POINT ( 'NONE',  ( -111.1290831280714997, -280.3010797114725960, -278.9559624860719396 ) ) ;
#24776 = CARTESIAN_POINT ( 'NONE',  ( -59.58733595899182234, -275.4829164708435769, -341.1848228058550490 ) ) ;
#24777 = CARTESIAN_POINT ( 'NONE',  ( -97.21549071196594127, -298.3467972376506623, -227.9080885675479351 ) ) ;
#24778 = CARTESIAN_POINT ( 'NONE',  ( -35.14987133282090781, -299.1598973309951930, -197.0515897046275597 ) ) ;
#24779 = CARTESIAN_POINT ( 'NONE',  ( -57.20106889814263695, -299.4003444165638257, -196.7398013132968515 ) ) ;
#24780 = CONICAL_SURFACE ( 'NONE', #23279, 4.025000000000000355, 0.7853981633973095011 ) ;
#24781 = CARTESIAN_POINT ( 'NONE',  ( -52.19617784265596327, -271.8831326211135320, -196.4312485482143131 ) ) ;
#24782 = CARTESIAN_POINT ( 'NONE',  ( -3.088661111480113242, -295.2383532001938420, -334.9414709280356988 ) ) ;
#24783 = CARTESIAN_POINT ( 'NONE',  ( -52.47334284020257655, -290.4293969061633334, -198.2920786537152367 ) ) ;
#24784 = CARTESIAN_POINT ( 'NONE',  ( -23.68628624284178130, -43.55766379199612004, -22.50000000000000000 ) ) ;
#24785 = CARTESIAN_POINT ( 'NONE',  ( 35.14510787699352790, -276.3720347211612989, -296.3094594296013611 ) ) ;
#24786 = CARTESIAN_POINT ( 'NONE',  ( -94.61403151622704399, -273.3575791947326934, -225.0965616287649027 ) ) ;
#24787 = CARTESIAN_POINT ( 'NONE',  ( 26.30229587354784115, -280.7994768393588743, -312.8198043207306114 ) ) ;
#24788 = CARTESIAN_POINT ( 'NONE',  ( -89.01556573898155023, -282.9983167109281794, -322.2242568858924869 ) ) ;
#24789 = CARTESIAN_POINT ( 'NONE',  ( -80.52953097775892388, -281.6355078514125125, -331.9455044203337479 ) ) ;
#24790 = CARTESIAN_POINT ( 'NONE',  ( -13.61243191700118338, -275.3128466127583351, -340.0731082936654275 ) ) ;
#24791 = CARTESIAN_POINT ( 'NONE',  ( 34.72565397882270588, -283.2828882598632845, -249.4124285421488594 ) ) ;
#24792 = CARTESIAN_POINT ( 'NONE',  ( 165.2494399300530290, 8.542400036368780647, 9.000000000000001776 ) ) ;
#24793 = DIRECTION ( 'NONE',  ( 0.000000000000000000, 1.000000000000000000, 0.000000000000000000 ) ) ;
#24794 = CARTESIAN_POINT ( 'NONE',  ( 2.022358464303719572, -272.9697259977997987, -205.1161081648782272 ) ) ;
#24795 = AXIS2_PLACEMENT_3D ( 'NONE', #83095, #46641, #61365 ) ;
#24796 = CARTESIAN_POINT ( 'NONE',  ( -83.71482780785348154, -279.6866015602371931, -329.5843295770815757 ) ) ;
#24797 = CARTESIAN_POINT ( 'NONE',  ( 209.8744251295252354, 28.03846817292548366, 12.09245862095555601 ) ) ;
#24798 = CARTESIAN_POINT ( 'NONE',  ( -89.42746297630637287, -285.6986192407990757, -325.1721046157323940 ) ) ;
#24799 = VECTOR ( 'NONE', #18488, 1000.000000000000000 ) ;
#24800 = CARTESIAN_POINT ( 'NONE',  ( 203.5977283565847529, 62.01285785379746329, 9.999999999999994671 ) ) ;
#24801 = CARTESIAN_POINT ( 'NONE',  ( -95.30663867216682661, -289.2084413559330187, -222.7486473314181978 ) ) ;
#24802 = CYLINDRICAL_SURFACE ( 'NONE', #39170, 3.000000000000004885 ) ;
#24803 = CARTESIAN_POINT ( 'NONE',  ( -107.0792717806403687, -295.6510953555426795, -247.3133846204875965 ) ) ;
#24804 = CARTESIAN_POINT ( 'NONE',  ( -74.17813100531300563, -287.6867868296533288, -334.8268643047002797 ) ) ;
#24805 = CARTESIAN_POINT ( 'NONE',  ( -106.3535322092011199, -272.9508360837029954, -295.9465859460973434 ) ) ;
#24806 = CARTESIAN_POINT ( 'NONE',  ( -85.33565360227775898, -295.3892637509222823, -212.6601712253174412 ) ) ;
#24807 = CARTESIAN_POINT ( 'NONE',  ( 38.29065932756787305, -285.9042940975855913, -260.2391638466600057 ) ) ;
#24808 = CARTESIAN_POINT ( 'NONE',  ( 35.35161745895025120, -282.9861394521215630, -257.6284044288957489 ) ) ;
#24809 = CARTESIAN_POINT ( 'NONE',  ( -4.620765952321999492, -280.8668921021031224, -338.9561290907877833 ) ) ;
#24810 = CARTESIAN_POINT ( 'NONE',  ( -26.47488923120474169, -288.9101573243335679, -342.5988172604406259 ) ) ;
#24811 = AXIS2_PLACEMENT_3D ( 'NONE', #54371, #33068, #26440 ) ;
#24812 = CIRCLE ( 'NONE', #91292, 24.00000000000000355 ) ;
#24813 = CARTESIAN_POINT ( 'NONE',  ( 34.81198186798426519, -283.1675409127749390, -284.8890862866510361 ) ) ;
#24814 = CARTESIAN_POINT ( 'NONE',  ( 29.46607840130818801, -282.7571512697327876, -300.3070568979467794 ) ) ;
#24815 = CARTESIAN_POINT ( 'NONE',  ( 22.84406396344988721, -290.1489792104142680, -315.7051430209286877 ) ) ;
#24816 = CARTESIAN_POINT ( 'NONE',  ( -73.28251617260180240, -297.7559995935917527, -202.2048575721676400 ) ) ;
#24817 = CIRCLE ( 'NONE', #33877, 1.000000000000000888 ) ;
#24818 = CARTESIAN_POINT ( 'NONE',  ( -70.13176940397751480, -273.6320433592557606, -200.6774046727921359 ) ) ;
#24819 = CARTESIAN_POINT ( 'NONE',  ( 11.99956529276631656, -294.7214923264852473, -214.2806834480696239 ) ) ;
#24820 = LINE ( 'NONE', #67454, #31822 ) ;
#24821 = CARTESIAN_POINT ( 'NONE',  ( -110.4542110544635705, -280.8376638359844719, -287.0812184334320705 ) ) ;
#24822 = CARTESIAN_POINT ( 'NONE',  ( 2.507451714836021139, -274.5195751377456190, -334.1567737173533033 ) ) ;
#24823 = DIRECTION ( 'NONE',  ( -0.01818181818182024526, 0.000000000000000000, -0.9998346970812742596 ) ) ;
#24824 = CARTESIAN_POINT ( 'NONE',  ( -35.82722352397853172, -296.4706921105976676, -194.1615168451946261 ) ) ;
#24825 = CARTESIAN_POINT ( 'NONE',  ( -103.5543086974015949, -291.7154037981345596, -302.9545357144925788 ) ) ;
#24826 = CARTESIAN_POINT ( 'NONE',  ( 13.57358983551266363, -274.1371493096339691, -217.9061285539933124 ) ) ;
#24827 = CARTESIAN_POINT ( 'NONE',  ( -107.2349525084756863, -292.3795863861720363, -247.0021577344368779 ) ) ;
#24828 = AXIS2_PLACEMENT_3D ( 'NONE', #84098, #26350, #11668 ) ;
#24829 = CARTESIAN_POINT ( 'NONE',  ( -89.99378689130482201, -292.2265899812234693, -219.4576190109595473 ) ) ;
#24830 = CARTESIAN_POINT ( 'NONE',  ( 1.654002269308343376, -284.2835648014221306, -333.3281206238400500 ) ) ;
#24831 = CARTESIAN_POINT ( 'NONE',  ( -61.51947899917362150, -293.1695000515571223, -197.8206200288855712 ) ) ;
#24832 = CARTESIAN_POINT ( 'NONE',  ( -69.43169095264151736, -292.9538257249130311, -200.8952238960266072 ) ) ;
#24833 = CARTESIAN_POINT ( 'NONE',  ( 34.06713222495056925, -293.5862276390502643, -285.5795208352517989 ) ) ;
#24834 = CARTESIAN_POINT ( 'NONE',  ( 37.65532829103823076, -289.5608954784788693, -271.0292302036929186 ) ) ;
#24835 = CARTESIAN_POINT ( 'NONE',  ( 34.32364353732583595, -281.3601779384821384, -242.0539507915007675 ) ) ;
#24836 = CARTESIAN_POINT ( 'NONE',  ( -113.1065001290297971, -270.6920356400427750, -270.3374835933531131 ) ) ;
#24837 = CARTESIAN_POINT ( 'NONE',  ( -110.6861932072879000, -284.0902465413399796, -293.8478397423305069 ) ) ;
#24838 = CARTESIAN_POINT ( 'NONE',  ( 29.51466977539436698, -277.9736138747033465, -303.6751993177975351 ) ) ;
#24839 = EDGE_CURVE ( 'NONE', #34882, #75628, #85143, .T. ) ;
#24840 = CARTESIAN_POINT ( 'NONE',  ( 1.721640143195543038, -284.5744438433160326, -206.3372466918966950 ) ) ;
#24841 = CARTESIAN_POINT ( 'NONE',  ( -94.29813285721857596, -276.0046491850214352, -320.3238065899197977 ) ) ;
#24842 = DIRECTION ( 'NONE',  ( 0.3529856947623295493, 0.9356287187197470656, 0.000000000000000000 ) ) ;
#24843 = CARTESIAN_POINT ( 'NONE',  ( -69.04153268970263468, -282.9883292892177451, -336.2012885968018736 ) ) ;
#24844 = CARTESIAN_POINT ( 'NONE',  ( -84.33550593962125674, -280.6271713875945579, -209.7994286087503042 ) ) ;
#24845 = CARTESIAN_POINT ( 'NONE',  ( 35.62912769290926462, -286.3081996604329333, -246.3566405324406787 ) ) ;
#24846 = CARTESIAN_POINT ( 'NONE',  ( 36.72213116950136680, -295.3172710898968489, -270.7430884814703518 ) ) ;
#24847 = CARTESIAN_POINT ( 'NONE',  ( 35.73214306658408645, -277.4266538224841838, -292.0093692451299034 ) ) ;
#24848 = CARTESIAN_POINT ( 'NONE',  ( 24.07392711949889730, -276.2567759611323481, -224.7385467734997064 ) ) ;
#24849 = CARTESIAN_POINT ( 'NONE',  ( -108.1725979723764510, -278.1517682801263049, -288.0757217756196269 ) ) ;
#24850 = CARTESIAN_POINT ( 'NONE',  ( -34.41505128678365111, -300.0890268891578216, -195.5267753367315606 ) ) ;
#24851 = CARTESIAN_POINT ( 'NONE',  ( -4.983405806014496342, -284.4789127254735490, -202.8712924513874611 ) ) ;
#24852 = CARTESIAN_POINT ( 'NONE',  ( -94.84110387253059571, -291.4692641055593185, -320.3637077735597813 ) ) ;
#24853 = CARTESIAN_POINT ( 'NONE',  ( 34.25466151595225028, -292.2647708970275175, -254.5490697432269371 ) ) ;
#24854 = VERTEX_POINT ( 'NONE', #52268 ) ;
#24855 = CARTESIAN_POINT ( 'NONE',  ( 8.865500545418697698, -292.3726991975644296, -213.7536688816939261 ) ) ;
#24856 = ORIENTED_EDGE ( 'NONE', *, *, #38856, .F. ) ;
#24857 = CARTESIAN_POINT ( 'NONE',  ( -77.96097736790834176, -290.6636822949068915, -335.4735538706531770 ) ) ;
#24858 = CARTESIAN_POINT ( 'NONE',  ( -92.29053374333041404, -279.8909286912926291, -222.1288139876928653 ) ) ;
#24859 = ADVANCED_FACE ( 'NONE', ( #58921 ), #87310, .F. ) ;
#24860 = CARTESIAN_POINT ( 'NONE',  ( -78.02678613167225308, -296.4391690474578240, -205.3517626077324678 ) ) ;
#24861 = CARTESIAN_POINT ( 'NONE',  ( 18.57639655014822821, -288.9253791339152713, -323.1482305238463937 ) ) ;
#24862 = CARTESIAN_POINT ( 'NONE',  ( 39.32676735299915549, -287.9718230239024592, -277.2669405668844433 ) ) ;
#24863 = CARTESIAN_POINT ( 'NONE',  ( -103.5064205576639580, -285.3038914751115840, -239.3492124669827774 ) ) ;
#24864 = CARTESIAN_POINT ( 'NONE',  ( -110.3352075041367044, -266.7738566106981466, -306.9872416995153230 ) ) ;
#24865 = CARTESIAN_POINT ( 'NONE',  ( -32.48651102487607290, -123.7208602147541967, -362.7017519726991850 ) ) ;
#24866 = CARTESIAN_POINT ( 'NONE',  ( 152.8736219892452084, 204.8876459940559016, -214.3033056176879825 ) ) ;
#24867 = EDGE_CURVE ( 'NONE', #8997, #19844, #36751, .T. ) ;
#24868 = CARTESIAN_POINT ( 'NONE',  ( 9.760221938220913884, -275.5811667680674191, -326.3433532371472552 ) ) ;
#24869 = CARTESIAN_POINT ( 'NONE',  ( -16.30526454057934771, -275.6942111142294038, -340.6403722902391564 ) ) ;
#24870 = CARTESIAN_POINT ( 'NONE',  ( -102.6988461933361094, -272.7511064686084410, -229.6894109900751175 ) ) ;
#24871 = CARTESIAN_POINT ( 'NONE',  ( 46.35570317780937444, 10.66898867798451711, -328.9001176944748863 ) ) ;
#24872 = CARTESIAN_POINT ( 'NONE',  ( -56.81478339010194389, -275.9828458547286800, -344.4029643667979599 ) ) ;
#24873 = ORIENTED_EDGE ( 'NONE', *, *, #42570, .F. ) ;
#24874 = CARTESIAN_POINT ( 'NONE',  ( -109.7619785483797585, -291.1767587362562608, -260.3268713466939630 ) ) ;
#24875 = CARTESIAN_POINT ( 'NONE',  ( -102.1856188433747974, -297.8964342587916008, -229.1370349007989375 ) ) ;
#24876 = CARTESIAN_POINT ( 'NONE',  ( -108.3158456690017601, -296.6648648964790027, -300.2007898421544496 ) ) ;
#24877 = CARTESIAN_POINT ( 'NONE',  ( -15.59080451184433258, -294.9295197944176721, -340.0985673028386032 ) ) ;
#24878 = ORIENTED_EDGE ( 'NONE', *, *, #23136, .F. ) ;
#24879 = AXIS2_PLACEMENT_3D ( 'NONE', #20461, #14303, #41254 ) ;
#24880 = CARTESIAN_POINT ( 'NONE',  ( -96.78070654838988673, -279.8367358613911051, -317.0121492477230163 ) ) ;
#24881 = CARTESIAN_POINT ( 'NONE',  ( 39.46730344522944023, -281.1261653167881036, -275.6629101201901904 ) ) ;
#24882 = CARTESIAN_POINT ( 'NONE',  ( -98.25810032709762254, -280.1969703194087629, -229.4859308229065391 ) ) ;
#24883 = CARTESIAN_POINT ( 'NONE',  ( -41.30882770459677999, -278.8615603419586364, -346.2571940978824045 ) ) ;
#24884 = CARTESIAN_POINT ( 'NONE',  ( -77.82106971138166784, -296.0717852092317912, -208.8442551567145529 ) ) ;
#24885 = CARTESIAN_POINT ( 'NONE',  ( 150.4957602436334696, 20.00000000000000355, -3.637614988394445081 ) ) ;
#24886 = CARTESIAN_POINT ( 'NONE',  ( -80.81767902855966668, -277.8277672775424207, -329.0027351424697599 ) ) ;
#24887 = CARTESIAN_POINT ( 'NONE',  ( -18.59927838776390274, -275.0903058786832958, -195.7885532554267058 ) ) ;
#24888 = VECTOR ( 'NONE', #55365, 1000.000000000000000 ) ;
#24889 = CARTESIAN_POINT ( 'NONE',  ( -20.62060439594502981, -287.5267595234128635, -345.0726706229452247 ) ) ;
#24890 = CARTESIAN_POINT ( 'NONE',  ( -52.17563904481882986, -275.8625448304757697, -196.7896889069208726 ) ) ;
#24891 = CARTESIAN_POINT ( 'NONE',  ( 36.66350591572529538, -274.3667745443983677, -289.3830992925116448 ) ) ;
#24892 = CARTESIAN_POINT ( 'NONE',  ( 197.3195042448029710, 214.9800000937857476, -12.43273589989834704 ) ) ;
#24893 = CARTESIAN_POINT ( 'NONE',  ( -18.44162639572057927, -287.9996593157644611, -341.0918836248139883 ) ) ;
#24894 = CARTESIAN_POINT ( 'NONE',  ( -100.9075469566849534, -284.4732473812842386, -226.9924126580549171 ) ) ;
#24895 = CARTESIAN_POINT ( 'NONE',  ( 36.43721176719488852, -279.8765894378322514, -276.8621489865867034 ) ) ;
#24897 = CARTESIAN_POINT ( 'NONE',  ( -95.22666276784291028, -283.2813603821070387, -223.5365944728001466 ) ) ;
#24896 = CARTESIAN_POINT ( 'NONE',  ( 35.06194823852340647, -280.2999618685950622, -283.5878713537687190 ) ) ;
#24898 = CARTESIAN_POINT ( 'NONE',  ( -107.9782549589254472, -292.2238796736452855, -295.7218778890996305 ) ) ;
#24899 = CARTESIAN_POINT ( 'NONE',  ( -110.6762482752506997, -279.7174939040168056, -273.3900702410109034 ) ) ;
#24900 = LINE ( 'NONE', #53780, #92639 ) ;
#24901 = CARTESIAN_POINT ( 'NONE',  ( 29.05471765238056037, -280.4434695260436570, -307.8578568709908154 ) ) ;
#24902 = CARTESIAN_POINT ( 'NONE',  ( 37.50807736187562114, -295.6230021732154114, -275.8662945541850036 ) ) ;
#24903 = CARTESIAN_POINT ( 'NONE',  ( -92.32482502241525424, -277.5193871696083647, -217.8376088618541928 ) ) ;
#24904 = CARTESIAN_POINT ( 'NONE',  ( -96.96403338409147921, -278.6135046988646877, -312.6802546109517493 ) ) ;
#24905 = CARTESIAN_POINT ( 'NONE',  ( -98.28669884495361941, -285.9536657177474126, -314.4450583561402937 ) ) ;
#24906 = CARTESIAN_POINT ( 'NONE',  ( 196.2275076780419170, 72.70431358716514580, 11.63072960017908564 ) ) ;
#24907 = CARTESIAN_POINT ( 'NONE',  ( -110.2499118893775574, -292.7261145376525064, -250.4699144322435984 ) ) ;
#24908 = CARTESIAN_POINT ( 'NONE',  ( 23.92904542599891116, -272.9641282553837982, -227.0850166246396498 ) ) ;
#24909 = CARTESIAN_POINT ( 'NONE',  ( 33.71401382126421709, -286.3753444776108950, -240.9775099686389979 ) ) ;
#24910 = CARTESIAN_POINT ( 'NONE',  ( -110.4902897636885797, -289.0846206561997747, -260.1989817374006861 ) ) ;
#24911 = CARTESIAN_POINT ( 'NONE',  ( -48.18343439338274692, -265.6649765806887444, -435.4852526219743822 ) ) ;
#24912 = CARTESIAN_POINT ( 'NONE',  ( -16.25528957513357042, -275.4587464146221691, -340.8176542087514349 ) ) ;
#24913 = CARTESIAN_POINT ( 'NONE',  ( -2.586079678399316073, -292.7269300648275134, -335.9577057709979044 ) ) ;
#24914 = CARTESIAN_POINT ( 'NONE',  ( 221.0059830678134460, 1.828427124746190957, 9.000000000000000000 ) ) ;
#24915 = CARTESIAN_POINT ( 'NONE',  ( 191.4749582765727212, -21.37379927922774314, 13.00000000000000178 ) ) ;
#24916 = CARTESIAN_POINT ( 'NONE',  ( -4.881345449857281693, -290.9517714535404025, -201.3029314322459413 ) ) ;
#24917 = CARTESIAN_POINT ( 'NONE',  ( -110.7927309066228361, -286.2524253503041791, -262.6868965602805588 ) ) ;
#24918 = CARTESIAN_POINT ( 'NONE',  ( 15.95896971949225041, -286.5495437925206943, -324.5915584081482734 ) ) ;
#24919 = EDGE_CURVE ( 'NONE', #7041, #75392, #39763, .T. ) ;
#24920 = CARTESIAN_POINT ( 'NONE',  ( -22.35745005580442069, -287.6729373325198367, -198.2612872854854231 ) ) ;
#24921 = DIRECTION ( 'NONE',  ( 0.000000000000000000, 0.000000000000000000, -1.000000000000000000 ) ) ;
#24922 = CARTESIAN_POINT ( 'NONE',  ( 21.30904977161062774, -288.9674995192254414, -314.1164188195903080 ) ) ;
#24923 = CARTESIAN_POINT ( 'NONE',  ( 36.98813944515188723, -295.6913644988241572, -282.8282327442788642 ) ) ;
#24924 = LINE ( 'NONE', #46670, #73087 ) ;
#24925 = CARTESIAN_POINT ( 'NONE',  ( 28.35009146148064829, -288.2395190693545715, -230.8558383656643684 ) ) ;
#24926 = CARTESIAN_POINT ( 'NONE',  ( -112.7953601776410721, -276.5809232829304847, -274.3685336897104321 ) ) ;
#24927 = CARTESIAN_POINT ( 'NONE',  ( -72.82716028268285413, -277.8424262843965380, -338.6877958660033983 ) ) ;
#24928 = CARTESIAN_POINT ( 'NONE',  ( 30.89622787397934900, -291.2067725280568879, -237.7910292729779087 ) ) ;
#24929 = CARTESIAN_POINT ( 'NONE',  ( -106.3453804656410995, -278.1116579412484953, -304.6496635814437468 ) ) ;
#24930 = CARTESIAN_POINT ( 'NONE',  ( -73.66891921500237572, -299.5472930436217780, -205.1523765639574890 ) ) ;
#24931 = CARTESIAN_POINT ( 'NONE',  ( -48.18343439341186496, -262.8409108322527459, -500.9583777586229871 ) ) ;
#24932 = CARTESIAN_POINT ( 'NONE',  ( -106.4302533154710915, -282.9348318877348447, -241.0425982353069116 ) ) ;
#24933 = DIRECTION ( 'NONE',  ( 0.5877852522924681411, 0.000000000000000000, -0.8090169943749512260 ) ) ;
#24934 = CARTESIAN_POINT ( 'NONE',  ( -77.03598048211077298, -275.7293076032742647, -333.1529934475112213 ) ) ;
#24935 = CARTESIAN_POINT ( 'NONE',  ( 34.68629357844553596, -279.2823340548097804, -249.4112237689645326 ) ) ;
#24936 = DIRECTION ( 'NONE',  ( -1.000000000000000000, 0.000000000000000000, 0.000000000000000000 ) ) ;
#24937 = CARTESIAN_POINT ( 'NONE',  ( -31.52263184620089120, -275.4599605900671122, -346.4977351006015738 ) ) ;
#24938 = CARTESIAN_POINT ( 'NONE',  ( -94.46783928043770118, -297.4192576053155221, -316.9353428337039418 ) ) ;
#24939 = CARTESIAN_POINT ( 'NONE',  ( -44.40449788088091765, -282.0597083655492838, -346.7792365828987613 ) ) ;
#24940 = CARTESIAN_POINT ( 'NONE',  ( -100.1046072116746330, -298.0121672199594514, -232.5235538516555209 ) ) ;
#24941 = CARTESIAN_POINT ( 'NONE',  ( -37.62276689743769253, -299.3638691411998707, -193.8547831036573541 ) ) ;
#24942 = CARTESIAN_POINT ( 'NONE',  ( 23.07221168254130461, -274.6483834088388107, -229.3234865802773754 ) ) ;
#24943 = CARTESIAN_POINT ( 'NONE',  ( 28.93712421303357374, -296.0189989757953981, -305.5737043482777153 ) ) ;
#24944 = CARTESIAN_POINT ( 'NONE',  ( 30.36370218936502496, -288.1945058792406371, -307.1465829586874179 ) ) ;
#24945 = CARTESIAN_POINT ( 'NONE',  ( -109.9466627088956585, -276.8993537287911977, -249.4366440837386278 ) ) ;
#24946 = CIRCLE ( 'NONE', #43069, 160.1282194813176716 ) ;
#24947 = CARTESIAN_POINT ( 'NONE',  ( -111.6322356973722236, -290.6396176618745812, -250.0647009199813908 ) ) ;
#24948 = EDGE_CURVE ( 'NONE', #93704, #63051, #51879, .T. ) ;
#24949 = CARTESIAN_POINT ( 'NONE',  ( 21.35490538856511833, -287.2236969503184127, -314.1784181319326876 ) ) ;
#24950 = CARTESIAN_POINT ( 'NONE',  ( -68.76144104770941112, -289.6390286088553694, -202.2457517645097198 ) ) ;
#24951 = VERTEX_POINT ( 'NONE', #88707 ) ;
#24952 = DIRECTION ( 'NONE',  ( 0.000000000000000000, 0.000000000000000000, 1.000000000000000000 ) ) ;
#24953 = CARTESIAN_POINT ( 'NONE',  ( -45.37543667678627912, -288.6643358988658861, -342.9796247055635376 ) ) ;
#24954 = CARTESIAN_POINT ( 'NONE',  ( 209.5646630284975629, 29.26077267968336315, 13.08022668053246740 ) ) ;
#24955 = CARTESIAN_POINT ( 'NONE',  ( -113.2565782013988951, -285.6406976867037315, -258.6193848352294822 ) ) ;
#24956 = CIRCLE ( 'NONE', #20432, 0.9999999999999986677 ) ;
#24957 = CARTESIAN_POINT ( 'NONE',  ( -13.92678369418804252, -291.4073269391968211, -197.1988004247917274 ) ) ;
#24958 = CARTESIAN_POINT ( 'NONE',  ( 36.20744015962704054, -282.8995747941821151, -250.3877213855793116 ) ) ;
#24959 = CARTESIAN_POINT ( 'NONE',  ( 8.239214098517875229, -281.9759987641352836, -208.8487233424524163 ) ) ;
#24960 = CARTESIAN_POINT ( 'NONE',  ( -51.01997869538324437, -283.0650301236675546, -342.1197702936550513 ) ) ;
#24961 = CARTESIAN_POINT ( 'NONE',  ( -87.46226070252184570, -297.3755750892354968, -211.8363220019750202 ) ) ;
#24962 = CARTESIAN_POINT ( 'NONE',  ( -79.14927638261603704, -274.7904860893174259, -209.8561775473375519 ) ) ;
#24963 = CARTESIAN_POINT ( 'NONE',  ( -47.18699936406832762, -289.9465539031880326, -196.3684366963796037 ) ) ;
#24964 = AXIS2_PLACEMENT_3D ( 'NONE', #31720, #53495, #17521 ) ;
#24965 = CARTESIAN_POINT ( 'NONE',  ( -109.9734265859501079, -271.4903272405545067, -259.4424881070290780 ) ) ;
#24966 = VERTEX_POINT ( 'NONE', #16751 ) ;
#24967 = DIRECTION ( 'NONE',  ( 0.000000000000000000, 1.000000000000000000, -0.000000000000000000 ) ) ;
#24968 = CARTESIAN_POINT ( 'NONE',  ( -103.5297167917779859, -286.9264217501230974, -236.2955834187858954 ) ) ;
#24969 = CARTESIAN_POINT ( 'NONE',  ( -13.86355234574031847, -295.8341141593112411, -343.3698098339721128 ) ) ;
#24970 = CARTESIAN_POINT ( 'NONE',  ( -85.79991449087306421, -286.0117269871989834, -215.5605196998682231 ) ) ;
#24971 = EDGE_CURVE ( 'NONE', #42443, #62086, #88164, .T. ) ;
#24972 = CARTESIAN_POINT ( 'NONE',  ( -25.81715911984839096, -275.9675261252064615, -346.2558158670120179 ) ) ;
#24973 = CARTESIAN_POINT ( 'NONE',  ( 17.41119197392769991, -293.4603246186936758, -216.2913910040802818 ) ) ;
#24974 = CARTESIAN_POINT ( 'NONE',  ( 2.118241632445099665, -284.7141658548872556, -205.6833128552913195 ) ) ;
#24975 = CARTESIAN_POINT ( 'NONE',  ( -58.93681956333193028, -292.1134500924573558, -196.4733983802848343 ) ) ;
#24976 = CARTESIAN_POINT ( 'NONE',  ( -98.12592179381310586, -290.3236088074801273, -310.8482574306502215 ) ) ;
#24977 = DIRECTION ( 'NONE',  ( 0.000000000000000000, 0.9681751575201845705, 0.2502735790305594676 ) ) ;
#24978 = CARTESIAN_POINT ( 'NONE',  ( 204.7786681169002350, 32.98517505407394168, 9.000000000000001776 ) ) ;
#24979 = CARTESIAN_POINT ( 'NONE',  ( -97.49377626717115675, -246.8080880501614160, -331.4215790215362176 ) ) ;
#24980 = CARTESIAN_POINT ( 'NONE',  ( -46.44218456700350117, -287.4587736984151434, -194.5990632669329159 ) ) ;
#24981 = CARTESIAN_POINT ( 'NONE',  ( -115.3288506153726871, -270.2666405000204009, -252.5284128619063608 ) ) ;
#24982 = EDGE_LOOP ( 'NONE', ( #47654, #89532, #19002, #26723 ) ) ;
#24983 = CARTESIAN_POINT ( 'NONE',  ( -92.80195566311395794, -282.7921144748079314, -318.3217121996497667 ) ) ;
#24984 = CARTESIAN_POINT ( 'NONE',  ( -72.83471064475116918, -277.1759716973489276, -338.6838738889823617 ) ) ;
#24985 = CARTESIAN_POINT ( 'NONE',  ( -46.71062212207951347, -281.9332393492775282, -196.0641906976348992 ) ) ;
#24986 = CARTESIAN_POINT ( 'NONE',  ( -110.7721571745674538, -273.6575316501529187, -283.9782850309709943 ) ) ;
#24987 = CARTESIAN_POINT ( 'NONE',  ( -0.6742606778060635797, -281.1496163467268730, -337.4140286614663182 ) ) ;
#24988 = CARTESIAN_POINT ( 'NONE',  ( -5.065103836973988471, -284.4991777402587445, -203.0412407449558145 ) ) ;
#24989 = CARTESIAN_POINT ( 'NONE',  ( -100.1972861174990470, -274.9799996766089407, -227.9654202172991688 ) ) ;
#24990 = CARTESIAN_POINT ( 'NONE',  ( -90.44765811065414596, -296.3216628452820487, -320.6111128458912845 ) ) ;
#24992 = VERTEX_POINT ( 'NONE', #37584 ) ;
#24991 = EDGE_CURVE ( 'NONE', #31159, #88967, #47336, .T. ) ;
#24993 = CARTESIAN_POINT ( 'NONE',  ( -17.28201242359606837, -291.0012081016744219, -199.6056034263659456 ) ) ;
#24994 = CARTESIAN_POINT ( 'NONE',  ( 32.92998674943279269, -276.6026556050021554, -301.5893553594597734 ) ) ;
#24995 = CARTESIAN_POINT ( 'NONE',  ( -46.17878014752664484, -273.9369232782852350, -197.8979824119133184 ) ) ;
#24996 = CARTESIAN_POINT ( 'NONE',  ( 36.98903739376044086, -274.2352935136458996, -251.4816590320255045 ) ) ;
#24997 = CARTESIAN_POINT ( 'NONE',  ( 175.2296996224750103, 20.00000000000000000, 0.000000000000000000 ) ) ;
#24998 = CARTESIAN_POINT ( 'NONE',  ( -65.94356194598800869, -271.6777997417465258, -201.0154030631533146 ) ) ;
#24999 = EDGE_CURVE ( 'NONE', #55951, #54596, #6560, .T. ) ;
#25000 = CARTESIAN_POINT ( 'NONE',  ( 8.566731766197730025, -295.8621839255966961, -331.4432116953627201 ) ) ;
#25001 = CARTESIAN_POINT ( 'NONE',  ( 153.2628468892384603, 20.37991841447901820, 11.93555113919330424 ) ) ;
#25002 = CARTESIAN_POINT ( 'NONE',  ( 212.3569123273291268, -147.7221692137691775, -10.75739200365177695 ) ) ;
#25003 = CARTESIAN_POINT ( 'NONE',  ( -109.2347950416587423, -285.8201850950070479, -256.0220462485468147 ) ) ;
#25004 = CARTESIAN_POINT ( 'NONE',  ( -11.03158101682675962, -284.4741215372958436, -341.7034313487334884 ) ) ;
#25005 = CARTESIAN_POINT ( 'NONE',  ( -97.43501274370701992, -284.4801380825769002, -228.7134444345888369 ) ) ;
#25006 = CARTESIAN_POINT ( 'NONE',  ( -9.707510823128119526, -275.0849210735937618, -338.8057591944971136 ) ) ;
#25007 = CARTESIAN_POINT ( 'NONE',  ( -45.75634227399419984, -285.0202243583240147, -344.1697311921894311 ) ) ;
#25008 = CARTESIAN_POINT ( 'NONE',  ( -89.59093267963146445, -276.2846886252912100, -322.4021050304311302 ) ) ;
#25009 = CARTESIAN_POINT ( 'NONE',  ( -13.97989637146349828, -275.4421884706039236, -200.8740530103883657 ) ) ;
#25010 = CARTESIAN_POINT ( 'NONE',  ( 195.2034772323600009, 41.96650104946161974, 13.30704316118699992 ) ) ;
#25011 = CARTESIAN_POINT ( 'NONE',  ( -84.47596062612213075, -280.2249929610514982, -209.6100054281786527 ) ) ;
#25012 = ORIENTED_EDGE ( 'NONE', *, *, #57248, .T. ) ;
#25013 = CARTESIAN_POINT ( 'NONE',  ( 201.2104617360081704, 15.00000000000000711, 10.00000000000000178 ) ) ;
#25014 = CARTESIAN_POINT ( 'NONE',  ( -113.1187155047932009, -286.3811513929716739, -272.8329575074588433 ) ) ;
#25015 = CARTESIAN_POINT ( 'NONE',  ( -10.44011714154755843, -293.8890886189444700, -338.3971860635331836 ) ) ;
#25016 = CARTESIAN_POINT ( 'NONE',  ( -103.7146442847458871, -289.3934818361951784, -309.2987281090792067 ) ) ;
#25017 = CARTESIAN_POINT ( 'NONE',  ( -5.340491729265707477, -284.7188931280256270, -203.6096202944680726 ) ) ;
#25019 = CARTESIAN_POINT ( 'NONE',  ( -106.6518019166097133, -289.1353579112077909, -244.2526876159719222 ) ) ;
#25018 = CARTESIAN_POINT ( 'NONE',  ( 30.51206343914375196, -285.7461960207598395, -241.7467718533398227 ) ) ;
#25020 = CARTESIAN_POINT ( 'NONE',  ( 11.38627293384450567, -287.9503721971141772, -215.4046386658568224 ) ) ;
#25021 = CARTESIAN_POINT ( 'NONE',  ( -111.2608893949524429, -276.7148886536036230, -257.6743489519632817 ) ) ;
#25022 = CARTESIAN_POINT ( 'NONE',  ( 37.88186166704951319, -286.1097444803992857, -282.8410012723633145 ) ) ;
#25023 = CARTESIAN_POINT ( 'NONE',  ( -37.99136011208090480, -288.0441689553572928, -195.3639274009831297 ) ) ;
#25024 = CARTESIAN_POINT ( 'NONE',  ( 37.77093731994414583, -285.6031122663101769, -274.3516212825301750 ) ) ;
#25025 = CARTESIAN_POINT ( 'NONE',  ( -51.05022569497469220, -284.1727838664469346, -342.3537015419958607 ) ) ;
#25026 = CARTESIAN_POINT ( 'NONE',  ( -38.85705544674746648, -291.0712801568224108, -345.5125127034490902 ) ) ;
#25027 = DIRECTION ( 'NONE',  ( 0.000000000000000000, -1.000000000000000000, 0.000000000000000000 ) ) ;
#25028 = CARTESIAN_POINT ( 'NONE',  ( 154.1772290835151011, 20.65814982784352694, -13.49254024715964029 ) ) ;
#25029 = CARTESIAN_POINT ( 'NONE',  ( -111.9712159807949661, -298.6240136288494114, -258.4574153217983508 ) ) ;
#25030 = AXIS2_PLACEMENT_3D ( 'NONE', #55838, #85176, #28364 ) ;
#25031 = CARTESIAN_POINT ( 'NONE',  ( 37.51763268699672693, -279.4930349287114950, -265.7697198595055283 ) ) ;
#25032 = CARTESIAN_POINT ( 'NONE',  ( 36.92914289369974767, -292.5016245303645519, -250.6125951860784369 ) ) ;
#25033 = CARTESIAN_POINT ( 'NONE',  ( -91.00278830484948855, -294.2295247924969317, -321.0995968437806027 ) ) ;
#25034 = CARTESIAN_POINT ( 'NONE',  ( 25.97544773420727537, -280.7472436800305786, -307.7736006643471001 ) ) ;
#25035 = CARTESIAN_POINT ( 'NONE',  ( 35.79273305344648293, -273.4524320866204334, -256.4805962555096812 ) ) ;
#25036 = CARTESIAN_POINT ( 'NONE',  ( -23.40904018080666660, -296.1856146146727156, -342.5734805678191037 ) ) ;
#25037 = CARTESIAN_POINT ( 'NONE',  ( -80.89948854861241045, -272.0486489451860166, -207.5170349825756375 ) ) ;
#25038 = CARTESIAN_POINT ( 'NONE',  ( 31.30482865398359493, -292.2165490865659763, -303.0663348960810595 ) ) ;
#25039 = CARTESIAN_POINT ( 'NONE',  ( 33.18863640069285736, -294.6996985007515377, -249.1893271684930085 ) ) ;
#25040 = DIRECTION ( 'NONE',  ( -0.000000000000000000, 1.000000000000000000, -0.000000000000000000 ) ) ;
#25041 = CARTESIAN_POINT ( 'NONE',  ( 18.59345203627408694, -293.6864562400584191, -223.2032927594639773 ) ) ;
#25042 = DIRECTION ( 'NONE',  ( -0.8457827187922920542, -0.5335274993777912034, -0.000000000000000000 ) ) ;
#25044 = CARTESIAN_POINT ( 'NONE',  ( 21.32646748840810247, -294.1612257996205244, -313.8012619570395145 ) ) ;
#25043 = CARTESIAN_POINT ( 'NONE',  ( -16.61889146615224178, -280.8059646905417139, -342.8650063351921062 ) ) ;
#25045 = CARTESIAN_POINT ( 'NONE',  ( -4.163835559721032809, -282.6267483492400743, -339.8610681934162585 ) ) ;
#25046 = CARTESIAN_POINT ( 'NONE',  ( -25.64311122380683372, -282.1202483747762813, -195.7122250675870134 ) ) ;
#25047 = CARTESIAN_POINT ( 'NONE',  ( -60.49951579780989164, -285.4266634271404541, -196.8926176604023510 ) ) ;
#25048 = CARTESIAN_POINT ( 'NONE',  ( -105.2085444465471937, -288.9671867804702856, -238.8314515452892692 ) ) ;
#25049 = CARTESIAN_POINT ( 'NONE',  ( 37.57767975301485563, -279.8492438214120739, -255.8768412473338856 ) ) ;
#25050 = CARTESIAN_POINT ( 'NONE',  ( 36.08544527965197801, -286.7519431525928439, -292.5414433792432192 ) ) ;
#25051 = CARTESIAN_POINT ( 'NONE',  ( 140.6539576904058606, 275.0000000000000568, 10.50000000000000000 ) ) ;
#25052 = CARTESIAN_POINT ( 'NONE',  ( -39.69434706120551226, -296.6822850743748745, -344.1361785667474464 ) ) ;
#25053 = CARTESIAN_POINT ( 'NONE',  ( -41.33535911566784193, -278.5267455061195960, -346.6805622605221515 ) ) ;
#25055 = CARTESIAN_POINT ( 'NONE',  ( -108.9071200265169779, -278.4110251519225017, -255.7904806030904581 ) ) ;
#25054 = CARTESIAN_POINT ( 'NONE',  ( 36.97977237842980003, -291.7322195847041257, -282.8780194435805697 ) ) ;
#25056 = CARTESIAN_POINT ( 'NONE',  ( -3.323264629320932251, -292.6556181789358106, -201.2687545031113245 ) ) ;
#25057 = CARTESIAN_POINT ( 'NONE',  ( -111.1243629882546742, -282.4243651793003096, -286.6532284566049498 ) ) ;
#25058 = CARTESIAN_POINT ( 'NONE',  ( -37.10696594301988682, -279.0493349546974287, -345.3734749490556624 ) ) ;
#25059 = CARTESIAN_POINT ( 'NONE',  ( 28.60121606276117490, -293.0420555563247831, -302.3361556639268315 ) ) ;
#25060 = CARTESIAN_POINT ( 'NONE',  ( 28.61621260249760113, -296.8776238487828891, -195.3835988277860736 ) ) ;
#25061 = EDGE_LOOP ( 'NONE', ( #86444, #33035, #6562, #31270 ) ) ;
#25062 = CARTESIAN_POINT ( 'NONE',  ( 160.5350683151633291, 276.0000000000000568, 20.22542485937379908 ) ) ;
#25063 = CARTESIAN_POINT ( 'NONE',  ( 18.01495856046697952, -293.7385066707562373, -318.0627750461171104 ) ) ;
#25064 = PLANE ( 'NONE',  #6668 ) ;
#25065 = CARTESIAN_POINT ( 'NONE',  ( 17.36665895637873192, -285.6952119285918457, -314.0302885647153062 ) ) ;
#25066 = CARTESIAN_POINT ( 'NONE',  ( -65.44466701188630964, -296.7524811496746224, -198.8687172117747082 ) ) ;
#25067 = CARTESIAN_POINT ( 'NONE',  ( -46.46341972090297645, -287.2538587767685385, -194.3999930321851934 ) ) ;
#25068 = CARTESIAN_POINT ( 'NONE',  ( 25.69497855006543219, -287.8919922355431709, -307.2764936944447527 ) ) ;
#25069 = CARTESIAN_POINT ( 'NONE',  ( -83.42539217835839338, -279.2168902879174084, -327.9333112984667196 ) ) ;
#25070 = CARTESIAN_POINT ( 'NONE',  ( -103.4473583112783928, -298.7592330576563882, -236.9600625526651356 ) ) ;
#25071 = CARTESIAN_POINT ( 'NONE',  ( -102.5013647381963580, -277.8053727829788500, -236.4666975723167468 ) ) ;
#25072 = EDGE_LOOP ( 'NONE', ( #91105, #61658, #37081, #80168 ) ) ;
#25073 = CARTESIAN_POINT ( 'NONE',  ( -48.96260573817354356, -297.5748347812544807, -194.2108251305076294 ) ) ;
#25074 = CARTESIAN_POINT ( 'NONE',  ( -108.3830566885144009, -292.7618007427822135, -248.0821281254899873 ) ) ;
#25075 = CARTESIAN_POINT ( 'NONE',  ( 22.55561096220015216, -295.7889791258217542, -317.4856954286067321 ) ) ;
#25076 = CARTESIAN_POINT ( 'NONE',  ( 215.7837434059060229, -147.7221692137691775, 8.778910157967997563 ) ) ;
#25077 = CARTESIAN_POINT ( 'NONE',  ( -110.4388797586241253, -291.1925874554362963, -271.1947833155672356 ) ) ;
#25078 = CARTESIAN_POINT ( 'NONE',  ( 196.2769060748385641, 71.88909962519697672, 11.58303352224541172 ) ) ;
#25079 = CARTESIAN_POINT ( 'NONE',  ( 22.15310391925788380, -291.0538936007217785, -223.4290380428915910 ) ) ;
#25080 = CARTESIAN_POINT ( 'NONE',  ( -103.8336813317700233, -297.3914678223946453, -231.4673927706366499 ) ) ;
#25081 = CARTESIAN_POINT ( 'NONE',  ( -101.2310140975651791, -296.7019934227330964, -235.0023418837693043 ) ) ;
#25082 = DIRECTION ( 'NONE',  ( -0.000000000000000000, -0.000000000000000000, -1.000000000000000000 ) ) ;
#25083 = CARTESIAN_POINT ( 'NONE',  ( 208.4306832106270804, -198.2391364535880598, 7.500000000000012434 ) ) ;
#25084 = CARTESIAN_POINT ( 'NONE',  ( -89.00769167969961870, -291.2830545843509640, -326.5156642655576889 ) ) ;
#25085 = CARTESIAN_POINT ( 'NONE',  ( -111.2586520408596868, -292.6233781216987495, -305.9938812882205070 ) ) ;
#25086 = CARTESIAN_POINT ( 'NONE',  ( -109.8638012882397561, -286.3146966435153900, -288.8157454015562280 ) ) ;
#25087 = CARTESIAN_POINT ( 'NONE',  ( 33.81277426305639722, -273.2500782434123607, -247.0194919982113220 ) ) ;
#25088 = CARTESIAN_POINT ( 'NONE',  ( -2.256129440645577855, -276.4404837920299656, -204.7081140189993107 ) ) ;
#25089 = CARTESIAN_POINT ( 'NONE',  ( -47.16067182951224623, -290.0062824044792933, -196.5715388337401919 ) ) ;
#25090 = CARTESIAN_POINT ( 'NONE',  ( -64.62774775184927023, -279.2649063883087024, -341.0973042245017268 ) ) ;
#25091 = EDGE_LOOP ( 'NONE', ( #60646, #28800, #78064, #79289, #4691, #20100 ) ) ;
#25092 = CARTESIAN_POINT ( 'NONE',  ( -26.73617389350672013, -282.2624118907904176, -342.7410132165962864 ) ) ;
#25093 = CARTESIAN_POINT ( 'NONE',  ( -80.04261685321067432, -278.6946497979890296, -334.1284465297387669 ) ) ;
#25094 = CARTESIAN_POINT ( 'NONE',  ( 14.90180662687149749, -279.5637330310814832, -214.2651621593729772 ) ) ;
#25095 = CARTESIAN_POINT ( 'NONE',  ( -95.53025548571402226, -238.2189646283312356, -339.1223768606931799 ) ) ;
#25096 = CARTESIAN_POINT ( 'NONE',  ( 34.49732749125324460, -276.1500600901871394, -243.3060939906405906 ) ) ;
#25097 = EDGE_CURVE ( 'NONE', #36396, #62468, #29192, .T. ) ;
#25098 = SHAPE_DEFINITION_REPRESENTATION ( #40553, #78428 ) ;
#25099 = CARTESIAN_POINT ( 'NONE',  ( -41.17746381798538380, -275.5249504634946334, -194.0991289433486315 ) ) ;
#25100 = CARTESIAN_POINT ( 'NONE',  ( -67.74223827176244583, -276.1233781216987495, -207.3071070584150277 ) ) ;
#25101 = ORIENTED_EDGE ( 'NONE', *, *, #10707, .T. ) ;
#25102 = ORIENTED_EDGE ( 'NONE', *, *, #11054, .F. ) ;
#25103 = CARTESIAN_POINT ( 'NONE',  ( -45.38275674166889218, -290.2361010911722019, -343.2278969830596793 ) ) ;
#25104 = CARTESIAN_POINT ( 'NONE',  ( -23.47456837290901532, -290.6375113347210686, -345.1251422553833663 ) ) ;
#25105 = CARTESIAN_POINT ( 'NONE',  ( -104.1442364373609593, -289.5001548687426975, -300.1730902607314420 ) ) ;
#25106 = CARTESIAN_POINT ( 'NONE',  ( 25.49846971219115943, -286.4716410379926401, -225.9465103141010047 ) ) ;
#25107 = FACE_OUTER_BOUND ( 'NONE', #3409, .T. ) ;
#25108 = CARTESIAN_POINT ( 'NONE',  ( 35.48980932413891054, -280.1075186424955632, -282.2779819497087033 ) ) ;
#25109 = CARTESIAN_POINT ( 'NONE',  ( 36.89054456648177904, -289.4211734303212324, -271.0239339768702393 ) ) ;
#25110 = CARTESIAN_POINT ( 'NONE',  ( -32.11567005307058764, -281.4649067403271374, -343.8689159535326212 ) ) ;
#25111 = CARTESIAN_POINT ( 'NONE',  ( -94.33349461238223910, -280.5197139791829386, -223.9587598416172796 ) ) ;
#25112 = CARTESIAN_POINT ( 'NONE',  ( 39.11914881985140369, -288.4006570871002850, -262.9679640439396167 ) ) ;
#25113 = CARTESIAN_POINT ( 'NONE',  ( -66.09969295732130945, -280.1577006354656305, -203.1837393843491384 ) ) ;
#25114 = CARTESIAN_POINT ( 'NONE',  ( -111.1634431910774765, -289.0895005352157341, -290.8149433070904024 ) ) ;
#25115 = CARTESIAN_POINT ( 'NONE',  ( -85.41984761917466074, -286.2093962739002109, -210.4223946576599928 ) ) ;
#25116 = CARTESIAN_POINT ( 'NONE',  ( -85.47929151680671112, -285.8989608587163502, -210.3419610545740852 ) ) ;
#25117 = CARTESIAN_POINT ( 'NONE',  ( -108.7196147447171342, -284.5161726657777876, -285.7238559050579170 ) ) ;
#25118 = ORIENTED_EDGE ( 'NONE', *, *, #22764, .F. ) ;
#25119 = DIRECTION ( 'NONE',  ( 1.000000000000000000, 0.000000000000000000, -0.000000000000000000 ) ) ;
#25120 = CARTESIAN_POINT ( 'NONE',  ( 12.44863597966686264, -294.5976484457647757, -213.2539563626215795 ) ) ;
#25121 = CARTESIAN_POINT ( 'NONE',  ( 31.74787745047207110, -291.8116552382054465, -237.3756766234327529 ) ) ;
#25122 = CARTESIAN_POINT ( 'NONE',  ( -19.20178795123518611, -273.3499643337128191, -199.3553518276607974 ) ) ;
#25123 = CARTESIAN_POINT ( 'NONE',  ( -22.12583956799603868, -294.2107332157362976, -345.7387696685323135 ) ) ;
#25124 = CARTESIAN_POINT ( 'NONE',  ( -30.72563090472262459, -290.6171782834506985, -196.9653730075692977 ) ) ;
#25125 = CARTESIAN_POINT ( 'NONE',  ( -85.14950810018693517, -293.9622843865565756, -326.9296437064185170 ) ) ;
#25126 = CARTESIAN_POINT ( 'NONE',  ( -32.14440362602869072, -293.3242137605143967, -197.1355980830198860 ) ) ;
#25127 = CARTESIAN_POINT ( 'NONE',  ( 223.4306832106270804, -135.2391364535880882, 21.50000000000000000 ) ) ;
#25128 = CARTESIAN_POINT ( 'NONE',  ( 0.7925061022009262102, -290.5589297706146681, -205.5265470059704285 ) ) ;
#25129 = CARTESIAN_POINT ( 'NONE',  ( 35.47390695503809610, -295.3209147620497106, -252.3394341053670757 ) ) ;
#25130 = CARTESIAN_POINT ( 'NONE',  ( -23.72972316758523803, -289.8153276731919732, -342.3721577262268170 ) ) ;
#25131 = CARTESIAN_POINT ( 'NONE',  ( -34.33101972808530178, -278.9943606447806701, -345.6561550612795486 ) ) ;
#25132 = CARTESIAN_POINT ( 'NONE',  ( -34.32218799048951041, -275.8099074843981384, -346.9045126413045637 ) ) ;
#25133 = CARTESIAN_POINT ( 'NONE',  ( -36.88775850084964958, -297.2548719360385689, -193.5226530337290853 ) ) ;
#25134 = CARTESIAN_POINT ( 'NONE',  ( -70.35737331132168038, -277.6934137627417840, -203.6290921608441806 ) ) ;
#25135 = CARTESIAN_POINT ( 'NONE',  ( -102.9277226285899758, -276.4401961655864852, -309.2578596960130994 ) ) ;
#25136 = CARTESIAN_POINT ( 'NONE',  ( -110.2961260465879576, -295.1152369048035098, -279.6516817937797441 ) ) ;
#25137 = DIRECTION ( 'NONE',  ( -1.000000000000000000, -0.000000000000000000, -0.000000000000000000 ) ) ;
#25138 = CARTESIAN_POINT ( 'NONE',  ( -109.9879886971798157, -273.3109204383923725, -262.2119201555834138 ) ) ;
#25139 = DIRECTION ( 'NONE',  ( 1.124465274301078281E-16, 1.000000000000000000, -0.000000000000000000 ) ) ;
#25141 = CARTESIAN_POINT ( 'NONE',  ( 2.931709498142104131, -274.4424217968935977, -209.4151356217638522 ) ) ;
#25140 = CARTESIAN_POINT ( 'NONE',  ( -23.63637687900775930, -286.8980798513205741, -344.5124607947947766 ) ) ;
#25142 = CARTESIAN_POINT ( 'NONE',  ( 37.82494409277387604, -287.7617935739439758, -287.1238747688250328 ) ) ;
#25143 = CARTESIAN_POINT ( 'NONE',  ( -34.85324837914217966, -300.0630427749880482, -195.0050747326455678 ) ) ;
#25144 = CARTESIAN_POINT ( 'NONE',  ( -112.2188999222151864, -294.5377763305235703, -271.4653726716557003 ) ) ;
#25145 = EDGE_CURVE ( 'NONE', #25416, #50728, #44221, .T. ) ;
#25146 = CARTESIAN_POINT ( 'NONE',  ( -67.82670965532517471, -282.6393887781904937, -340.8935432561564767 ) ) ;
#25147 = ADVANCED_FACE ( 'NONE', ( #31436 ), #17086, .T. ) ;
#25148 = DIRECTION ( 'NONE',  ( 0.000000000000000000, 1.000000000000000000, -0.000000000000000000 ) ) ;
#25149 = CARTESIAN_POINT ( 'NONE',  ( -42.99027323350390617, -277.9808197747851182, -195.5229303319318319 ) ) ;
#25150 = PLANE ( 'NONE',  #24751 ) ;
#25151 = CARTESIAN_POINT ( 'NONE',  ( -65.46498868004236726, -290.4710229748278039, -202.5521695197263909 ) ) ;
#25152 = CARTESIAN_POINT ( 'NONE',  ( 199.6898571221144039, 41.17245366902173487, 10.18361224148079280 ) ) ;
#25153 = CARTESIAN_POINT ( 'NONE',  ( 175.2296996224750103, 140.2072866198470251, 0.000000000000000000 ) ) ;
#25154 = CARTESIAN_POINT ( 'NONE',  ( -96.68158721091300833, -289.1805867935663628, -224.4941532505116015 ) ) ;
#25155 = CARTESIAN_POINT ( 'NONE',  ( -21.80656606556936694, -275.7750136912459880, -198.3238542910373781 ) ) ;
#25156 = CARTESIAN_POINT ( 'NONE',  ( 38.08911892454495529, -283.1321845092203375, -282.6412405056415764 ) ) ;
#25158 = CARTESIAN_POINT ( 'NONE',  ( -70.21492497528232946, -283.4978458239715451, -335.5544728161844432 ) ) ;
#25157 = CARTESIAN_POINT ( 'NONE',  ( 17.90906207888829726, -296.7606155457845034, -195.0244414490978215 ) ) ;
#25159 = CARTESIAN_POINT ( 'NONE',  ( 5.505204031250785945, -276.0699991422507651, -210.4690768661828599 ) ) ;
#25160 = CARTESIAN_POINT ( 'NONE',  ( -4.040294945074710320, -275.3058196584017310, -205.2039958640114037 ) ) ;
#25161 = CARTESIAN_POINT ( 'NONE',  ( -60.58695834865802965, -285.3536961951770081, -341.7221410843583271 ) ) ;
#25162 = EDGE_LOOP ( 'NONE', ( #6103, #7029, #91039, #43148, #55361, #29948 ) ) ;
#25163 = CARTESIAN_POINT ( 'NONE',  ( 189.9243309297870610, 250.0000000000000568, 20.22542485937349355 ) ) ;
#25164 = CARTESIAN_POINT ( 'NONE',  ( 32.22911027982584642, -293.8097538677115494, -303.4839243319868274 ) ) ;
#25165 = CARTESIAN_POINT ( 'NONE',  ( -108.9631407931277636, -286.2594202610957836, -291.4356343291743769 ) ) ;
#25166 = DIRECTION ( 'NONE',  ( 0.000000000000000000, 0.000000000000000000, 1.000000000000000000 ) ) ;
#25167 = CARTESIAN_POINT ( 'NONE',  ( -117.3381139276884966, -270.1608578419545665, -261.3154543817420290 ) ) ;
#25168 = CARTESIAN_POINT ( 'NONE',  ( -42.80491282601077785, -276.3166167435363150, -347.0051792499501744 ) ) ;
#25169 = CARTESIAN_POINT ( 'NONE',  ( -77.72984708707444668, -287.9843144344482653, -335.0387596558152268 ) ) ;
#25170 = CARTESIAN_POINT ( 'NONE',  ( -51.12880872620584682, -284.7515606856853765, -342.8053322172132766 ) ) ;
#25171 = CARTESIAN_POINT ( 'NONE',  ( -3.382832845664823562, -278.3574796677457357, -336.1240965390247197 ) ) ;
#25172 = CARTESIAN_POINT ( 'NONE',  ( -60.34992273855526435, -287.1849336966969872, -197.4415129900818897 ) ) ;
#25173 = CARTESIAN_POINT ( 'NONE',  ( 16.68282718286465283, -282.8204410232708028, -218.2643534992610057 ) ) ;
#25174 = CARTESIAN_POINT ( 'NONE',  ( 38.92388368347735650, -275.5861456202410977, -259.7516537931156222 ) ) ;
#25175 = CARTESIAN_POINT ( 'NONE',  ( -48.49608528405272523, -277.0235862677593559, -346.6028048552147993 ) ) ;
#25176 = CARTESIAN_POINT ( 'NONE',  ( -41.98206177234902725, -299.9133670332113297, -196.0658876998973597 ) ) ;
#25177 = CARTESIAN_POINT ( 'NONE',  ( 155.9223079842149104, 17.31716537717099058, 7.900495735314976287 ) ) ;
#25178 = CARTESIAN_POINT ( 'NONE',  ( -95.99890600148557951, -281.6948066931273615, -223.6242672951989618 ) ) ;
#25179 = CARTESIAN_POINT ( 'NONE',  ( -33.39053363272466157, -296.2407055138936585, -194.5975469267984010 ) ) ;
#25180 = CYLINDRICAL_SURFACE ( 'NONE', #18305, 0.5000000000000004441 ) ;
#25181 = CARTESIAN_POINT ( 'NONE',  ( -53.97402699466512388, -276.7790018905211014, -341.5564983688221332 ) ) ;
#25182 = CARTESIAN_POINT ( 'NONE',  ( 0.9834008940867228210, -275.7567751832115732, -204.0194830156026455 ) ) ;
#25183 = CARTESIAN_POINT ( 'NONE',  ( 36.24966276459002756, -280.8878687597151043, -292.3872257591397670 ) ) ;
#25184 = CARTESIAN_POINT ( 'NONE',  ( 32.79378289114194445, -289.0025066346683502, -246.7181901884279682 ) ) ;
#25185 = CARTESIAN_POINT ( 'NONE',  ( -112.5173958698081407, -297.9033231660807814, -283.7482983842118074 ) ) ;
#25186 = CARTESIAN_POINT ( 'NONE',  ( -37.67178547851752768, -296.2612328933909112, -346.9763469458639520 ) ) ;
#25187 = CARTESIAN_POINT ( 'NONE',  ( -30.66822414133165609, -294.1368928966069802, -195.8259373990516110 ) ) ;
#25188 = CARTESIAN_POINT ( 'NONE',  ( -92.63468657255643279, -277.2574126706537072, -219.9357862776953141 ) ) ;
#25189 = CARTESIAN_POINT ( 'NONE',  ( -21.91948622416577663, -282.1713169440589581, -197.4833172403596961 ) ) ;
#25190 = CARTESIAN_POINT ( 'NONE',  ( -69.86503574326503951, -295.7002740160994563, -203.4018255548325271 ) ) ;
#25191 = CARTESIAN_POINT ( 'NONE',  ( -96.19763467012533908, -285.7619750118894331, -318.0919214514875648 ) ) ;
#25192 = CARTESIAN_POINT ( 'NONE',  ( 18.90774963471604408, -285.8078206768904579, -223.3285211886541504 ) ) ;
#25193 = CARTESIAN_POINT ( 'NONE',  ( -93.43388131815913766, -240.9352012794298048, -341.3099153835386801 ) ) ;
#25194 = ORIENTED_EDGE ( 'NONE', *, *, #33757, .F. ) ;
#25195 = CARTESIAN_POINT ( 'NONE',  ( 35.67628277333682263, -287.2278293432846681, -271.0405734159317603 ) ) ;
#25196 = ORIENTED_EDGE ( 'NONE', *, *, #20342, .F. ) ;
#25197 = CARTESIAN_POINT ( 'NONE',  ( -37.30055933580196381, -284.1312777191505461, -347.0650093396591274 ) ) ;
#25198 = CARTESIAN_POINT ( 'NONE',  ( -1.716021741578490856, -274.8713905094053871, -206.6059306492987275 ) ) ;
#25199 = CARTESIAN_POINT ( 'NONE',  ( 37.33600110609494038, -286.1318820393241822, -253.2368117600678943 ) ) ;
#25200 = CARTESIAN_POINT ( 'NONE',  ( -99.77139272779301393, -290.0648481671703394, -225.8187113112333009 ) ) ;
#25201 = CARTESIAN_POINT ( 'NONE',  ( -5.053894075478392978, -281.4081619655672171, -200.7168950041703397 ) ) ;
#25202 = CARTESIAN_POINT ( 'NONE',  ( 194.7336594103350080, 19.94899969135506979, -14.16570715603806008 ) ) ;
#25203 = CARTESIAN_POINT ( 'NONE',  ( -104.1955451656680793, -280.5530532153895251, -233.5742839954862973 ) ) ;
#25204 = CARTESIAN_POINT ( 'NONE',  ( 38.23312054843977847, -281.7023473310466102, -255.7258601676017804 ) ) ;
#25205 = CARTESIAN_POINT ( 'NONE',  ( -105.5937364680635966, -287.8380690714489560, -285.9065529553535612 ) ) ;
#25206 = CARTESIAN_POINT ( 'NONE',  ( -62.97513941457921760, -183.2172664956623009, -362.5461488121814000 ) ) ;
#25207 = ORIENTED_EDGE ( 'NONE', *, *, #48163, .F. ) ;
#25208 = CARTESIAN_POINT ( 'NONE',  ( 30.83474101785412813, -277.9579614473229867, -301.2156362274538992 ) ) ;
#25209 = CARTESIAN_POINT ( 'NONE',  ( 202.4138562182569387, 295.8836489450775957, -54.00000000003736034 ) ) ;
#25210 = CARTESIAN_POINT ( 'NONE',  ( 35.83831777116904505, -279.7629271663977306, -285.1403556233622112 ) ) ;
#25211 = CARTESIAN_POINT ( 'NONE',  ( -8.748272599226140755, -296.4434134283867479, -340.8184974123483357 ) ) ;
#25212 = CARTESIAN_POINT ( 'NONE',  ( -105.0594421304473940, -295.5324056855743038, -297.8965512642938052 ) ) ;
#25213 = CARTESIAN_POINT ( 'NONE',  ( -33.53613339093320178, -291.6065071166103166, -193.5168301977918475 ) ) ;
#25214 = CARTESIAN_POINT ( 'NONE',  ( 150.6539576904058606, 293.9636489450775230, 9.103929867429224387 ) ) ;
#25216 = CARTESIAN_POINT ( 'NONE',  ( 24.90226242880337892, -286.4943325827110243, -310.0112067575118431 ) ) ;
#25215 = CARTESIAN_POINT ( 'NONE',  ( -112.3070419704224889, -295.3141535650882474, -255.5018913414270969 ) ) ;
#25217 = CARTESIAN_POINT ( 'NONE',  ( 31.74363342494571683, -295.7714731510176307, -297.6695450812549097 ) ) ;
#25218 = CARTESIAN_POINT ( 'NONE',  ( -10.58593706380056254, -287.7237911593846320, -201.8977204074249130 ) ) ;
#25219 = ORIENTED_EDGE ( 'NONE', *, *, #48693, .F. ) ;
#25220 = CARTESIAN_POINT ( 'NONE',  ( 37.19060834858754561, -294.2627866692729413, -251.9830003684886890 ) ) ;
#25221 = CARTESIAN_POINT ( 'NONE',  ( -99.07968294639007922, -284.5039165993395045, -309.5251142473516666 ) ) ;
#25222 = CARTESIAN_POINT ( 'NONE',  ( -104.2635283825039210, -294.8601048830344666, -307.7452902670593744 ) ) ;
#25223 = CARTESIAN_POINT ( 'NONE',  ( -110.2808628256932622, -291.6616932123060906, -246.0276771575050248 ) ) ;
#25224 = CARTESIAN_POINT ( 'NONE',  ( -47.74128603324633247, -292.4157796233029103, -194.0749874361701757 ) ) ;
#25225 = CARTESIAN_POINT ( 'NONE',  ( -78.17265769043761736, -289.7845943366682491, -330.9350521204080451 ) ) ;
#25226 = ORIENTED_EDGE ( 'NONE', *, *, #73250, .F. ) ;
#25227 = CARTESIAN_POINT ( 'NONE',  ( 175.2296996224750103, 250.5000000000000568, 0.000000000000000000 ) ) ;
#25228 = CARTESIAN_POINT ( 'NONE',  ( -48.80684464599588779, -299.7681786728757061, -195.4160152565822273 ) ) ;
#25229 = CARTESIAN_POINT ( 'NONE',  ( -103.8769957264625958, -271.8439022749217884, -232.2933646106326364 ) ) ;
#25230 = CARTESIAN_POINT ( 'NONE',  ( 33.68671444085101996, -280.3755698939135073, -252.4671301250645001 ) ) ;
#25231 = VERTEX_POINT ( 'NONE', #74044 ) ;
#25232 = CARTESIAN_POINT ( 'NONE',  ( 38.66779417274447894, -274.9095495595499870, -258.3562667534898765 ) ) ;
#25233 = CARTESIAN_POINT ( 'NONE',  ( -109.2728116222713766, -294.8226935133391748, -286.3805734636300713 ) ) ;
#25234 = CARTESIAN_POINT ( 'NONE',  ( 3.838665179277843009, -278.3516282875589241, -332.1271522709898250 ) ) ;
#25235 = CARTESIAN_POINT ( 'NONE',  ( 8.105489990007118450, -272.8207661384156495, -211.6634315901055174 ) ) ;
#25236 = CARTESIAN_POINT ( 'NONE',  ( -109.7521570903174535, -297.5998672125587632, -282.3551259800321986 ) ) ;
#25237 = CARTESIAN_POINT ( 'NONE',  ( -92.08483910244299864, -298.3260921711725473, -221.6023771320925277 ) ) ;
#25238 = CARTESIAN_POINT ( 'NONE',  ( 175.2296996224750103, 160.0000000000000568, -24.00000000000001066 ) ) ;
#25239 = CARTESIAN_POINT ( 'NONE',  ( -107.0495268115293896, -298.5505482323789010, -239.4530033461889786 ) ) ;
#25240 = CARTESIAN_POINT ( 'NONE',  ( -112.6969001285957432, -270.5725786104129043, -270.3359661452269620 ) ) ;
#25241 = CARTESIAN_POINT ( 'NONE',  ( 28.82726061175138810, -293.7829783668840378, -239.1681964442797153 ) ) ;
#25242 = CARTESIAN_POINT ( 'NONE',  ( -55.13741884599251364, -290.3934756011420859, -198.9560249515514840 ) ) ;
#25243 = CARTESIAN_POINT ( 'NONE',  ( 208.1751813995450107, 30.16346637533325747, 14.32775664334902821 ) ) ;
#25244 = CARTESIAN_POINT ( 'NONE',  ( 32.49456653272469708, -275.6296617277954510, -237.9476973030945999 ) ) ;
#25245 = CARTESIAN_POINT ( 'NONE',  ( -89.24366284580175090, -273.4628928124282652, -219.0270525820155854 ) ) ;
#25246 = CARTESIAN_POINT ( 'NONE',  ( 35.72999478662111272, -283.2966628321873372, -251.9509520787949839 ) ) ;
#25247 = CARTESIAN_POINT ( 'NONE',  ( -71.53347191452294851, -282.1792009550591729, -338.8024871738685420 ) ) ;
#25248 = CARTESIAN_POINT ( 'NONE',  ( 189.9243309297870610, 215.0000000000000568, 20.22542485937349355 ) ) ;
#25249 = CARTESIAN_POINT ( 'NONE',  ( -110.0344009423584879, -283.6347179900207607, -279.0674441476498941 ) ) ;
#25250 = CARTESIAN_POINT ( 'NONE',  ( -110.1067911311129990, -282.3097460872800184, -289.2608214239889435 ) ) ;
#25251 = CARTESIAN_POINT ( 'NONE',  ( 35.93912889016937129, -274.2149443663769262, -277.0912750860239271 ) ) ;
#25252 = CARTESIAN_POINT ( 'NONE',  ( -59.36924147933729046, -281.7672785440761913, -198.6153887634210946 ) ) ;
#25253 = CARTESIAN_POINT ( 'NONE',  ( 208.6610832702913285, 1.063508326896295486, 7.500000000000013323 ) ) ;
#25254 = CARTESIAN_POINT ( 'NONE',  ( 195.1565306243040823, 21.00000000082943430, 15.11139605583089462 ) ) ;
#25255 = CARTESIAN_POINT ( 'NONE',  ( -92.57807190576829726, -271.6771615585735731, -217.8503338192332990 ) ) ;
#25256 = CARTESIAN_POINT ( 'NONE',  ( -81.44940733752194717, -279.6507961020809034, -331.2260388195819587 ) ) ;
#25257 = ADVANCED_FACE ( 'NONE', ( #89163 ), #1612, .F. ) ;
#25258 = CARTESIAN_POINT ( 'NONE',  ( 184.5358909326088792, 2.965303559109565779, 10.00000000000000000 ) ) ;
#25259 = CARTESIAN_POINT ( 'NONE',  ( -111.7150981210542540, -286.2986547208555521, -283.9862470302665542 ) ) ;
#25260 = ORIENTED_EDGE ( 'NONE', *, *, #80129, .T. ) ;
#25261 = CARTESIAN_POINT ( 'NONE',  ( 208.7913547201125084, 38.28482993310899474, 14.12814564770278025 ) ) ;
#25262 = CARTESIAN_POINT ( 'NONE',  ( -29.83112135436138956, -286.9570422825841547, -345.0355507747944444 ) ) ;
#25263 = DIRECTION ( 'NONE',  ( 0.000000000000000000, 0.000000000000000000, -1.000000000000000000 ) ) ;
#25264 = CARTESIAN_POINT ( 'NONE',  ( -110.4963473120028112, -295.2610165182085211, -276.9199384511147741 ) ) ;
#25265 = CARTESIAN_POINT ( 'NONE',  ( -97.57447250935021543, -288.0950306985853899, -313.7532671935239819 ) ) ;
#25266 = CARTESIAN_POINT ( 'NONE',  ( 156.0793278192224420, 19.94580804510003347, -11.55434249967656690 ) ) ;
#25267 = CARTESIAN_POINT ( 'NONE',  ( -98.49924495541347369, -295.1420787038750291, -226.9473487275503487 ) ) ;
#25268 = CARTESIAN_POINT ( 'NONE',  ( 13.79671879221067243, -285.2332663998147950, -213.6547990546205540 ) ) ;
#25269 = CARTESIAN_POINT ( 'NONE',  ( -7.696587696186280247, -282.0474224700297441, -202.7632188005093496 ) ) ;
#25270 = CARTESIAN_POINT ( 'NONE',  ( -87.66741468874603527, -281.9830977621025454, -327.3637777075008444 ) ) ;
#25271 = CARTESIAN_POINT ( 'NONE',  ( 7.979943769627845462, -288.4125489688288440, -327.5882845593636716 ) ) ;
#25272 = CARTESIAN_POINT ( 'NONE',  ( -46.54802444680345275, -281.3584437868312875, -197.2985173056615906 ) ) ;
#25273 = CARTESIAN_POINT ( 'NONE',  ( -22.17088307361434474, -281.0541752502652457, -198.7378679017543277 ) ) ;
#25274 = CARTESIAN_POINT ( 'NONE',  ( -2.537498904906047681, -290.5739818968099257, -337.1972936879895428 ) ) ;
#25275 = CARTESIAN_POINT ( 'NONE',  ( 99.18384067648280222, -299.8839462645673848, -193.3572539837404349 ) ) ;
#25276 = ORIENTED_EDGE ( 'NONE', *, *, #4151, .F. ) ;
#25277 = CARTESIAN_POINT ( 'NONE',  ( -106.8432217404455997, -272.9770507113296389, -237.2169104408783369 ) ) ;
#25278 = CARTESIAN_POINT ( 'NONE',  ( -30.68484402586279458, -294.1166278728923089, -196.0137369299496299 ) ) ;
#25279 = CARTESIAN_POINT ( 'NONE',  ( 153.6539576904058038, 131.0000000000000568, 12.50000000000000000 ) ) ;
#25280 = CARTESIAN_POINT ( 'NONE',  ( 31.95455697924148097, -277.6233781216988064, -236.9535640164627637 ) ) ;
#25281 = EDGE_LOOP ( 'NONE', ( #48259, #79972, #92607, #11885 ) ) ;
#25282 = CARTESIAN_POINT ( 'NONE',  ( 36.92041395726739239, -273.4019796760302938, -258.6518468044378665 ) ) ;
#25283 = DIRECTION ( 'NONE',  ( 0.000000000000000000, 0.000000000000000000, 1.000000000000000000 ) ) ;
#25284 = CARTESIAN_POINT ( 'NONE',  ( -111.8142459796560928, -295.1566365512167067, -254.1670871884807923 ) ) ;
#25285 = CARTESIAN_POINT ( 'NONE',  ( -89.30881257830486675, -272.6449314474696166, -218.9479689669707341 ) ) ;
#25286 = CARTESIAN_POINT ( 'NONE',  ( -111.0301178524968719, -292.0611564083727103, -271.2124955562864557 ) ) ;
#25287 = CARTESIAN_POINT ( 'NONE',  ( 16.57927784217249112, -284.0328252484292193, -321.1352046807982106 ) ) ;
#25288 = CARTESIAN_POINT ( 'NONE',  ( -76.88002984230645609, -292.9592470108124189, -204.9141055977990504 ) ) ;
#25289 = CARTESIAN_POINT ( 'NONE',  ( -101.2810941020852624, -292.4242238568601238, -228.2534963741508420 ) ) ;
#25290 = CARTESIAN_POINT ( 'NONE',  ( 8.226511291301040529, -294.2422458917769177, -327.4571095112128205 ) ) ;
#25291 = CARTESIAN_POINT ( 'NONE',  ( 19.26953764472149899, -288.8696336939174216, -221.1659108086443553 ) ) ;
#25292 = CARTESIAN_POINT ( 'NONE',  ( 22.52460511167108237, -282.3683730855884164, -318.8073852795956782 ) ) ;
#25293 = CARTESIAN_POINT ( 'NONE',  ( -87.66496115127756639, -293.8278495772934207, -326.7951511929214803 ) ) ;
#25294 = CARTESIAN_POINT ( 'NONE',  ( 2.092315352667752038, -282.3727358251757096, -336.4970267429923183 ) ) ;
#25295 = CARTESIAN_POINT ( 'NONE',  ( 36.46426520696237361, -277.3869757330227799, -259.1161724500052514 ) ) ;
#25296 = CARTESIAN_POINT ( 'NONE',  ( 7.450504543161046378, -284.9090924074130839, -326.4764044574609443 ) ) ;
#25297 = CARTESIAN_POINT ( 'NONE',  ( -112.0845800623916659, -276.5341076636472053, -282.7630283427802738 ) ) ;
#25298 = DIRECTION ( 'NONE',  ( 0.000000000000000000, 0.000000000000000000, 1.000000000000000000 ) ) ;
#25299 = CARTESIAN_POINT ( 'NONE',  ( -76.16513041315916155, -283.0936099488778268, -332.3138420805906890 ) ) ;
#25300 = CARTESIAN_POINT ( 'NONE',  ( -99.93344424428246953, -280.3445826990167120, -226.1991174904782440 ) ) ;
#25301 = CARTESIAN_POINT ( 'NONE',  ( 39.40507359593098613, -286.5900875378303567, -268.7019208138915474 ) ) ;
#25302 = CARTESIAN_POINT ( 'NONE',  ( -57.95841259011505286, -293.5424550768269114, -199.2235717470466341 ) ) ;
#25303 = CARTESIAN_POINT ( 'NONE',  ( 20.22935160620968631, -277.8340848278626254, -320.3009533331063494 ) ) ;
#25304 = CARTESIAN_POINT ( 'NONE',  ( 33.25200280530626173, -276.4882719995125626, -240.7315256981000857 ) ) ;
#25305 = CARTESIAN_POINT ( 'NONE',  ( -53.95599249986268831, -277.1046166483944830, -341.4974718154298330 ) ) ;
#25306 = CARTESIAN_POINT ( 'NONE',  ( -106.9591993256848923, -274.8856171023163029, -243.2879330334971257 ) ) ;
#25307 = CARTESIAN_POINT ( 'NONE',  ( -52.43441197048003488, -283.8582324817880931, -197.0655623691760923 ) ) ;
#25308 = CARTESIAN_POINT ( 'NONE',  ( 23.09411230421855876, -292.5807809867879996, -222.6613691358707570 ) ) ;
#25309 = CARTESIAN_POINT ( 'NONE',  ( -48.72910882811514455, -290.7948378631049309, -345.7588251744553531 ) ) ;
#25310 = CARTESIAN_POINT ( 'NONE',  ( -47.02172961108180260, -290.8466296573629961, -197.6939100939247567 ) ) ;
#25311 = ORIENTED_EDGE ( 'NONE', *, *, #80735, .F. ) ;
#25312 = CARTESIAN_POINT ( 'NONE',  ( -3.565331672669104890, -291.0639237552227883, -201.8064587554073626 ) ) ;
#25313 = CARTESIAN_POINT ( 'NONE',  ( -25.40145526563462397, -291.8751199887706775, -198.2713144429138481 ) ) ;
#25314 = EDGE_LOOP ( 'NONE', ( #30460, #62937, #15656, #22615 ) ) ;
#25315 = CARTESIAN_POINT ( 'NONE',  ( -97.90699785994191018, -291.0009720746564881, -317.4072360133181974 ) ) ;
#25316 = CARTESIAN_POINT ( 'NONE',  ( -49.16655620748250044, -280.5488808362643454, -198.2219091803277706 ) ) ;
#25317 = CARTESIAN_POINT ( 'NONE',  ( -108.5962795115171389, -295.8353016186897548, -241.8586888524557423 ) ) ;
#25318 = CARTESIAN_POINT ( 'NONE',  ( -80.88732289647593632, -286.1297315218801032, -206.9163107511304815 ) ) ;
#25319 = CARTESIAN_POINT ( 'NONE',  ( 22.97267074852972613, -287.2449544024692045, -222.5078930308498002 ) ) ;
#25320 = CARTESIAN_POINT ( 'NONE',  ( -73.80367000584455184, -283.8835602847856308, -333.6849382195065914 ) ) ;
#25321 = CARTESIAN_POINT ( 'NONE',  ( -13.31626158342701771, -91.39965012445205161, -359.9159752948824007 ) ) ;
#25322 = CARTESIAN_POINT ( 'NONE',  ( 172.3846408709008244, 243.2224064566618438, -178.8072285208067740 ) ) ;
#25323 = CARTESIAN_POINT ( 'NONE',  ( 64.22521439624901518, 46.71045597819469464, -315.3326039784200248 ) ) ;
#25324 = CARTESIAN_POINT ( 'NONE',  ( -45.93719516178872198, -276.3609526216555423, -343.0666507131855383 ) ) ;
#25325 = CARTESIAN_POINT ( 'NONE',  ( -29.69479536131630582, -275.8735244326393854, -343.3214352640654283 ) ) ;
#25326 = CARTESIAN_POINT ( 'NONE',  ( -37.24736439065320326, -297.5609611697809100, -193.4219005745662798 ) ) ;
#25327 = CARTESIAN_POINT ( 'NONE',  ( -61.61208932556601070, -183.4966681853139221, -359.3482004706497150 ) ) ;
#25328 = CARTESIAN_POINT ( 'NONE',  ( -75.10743839796491272, -276.2293225812792343, -336.8971780247672996 ) ) ;
#25329 = CARTESIAN_POINT ( 'NONE',  ( -102.9388032797653807, -274.7736880993315935, -235.9718629566357038 ) ) ;
#25330 = VERTEX_POINT ( 'NONE', #32366 ) ;
#25331 = CARTESIAN_POINT ( 'NONE',  ( -97.39591930593921631, -290.4649665910751537, -311.9941417160450783 ) ) ;
#25332 = CARTESIAN_POINT ( 'NONE',  ( 30.60061854741075393, -299.6853369978908859, -193.5135760210463900 ) ) ;
#25333 = CARTESIAN_POINT ( 'NONE',  ( -109.7950203624954071, -297.3715044212949579, -244.4759235628065142 ) ) ;
#25334 = CARTESIAN_POINT ( 'NONE',  ( -66.05118267075141603, -295.6053306492599972, -337.4786687174667463 ) ) ;
#25335 = ORIENTED_EDGE ( 'NONE', *, *, #13517, .F. ) ;
#25336 = CARTESIAN_POINT ( 'NONE',  ( -73.38795866116659283, -279.4465274672778605, -336.7835283423722217 ) ) ;
#25337 = CARTESIAN_POINT ( 'NONE',  ( -16.16479937763233465, -282.2932702439318291, -344.3830112493215552 ) ) ;
#25338 = CARTESIAN_POINT ( 'NONE',  ( -7.400523337463443596, -277.5908462099307599, -337.1962463293898509 ) ) ;
#25339 = CARTESIAN_POINT ( 'NONE',  ( 35.52815801109034766, -277.5866408264053007, -291.9467515334152381 ) ) ;
#25340 = CARTESIAN_POINT ( 'NONE',  ( -69.49876373618745617, -296.1950756646697869, -204.1697425683345557 ) ) ;
#25341 = CARTESIAN_POINT ( 'NONE',  ( 175.2296996224750103, 20.99999999999998934, 0.000000000000000000 ) ) ;
#25342 = CARTESIAN_POINT ( 'NONE',  ( -106.4454159008273137, -279.0333888795598796, -246.6755423743570645 ) ) ;
#25343 = CARTESIAN_POINT ( 'NONE',  ( -67.48174188482548175, -274.4695436595636693, -199.6805923499918265 ) ) ;
#25344 = CARTESIAN_POINT ( 'NONE',  ( 39.11063933135869775, -286.2879884859008826, -274.4136205686718881 ) ) ;
#25345 = CARTESIAN_POINT ( 'NONE',  ( -5.974541806667331478, -276.4646038987892211, -202.2354838096020444 ) ) ;
#25346 = DIRECTION ( 'NONE',  ( 0.8571673007021122226, 0.000000000000000000, 0.5150380749100541555 ) ) ;
#25347 = CARTESIAN_POINT ( 'NONE',  ( -98.98330885496692133, -289.2054505400968765, -309.7681452801497244 ) ) ;
#25348 = CARTESIAN_POINT ( 'NONE',  ( -71.01410266429503793, -284.9679966495662029, -201.2273194856097120 ) ) ;
#25349 = EDGE_CURVE ( 'NONE', #10045, #89245, #65738, .T. ) ;
#25350 = CARTESIAN_POINT ( 'NONE',  ( 35.06111417893038151, -279.5914541263940123, -254.9446503329105838 ) ) ;
#25352 = CARTESIAN_POINT ( 'NONE',  ( -49.63573658191625526, -283.9741464484075664, -196.8908233047757790 ) ) ;
#25351 = CARTESIAN_POINT ( 'NONE',  ( 23.05810360897427103, -280.7081466267550809, -312.3996553762333974 ) ) ;
#25353 = CARTESIAN_POINT ( 'NONE',  ( -21.56074910916992593, -290.8501246887855700, -343.7346010612021132 ) ) ;
#25354 = CARTESIAN_POINT ( 'NONE',  ( -107.6116862006213779, -280.0363335076874591, -249.1653740100405798 ) ) ;
#25355 = DIRECTION ( 'NONE',  ( -0.000000000000000000, -1.000000000000000000, -0.000000000000000000 ) ) ;
#25356 = CARTESIAN_POINT ( 'NONE',  ( 16.67058882306360346, -279.2044453294562345, -216.5366382635107811 ) ) ;
#25357 = CARTESIAN_POINT ( 'NONE',  ( -5.477601988872035754, -294.4714841000851493, -202.4664944626865406 ) ) ;
#25358 = CARTESIAN_POINT ( 'NONE',  ( -110.7462384188004165, -277.0417893900952890, -250.6704779151933167 ) ) ;
#25359 = CARTESIAN_POINT ( 'NONE',  ( -39.15198378159497139, -277.7268825637064538, -343.4406331806724779 ) ) ;
#25360 = CARTESIAN_POINT ( 'NONE',  ( -22.07290868366385439, -284.8571383141285764, -343.9606589548379247 ) ) ;
#25361 = DIRECTION ( 'NONE',  ( 0.000000000000000000, 0.000000000000000000, 1.000000000000000000 ) ) ;
#25362 = CARTESIAN_POINT ( 'NONE',  ( -111.5161538510381547, -292.6567330799762772, -255.8899732335158603 ) ) ;
#25363 = CARTESIAN_POINT ( 'NONE',  ( 34.70637808644205791, -286.4109706138750084, -243.6546909327920787 ) ) ;
#25364 = CARTESIAN_POINT ( 'NONE',  ( -66.86560970675941462, -290.0585375724083974, -202.7240040591368029 ) ) ;
#25365 = CARTESIAN_POINT ( 'NONE',  ( -48.18343439340851830, -256.9335312097066435, -442.7126937774146427 ) ) ;
#25366 = CARTESIAN_POINT ( 'NONE',  ( -1.242509074817608861, -275.2477632188437724, -334.4350404483913621 ) ) ;
#25367 = CARTESIAN_POINT ( 'NONE',  ( 25.45977718219043595, -292.2305885300951900, -310.0409597163760509 ) ) ;
#25368 = DIRECTION ( 'NONE',  ( 1.000000000000000000, -0.000000000000000000, -0.000000000000000000 ) ) ;
#25369 = CARTESIAN_POINT ( 'NONE',  ( -111.3176030456619685, -289.2689422042759588, -251.5929453563863092 ) ) ;
#25370 = CARTESIAN_POINT ( 'NONE',  ( -110.6651808524029690, -286.0372916144630722, -279.1738967997951022 ) ) ;
#25371 = CARTESIAN_POINT ( 'NONE',  ( -8.636979200828667658, -286.9215176330077952, -340.7315233392874916 ) ) ;
#25372 = EDGE_CURVE ( 'NONE', #67402, #9610, #84399, .T. ) ;
#25373 = CARTESIAN_POINT ( 'NONE',  ( 35.54649439789385212, -289.1112386519912434, -280.5864364919723357 ) ) ;
#25374 = FACE_OUTER_BOUND ( 'NONE', #46111, .T. ) ;
#25375 = CARTESIAN_POINT ( 'NONE',  ( 35.81674259387337145, -288.3637602753262854, -271.0274399146314295 ) ) ;
#25376 = CARTESIAN_POINT ( 'NONE',  ( 28.15775018440013611, -296.0276461010991511, -307.7255312880222391 ) ) ;
#25377 = CARTESIAN_POINT ( 'NONE',  ( -90.33683986780398811, -275.8743505305516805, -324.2937606923914018 ) ) ;
#25378 = CARTESIAN_POINT ( 'NONE',  ( -109.7154302119714373, -278.5523456022054916, -296.7427303703722714 ) ) ;
#25379 = CARTESIAN_POINT ( 'NONE',  ( -66.43791542598705746, -289.7539504066996869, -200.6278801774358556 ) ) ;
#25380 = CARTESIAN_POINT ( 'NONE',  ( -114.0438979584680226, -278.6440389501078130, -263.0139254115716199 ) ) ;
#25381 = CARTESIAN_POINT ( 'NONE',  ( -39.23475806822107614, -300.0082013522594480, -195.7276342458387148 ) ) ;
#25382 = CARTESIAN_POINT ( 'NONE',  ( -48.18343439338961076, -261.4749445206144856, -499.9176714739165277 ) ) ;
#25383 = CARTESIAN_POINT ( 'NONE',  ( -112.3919468259040855, -282.5450820974854196, -270.8988963351653751 ) ) ;
#25384 = CARTESIAN_POINT ( 'NONE',  ( -48.18343439339133027, -283.1093320178187582, -502.6442049081569508 ) ) ;
#25385 = CARTESIAN_POINT ( 'NONE',  ( -101.8740739154087009, -277.1859463547153837, -233.6672736551553839 ) ) ;
#25386 = CARTESIAN_POINT ( 'NONE',  ( 30.23089727730868503, -279.1220303880001552, -237.7001221877023625 ) ) ;
#25387 = DIRECTION ( 'NONE',  ( 1.000000000000000000, -0.000000000000000000, 0.000000000000000000 ) ) ;
#25388 = CARTESIAN_POINT ( 'NONE',  ( 16.45258848134471918, -274.7848160669978483, -324.5540293011601989 ) ) ;
#25389 = CARTESIAN_POINT ( 'NONE',  ( -109.4616437019882795, -298.2709844495605580, -255.1536994388734456 ) ) ;
#25390 = CARTESIAN_POINT ( 'NONE',  ( 1.924017938745252287, -281.4598917350016904, -336.2374862363736270 ) ) ;
#25391 = CARTESIAN_POINT ( 'NONE',  ( -104.1463484580092569, -297.0889874438032621, -300.4941583035100621 ) ) ;
#25392 = CARTESIAN_POINT ( 'NONE',  ( -113.8175555806980412, -297.9124606077208455, -266.7752044999442660 ) ) ;
#25393 = CARTESIAN_POINT ( 'NONE',  ( -24.58857008613662387, -273.8859802979326332, -198.4106603393156831 ) ) ;
#25394 = CARTESIAN_POINT ( 'NONE',  ( 20.88276312212021324, -294.9010370225440738, -223.0659537655007227 ) ) ;
#25395 = CARTESIAN_POINT ( 'NONE',  ( 12.07595248769084861, -286.8838986166870200, -211.2416021627170721 ) ) ;
#25396 = CARTESIAN_POINT ( 'NONE',  ( 20.76777738762629255, -274.3567082443536833, -318.9779268699946329 ) ) ;
#25397 = CARTESIAN_POINT ( 'NONE',  ( -20.49847264130503177, -288.6750686911897787, -345.5510342762020173 ) ) ;
#25398 = CARTESIAN_POINT ( 'NONE',  ( 29.02823163649771487, -286.1942101750606753, -239.4024260699484898 ) ) ;
#25399 = AXIS2_PLACEMENT_3D ( 'NONE', #56152, #70375, #83600 ) ;
#25400 = CARTESIAN_POINT ( 'NONE',  ( -110.6788002138020488, -288.7543947931842467, -254.5948808906440206 ) ) ;
#25401 = ORIENTED_EDGE ( 'NONE', *, *, #93547, .T. ) ;
#25402 = CARTESIAN_POINT ( 'NONE',  ( 9.093980818847771985, -59.61193948127866094, -357.4272672779520121 ) ) ;
#25403 = CARTESIAN_POINT ( 'NONE',  ( -56.08742402907907376, -288.8077049740932125, -341.0294855659019504 ) ) ;
#25404 = CARTESIAN_POINT ( 'NONE',  ( 165.2424497756046549, 249.5000000000000568, 22.91843887563435800 ) ) ;
#25405 = CARTESIAN_POINT ( 'NONE',  ( -111.9875264138401292, -285.2680066179402729, -288.3281988650538210 ) ) ;
#25406 = CARTESIAN_POINT ( 'NONE',  ( -5.972087058750113364, -291.5132298220748908, -200.2842743670373409 ) ) ;
#25407 = CARTESIAN_POINT ( 'NONE',  ( 32.43215797779591014, -282.7575677097264020, -239.7335301161027985 ) ) ;
#25408 = CARTESIAN_POINT ( 'NONE',  ( 19.74945074723329341, -282.1721589617825998, -219.4110920227378756 ) ) ;
#25409 = CARTESIAN_POINT ( 'NONE',  ( -48.33077754406365756, -283.0292425886395904, -342.5292562572490738 ) ) ;
#25410 = CARTESIAN_POINT ( 'NONE',  ( -23.94808513997843491, -278.8813625854842826, -344.2083690371267153 ) ) ;
#25411 = CARTESIAN_POINT ( 'NONE',  ( -78.20246349483095116, -297.5186664069001949, -205.0970542331542674 ) ) ;
#25412 = CARTESIAN_POINT ( 'NONE',  ( -103.6572200806989628, -274.2928604961148835, -238.6831242018080843 ) ) ;
#25413 = CARTESIAN_POINT ( 'NONE',  ( -16.95979391574139328, -290.3365969262440558, -198.4990851546085651 ) ) ;
#25414 = UNCERTAINTY_MEASURE_WITH_UNIT (LENGTH_MEASURE( 1.000000000000000082E-05 ), #24432, 'distance_accuracy_value', 'NONE');
#25415 = CARTESIAN_POINT ( 'NONE',  ( -90.47351426350603276, -272.0735781127592077, -219.7053883047262275 ) ) ;
#25416 = VERTEX_POINT ( 'NONE', #55550 ) ;
#25417 = DIRECTION ( 'NONE',  ( 1.000000000000000000, 0.000000000000000000, 0.000000000000000000 ) ) ;
#25418 = CARTESIAN_POINT ( 'NONE',  ( -83.67222396746511492, -285.6132797491057431, -328.6921287446546671 ) ) ;
#25419 = CARTESIAN_POINT ( 'NONE',  ( 25.46941863734217648, -295.2162608897929204, -314.3869496283570584 ) ) ;
#25420 = CARTESIAN_POINT ( 'NONE',  ( -95.04262091548704916, -285.8352853148911095, -225.4576477110521466 ) ) ;
#25421 = CARTESIAN_POINT ( 'NONE',  ( 5.729328823447515262, -275.5426119433953431, -333.9040694209037952 ) ) ;
#25422 = CARTESIAN_POINT ( 'NONE',  ( -86.45431405527689606, -292.0424002502364829, -211.1204927577868204 ) ) ;
#25423 = CARTESIAN_POINT ( 'NONE',  ( -112.5900617009342284, -282.8039838590052568, -261.5299481777547044 ) ) ;
#25424 = CARTESIAN_POINT ( 'NONE',  ( -5.899457512176192964, -292.7875569025314917, -200.0821225246380948 ) ) ;
#25425 = CARTESIAN_POINT ( 'NONE',  ( -108.1300205867590165, -291.1224743035724032, -252.3909564375660466 ) ) ;
#25426 = DIRECTION ( 'NONE',  ( 0.000000000000000000, 0.000000000000000000, 1.000000000000000000 ) ) ;
#25427 = CARTESIAN_POINT ( 'NONE',  ( -83.63170945779077670, -298.0521521680024080, -421.1172536214571096 ) ) ;
#25428 = CARTESIAN_POINT ( 'NONE',  ( -69.56015552319689732, -196.2844319401296218, -356.7998354135015120 ) ) ;
#25429 = CARTESIAN_POINT ( 'NONE',  ( -85.09422673512297308, -286.9265702216204090, -210.8430202850986461 ) ) ;
#25430 = CARTESIAN_POINT ( 'NONE',  ( -99.86837403722181250, -270.6952119285918457, -220.4570493818173702 ) ) ;
#25431 = ORIENTED_EDGE ( 'NONE', *, *, #12195, .F. ) ;
#25432 = CARTESIAN_POINT ( 'NONE',  ( 19.92607102360820193, -279.8286444439469847, -224.5940068429489145 ) ) ;
#25433 = CARTESIAN_POINT ( 'NONE',  ( -41.38757935571820212, -276.7684760752744637, -347.2467834828916580 ) ) ;
#25434 = CARTESIAN_POINT ( 'NONE',  ( -99.53103344926849161, -281.1173109067062228, -228.6455674257470037 ) ) ;
#25435 = CARTESIAN_POINT ( 'NONE',  ( 123.3664110013779123, 147.4260113058992658, -261.7119338772159267 ) ) ;
#25436 = CARTESIAN_POINT ( 'NONE',  ( -24.64946485751858063, -281.4681075383765005, -345.7640942132951523 ) ) ;
#25437 = CARTESIAN_POINT ( 'NONE',  ( -102.4130865246282127, -283.0629160738077417, -233.6825652546871481 ) ) ;
#25438 = CARTESIAN_POINT ( 'NONE',  ( -40.42192789263766173, -299.7742003127527823, -194.3854649232285112 ) ) ;
#25439 = B_SPLINE_SURFACE_WITH_KNOTS ( 'NONE', 3, 3, ( 
 ( #44293, #38110, #8320, #88774, #36733, #1679, #58987, #87835, #37202, #23922, #16819, #22986, #767, #79828, #67020, #29652, #51860, #88310, #45677, #50945, #58532, #25321, #46156, #3548, #38592, #54201, #68418, #11580, #54658, #39496, #69346, #10637, #40428, #67495, #18691, #82613, #9711, #82144, #2626, #47073 ),
 ( #47554, #26256, #3077, #39041, #18223, #53747, #83069, #31505, #19160, #32437, #33353, #60393, #89231, #24383, #4476, #83532, #53262, #17300, #75515, #11108, #61336, #39975, #89698, #90173, #91085, #75060, #46614, #10171, #67952, #74584, #4020, #75980, #31961, #60855, #68890, #62250, #24864, #17760, #32895, #61783 ),
 ( #90615, #25776, #76459, #55150, #84012, #6361, #35711, #20090, #33837, #12525, #49897, #34307, #40897, #63213, #5899, #77387, #27675, #78792, #13935, #28150, #41375, #92992, #57039, #62746, #85877, #71234, #21029, #5440, #48971, #35234, #69815, #42794, #64159, #4951, #92045, #70309, #91578, #64625, #93451, #27199 ),
 ( #71710, #55621, #26734, #28606, #84470, #6837, #57495, #19620, #56086, #48488, #86338, #13476, #84938, #56573, #70766, #85426, #48017, #76922, #77867, #13017, #12050, #41853, #34769, #63684, #92507, #20574, #49446, #78334, #42323, #58879, #43721, #79725, #8659, #52220, #57956, #80179, #86811, #50842, #14867, #66899 ),
 ( #36622, #8214, #37991, #43270, #87269, #7284, #21969, #21488, #44649, #1113, #79272, #72619, #44176, #81103, #65544, #7741, #37092, #66001, #659, #9115, #29543, #72168, #80634, #14412, #29994, #58423, #15790, #59341, #22415, #51287, #87725, #15317, #2039, #73083, #73550, #22876, #88193, #51741, #65083, #73998 ),
 ( #30449, #36162, #1566, #37537, #23353, #66448, #16246, #45096, #183, #30929, #59819, #29064, #50368, #53141, #9589, #76338, #11464, #74947, #4359, #16701, #3902, #2511, #45556, #40315, #74456, #39850, #33236, #31388, #10057, #38477, #18103, #54079, #60278, #32316, #17648, #61219, #88660, #23809, #89576, #82021 ),
 ( #89115, #52672, #25659, #82949, #75858, #46956, #17178, #68773, #31847, #90053, #46042, #24266, #38927, #10980, #81553, #69230, #32779, #67381, #61667, #67836, #2961, #60736, #53630, #90499, #82500, #46499, #75402, #25206, #10516, #54541, #39385, #68300, #83409, #47428, #18561, #90963, #26127, #56921, #42195, #55023 ),
 ( #62132, #63092, #26610, #64028, #28032, #83893, #19044, #34188, #34649, #19499, #91920, #47900, #5775, #84350, #55501, #49320, #92869, #4824, #27075, #33707, #6240, #70186, #76802, #69695, #11928, #63561, #49779, #77744, #84815, #35109, #62619, #91459, #85760, #92388, #78675, #55961, #27548, #71584, #48366, #77269 ),
 ( #20910, #71108, #12398, #41244, #19965, #56441, #48838, #85304, #5320, #12895, #13816, #41733, #70647, #20453, #78215, #13354, #42668, #6721, #69593, #62509, #55399, #12297, #91349, #26510, #84251, #19402, #48265, #4723, #77167, #33601, #30436, #29051, #15777, #73070, #59328, #9101, #37080, #87256, #37523, #7729 ),
 ( #22863, #647, #44635, #2025, #30917, #45083, #58410, #16233, #73984, #79713, #37978, #88179, #66886, #22402, #65989, #52207, #57943, #59806, #81089, #86798, #80167, #29530, #14855, #52659, #81539, #51274, #74443, #21956, #88647, #72607, #50829, #16687, #43708, #23795, #9575, #36610, #15305, #65530, #23339, #45542 ),
 ( #87712, #73537, #65072, #171, #1100, #44164, #8201, #29981, #58865, #51728, #80621, #8646, #66433, #1553, #69218, #4347, #18548, #31834, #83398, #47416, #53127, #76326, #61655, #11451, #89564, #10502, #25646, #31375, #40303, #54529, #60264, #53617, #2948, #82007, #26115, #55009, #24734, #47886, #89101, #33224 ),
 ( #83882, #24253, #62120, #76790, #74934, #82487, #17164, #90488, #3890, #10044, #46943, #61206, #75845, #38464, #67368, #39371, #60725, #90951, #19032, #46029, #2497, #68287, #10968, #17635, #3408, #38914, #39836, #46486, #75389, #67823, #32300, #90041, #25193, #54067, #82937, #18089, #68760, #32767, #33694, #78204 ),
 ( #49771, #58645, #34177, #70173, #49310, #84805, #20442, #62605, #51509, #70637, #64500, #91448, #40765, #69683, #6712, #85752, #4813, #55488, #12884, #42184, #41721, #71097, #27063, #92378, #29766, #26598, #77733, #84337, #48354, #11916, #35100, #85292, #19488, #77257, #34639, #42659, #55950, #5308, #27537, #56430 ),
 ( #12387, #41233, #63079, #91909, #5765, #78666, #19955, #63549, #92858, #13343, #48826, #6230, #64018, #28022, #56912, #20899, #13807, #71576, #35586, #93326, #87487, #22637, #16472, #17420, #44414, #88435, #46269, #66219, #80872, #80397, #75173, #45800, #67611, #9831, #73773, #31619, #23584, #24035, #37766, #51983 ),
 ( #45327, #23101, #24500, #52451, #15542, #87949, #8433, #52911, #68068, #2280, #9348, #53382, #1334, #16020, #82267, #81789, #3193, #81325, #74710, #89825, #44871, #8887, #60510, #16938, #10286, #38704, #74229, #66671, #1799, #32077, #2739, #73322, #30684, #89345, #39156, #59584, #60976, #30216, #24986, #38233 ),
 ( #37312, #67146, #31163, #59107, #60049, #88887, #69464, #40549, #11237, #41497, #54313, #75632, #19276, #17877, #4596, #61901, #48134, #91695, #25894, #76104, #26383, #90284, #70427, #90735, #77037, #33469, #26847, #40092, #3674, #12652, #55271, #82725, #84126, #83188, #46729, #61453, #54776, #69934, #83653, #48605 ),
 ( #41011, #10755, #69008, #18335, #68536, #5553, #34423, #4139, #63330, #92161, #62372, #76575, #55735, #39612, #25435, #84587, #12168, #53859, #18817, #5076, #32561, #47191, #33010, #33958, #91215, #19737, #62862, #47674, #11698, #77505, #72731, #43380, #56204, #49555, #50486, #22081, #56690, #72275, #70880, #50951 ),
 ( #34886, #21605, #42438, #93107, #21141, #86928, #28262, #71348, #7394, #64278, #6011, #63797, #92626, #49092, #57150, #79388, #14974, #85991, #13131, #85537, #29179, #13586, #20214, #6479, #78904, #20684, #6947, #58075, #79834, #36275, #78450, #65196, #299, #41967, #43830, #14525, #7852, #35356, #50011, #36739 ),
 ( #35820, #14051, #42914, #71828, #65660, #27318, #64734, #27797, #93561, #85063, #28719, #57604, #77990, #86447, #58538, #29658, #45215, #66116, #23474, #87383, #74117, #88317, #31511, #74590, #59465, #89237, #30567, #60399, #22530, #8778, #24390, #80293, #1229, #774, #53268, #59941, #81677, #23928, #87842, #45683 ),
 ( #58993, #16826, #82151, #37208, #52340, #30111, #38598, #37656, #51402, #8326, #15432, #67026, #22992, #1686, #9718, #81218, #44299, #73207, #9237, #51866, #16364, #80759, #38116, #2162, #17306, #67501, #31051, #46163, #88780, #75066, #15911, #66564, #10177, #44767, #73667, #52798, #39047, #2632, #55156, #91091 ),
 ( #11587, #90179, #32443, #84018, #4957, #10643, #32901, #39503, #12056, #75986, #3083, #75521, #89704, #40434, #55627, #83538, #90621, #40903, #53753, #68424, #69823, #69352, #84476, #39981, #33359, #77394, #61344, #25327, #19166, #4482, #33843, #62257, #61789, #3554, #54207, #19626, #48023, #31968, #83075, #26262 ),
 ( #76928, #17766, #62752, #18229, #67958, #47080, #91584, #11114, #68896, #25783, #26741, #4028, #54665, #48495, #18697, #46620, #47560, #76465, #24871, #12531, #60861, #82619, #13482, #27205, #5905, #43276, #27681, #34313, #56579, #92998, #70772, #21035, #72174, #7290, #21496, #34775, #86345, #50374, #56092, #79278 ),
 ( #78340, #57501, #42329, #36168, #13023, #49903, #64166, #6369, #71240, #65089, #86816, #35240, #77874, #20096, #14419, #6843, #63219, #57962, #35717, #84946, #189, #63690, #92515, #85432, #21974, #29070, #50847, #20580, #49452, #78798, #28156, #13943, #92051, #79730, #57045, #41381, #48978, #70315, #41859, #85883 ),
 ( #42800, #71716, #64631, #93457, #28612, #43726, #37098, #37998, #9597, #44184, #30935, #58429, #38484, #30000, #14872, #22421, #9121, #58885, #80642, #8666, #74464, #15797, #87731, #88666, #51750, #87275, #51293, #80185, #36629, #44656, #66907, #2518, #73557, #665, #73090, #16707, #1119, #7746, #22883, #66455 ),
 ( #45562, #67388, #23815, #8220, #59825, #52678, #29549, #81559, #2046, #31395, #66007, #37544, #60285, #65551, #89122, #24273, #15323, #1572, #30455, #59349, #53148, #72624, #88200, #23359, #52226, #81109, #16252, #45102, #74004, #67843, #33245, #91467, #24755, #3429, #38934, #11472, #47437, #53637, #90507, #10989 ) ),
 .UNSPECIFIED., .F., .F., .F.,
 ( 4, 3, 3, 3, 3, 3, 3, 3, 4 ),
 ( 4, 3, 3, 3, 3, 3, 3, 3, 3, 3, 3, 3, 3, 4 ),
 ( -3.330669073875469621E-15, 0.06249999999999708566, 0.1249999999999975020, 0.1874999999999979183, 0.2499999999999983347, 0.3124999999999987788, 0.3749999999999991673, 0.4374999999999995559, 0.5000000000000000000 ),
 ( -7.331489042931211300E-13, 0.06249999999910264836, 0.1249999999989384464, 0.1874999999987742305, 0.2499999999986100285, 0.3749999999982815968, 0.4999999999979531928, 0.6249999999976247889, 0.6874999999974605869, 0.7499999999972963849, 0.8124999999971321829, 0.8749999999969679809, 0.9374999999968037789, 0.9999999999966395769 ),
 .UNSPECIFIED. ) ;
#25440 = CARTESIAN_POINT ( 'NONE',  ( -5.509032888388956550, -295.1140799928280103, -336.1371621343747620 ) ) ;
#25441 = EDGE_LOOP ( 'NONE', ( #83264, #71223, #50033, #74140, #54424 ) ) ;
#25442 = CARTESIAN_POINT ( 'NONE',  ( -25.31198342667658707, -290.8933852086360048, -197.8073629383141565 ) ) ;
#25443 = CARTESIAN_POINT ( 'NONE',  ( 37.49459235954292069, -276.4257125213072754, -288.1052055941094636 ) ) ;
#25444 = CARTESIAN_POINT ( 'NONE',  ( 26.63652656261450247, -275.0707052991883756, -235.1020089541326570 ) ) ;
#25445 = CARTESIAN_POINT ( 'NONE',  ( 15.82268886041457812, -273.7045411421397603, -215.0886994298425350 ) ) ;
#25446 = FACE_OUTER_BOUND ( 'NONE', #86109, .T. ) ;
#25447 = CARTESIAN_POINT ( 'NONE',  ( -99.68310566211027890, -271.1166714750369806, -228.5733690296224268 ) ) ;
#25448 = CARTESIAN_POINT ( 'NONE',  ( 6.292525700994897164, -295.8980229839523304, -333.1524725929577926 ) ) ;
#25449 = CARTESIAN_POINT ( 'NONE',  ( 154.1407330040854333, 128.0000000000000568, 13.42592592592592737 ) ) ;
#25450 = CARTESIAN_POINT ( 'NONE',  ( 199.2296996224019381, 66.10105075032892330, 2.340466192621719177 ) ) ;
#25451 = CARTESIAN_POINT ( 'NONE',  ( 31.65015953459397124, -282.9623050531744184, -295.2973613425602366 ) ) ;
#25452 = CARTESIAN_POINT ( 'NONE',  ( 35.62036314281331784, -283.0420285402008176, -249.0892671829823541 ) ) ;
#25453 = CARTESIAN_POINT ( 'NONE',  ( -106.6262642408735388, -284.2118868329184238, -246.8886854162517182 ) ) ;
#25454 = CARTESIAN_POINT ( 'NONE',  ( -68.39236274638071222, -275.8668823817476436, -337.3249755719738801 ) ) ;
#25455 = CARTESIAN_POINT ( 'NONE',  ( 4.099072374511927741, -284.3480798981710791, -332.0149324341556394 ) ) ;
#25456 = CARTESIAN_POINT ( 'NONE',  ( -102.4787064723253849, -276.5669855688445864, -304.8267262778476834 ) ) ;
#25457 = CARTESIAN_POINT ( 'NONE',  ( 35.68483565052919460, -276.5400946109438109, -263.3776813487488084 ) ) ;
#25458 = DIRECTION ( 'NONE',  ( 2.940294503956655304E-16, -0.000000000000000000, 1.000000000000000000 ) ) ;
#25459 = CARTESIAN_POINT ( 'NONE',  ( -114.0702159846059942, -279.3034715394155114, -274.4713095234498041 ) ) ;
#25460 = VERTEX_POINT ( 'NONE', #68823 ) ;
#25461 = CARTESIAN_POINT ( 'NONE',  ( 202.9738562182569694, 293.9636489450776367, -40.00000000000000711 ) ) ;
#25462 = CARTESIAN_POINT ( 'NONE',  ( -111.7891118326123205, -286.5947931372634798, -256.0204010818362121 ) ) ;
#25463 = CARTESIAN_POINT ( 'NONE',  ( -100.3106522776319878, -295.2374354079971681, -307.7102269042525222 ) ) ;
#25464 = CARTESIAN_POINT ( 'NONE',  ( -110.3315174758904078, -290.2076818926813075, -245.9912452338584501 ) ) ;
#25465 = ADVANCED_FACE ( 'NONE', ( #19095 ), #3496, .F. ) ;
#25466 = CARTESIAN_POINT ( 'NONE',  ( 34.99103750803095636, -285.5879606625928204, -254.6783541169293414 ) ) ;
#25468 = CARTESIAN_POINT ( 'NONE',  ( -111.3505679452838137, -288.7814211044070021, -271.1744416007073823 ) ) ;
#25467 = CARTESIAN_POINT ( 'NONE',  ( -38.61706088930186809, -284.6106107942260337, -196.7703566605917729 ) ) ;
#25469 = VECTOR ( 'NONE', #43320, 1000.000000000000000 ) ;
#25470 = CARTESIAN_POINT ( 'NONE',  ( -108.7554054368453080, -285.9802409594319101, -253.3595753269164561 ) ) ;
#25471 = CARTESIAN_POINT ( 'NONE',  ( -31.62870805527227702, -274.9799995327869624, -345.1944739464025247 ) ) ;
#25472 = CARTESIAN_POINT ( 'NONE',  ( 37.50822985570060553, -285.7715584961492823, -256.0807678992746901 ) ) ;
#25473 = CARTESIAN_POINT ( 'NONE',  ( -26.92476022374850686, -288.1846429863961134, -196.0359461834780461 ) ) ;
#25474 = CARTESIAN_POINT ( 'NONE',  ( 11.21173076402869562, -286.3811501699633482, -327.7422365859876550 ) ) ;
#25475 = CARTESIAN_POINT ( 'NONE',  ( -30.25149832316010645, -281.0851610841808110, -197.4193289838501073 ) ) ;
#25476 = CARTESIAN_POINT ( 'NONE',  ( -67.29923345947612745, -291.4442404984839072, -339.3000375110531195 ) ) ;
#25477 = DIRECTION ( 'NONE',  ( -0.000000000000000000, -0.000000000000000000, -1.000000000000000000 ) ) ;
#25478 = FACE_OUTER_BOUND ( 'NONE', #17602, .T. ) ;
#25479 = CARTESIAN_POINT ( 'NONE',  ( -108.9726681848178202, -298.1636975270963035, -294.4093738988105997 ) ) ;
#25480 = CARTESIAN_POINT ( 'NONE',  ( -70.60499417502440167, -277.6134202932714743, -203.1267063012960818 ) ) ;
#25481 = CARTESIAN_POINT ( 'NONE',  ( -44.87102674738007835, -291.1564412950571068, -193.8395676426056582 ) ) ;
#25482 = CARTESIAN_POINT ( 'NONE',  ( -75.60821979140706617, -295.9326490227792874, -207.1978848992800977 ) ) ;
#25483 = CARTESIAN_POINT ( 'NONE',  ( 33.59394399054472302, -279.9842275965743283, -251.0937228892536268 ) ) ;
#25484 = CARTESIAN_POINT ( 'NONE',  ( -65.08316163842918911, -271.7667198546649843, -201.2696970755833661 ) ) ;
#25485 = CARTESIAN_POINT ( 'NONE',  ( 24.85347470641512757, -295.4056666720099429, -309.6103381518848892 ) ) ;
#25486 = CARTESIAN_POINT ( 'NONE',  ( -114.2704648735229114, -287.0519495502702512, -270.3937649182068981 ) ) ;
#25487 = CARTESIAN_POINT ( 'NONE',  ( -102.2091707222743082, -271.6592913489806733, -229.9777358706982966 ) ) ;
#25488 = CARTESIAN_POINT ( 'NONE',  ( 29.99388428293444164, -292.2523819729739785, -305.5732335597014639 ) ) ;
#25489 = ADVANCED_FACE ( 'NONE', ( #83461 ), #4876, .T. ) ;
#25490 = CARTESIAN_POINT ( 'NONE',  ( 19.79187067718770265, -294.3262418708314954, -223.9609186868267727 ) ) ;
#25491 = DIRECTION ( 'NONE',  ( 0.000000000000000000, 0.000000000000000000, -1.000000000000000000 ) ) ;
#25492 = CARTESIAN_POINT ( 'NONE',  ( 34.99921143403249602, -294.5031536899988964, -281.6177096995916713 ) ) ;
#25493 = LINE ( 'NONE', #12714, #2104 ) ;
#25495 = CARTESIAN_POINT ( 'NONE',  ( -39.68903769236293044, -295.0824154072274723, -343.3357989888760926 ) ) ;
#25494 = CARTESIAN_POINT ( 'NONE',  ( -89.32219838708532222, -281.7992011353934458, -324.9893994723233277 ) ) ;
#25496 = CARTESIAN_POINT ( 'NONE',  ( 9.208804488454413573, -282.4323998628255481, -331.6966747171807697 ) ) ;
#25497 = CARTESIAN_POINT ( 'NONE',  ( -83.87379996095796741, -283.3380133866291430, -331.7510615724602303 ) ) ;
#25498 = CARTESIAN_POINT ( 'NONE',  ( -76.85793325261528253, -287.5825399555865260, -333.9102780500822973 ) ) ;
#25499 = CARTESIAN_POINT ( 'NONE',  ( -83.63170945779077670, -298.0521521680024080, -417.1172536214571096 ) ) ;
#25500 = CARTESIAN_POINT ( 'NONE',  ( 36.32082713823489684, -279.7798286983633602, -250.3982111275191471 ) ) ;
#25501 = CARTESIAN_POINT ( 'NONE',  ( 20.33132837980222618, -287.1593480809937091, -320.9310140225105101 ) ) ;
#25502 = DIRECTION ( 'NONE',  ( 0.000000000000000000, 0.000000000000000000, 1.000000000000000000 ) ) ;
#25503 = CARTESIAN_POINT ( 'NONE',  ( -66.34901754743862057, -297.0385473537887719, -338.2213858319584006 ) ) ;
#25504 = CARTESIAN_POINT ( 'NONE',  ( -4.233606403759325509, -278.0495042174313767, -339.2410320296824580 ) ) ;
#25505 = CARTESIAN_POINT ( 'NONE',  ( -54.49363932420450141, -279.4925008586195077, -199.3307516649444722 ) ) ;
#25506 = CARTESIAN_POINT ( 'NONE',  ( -22.19586651930662669, -292.4075374037363986, -194.8110721692961533 ) ) ;
#25507 = CARTESIAN_POINT ( 'NONE',  ( -41.51453533694849085, -281.1840301448403920, -345.8571577947228661 ) ) ;
#25508 = EDGE_CURVE ( 'NONE', #42443, #2063, #3475, .T. ) ;
#25509 = CARTESIAN_POINT ( 'NONE',  ( -45.40851032513277374, -279.1543904687937356, -344.9777172841940001 ) ) ;
#25510 = CARTESIAN_POINT ( 'NONE',  ( 11.09538014014875529, -291.8008182981295136, -215.3638676092463413 ) ) ;
#25511 = CARTESIAN_POINT ( 'NONE',  ( -107.0207933031602607, -294.9149607289440951, -242.4759629644131564 ) ) ;
#25512 = VERTEX_POINT ( 'NONE', #32826 ) ;
#25513 = DIRECTION ( 'NONE',  ( 0.000000000000000000, 0.000000000000000000, 1.000000000000000000 ) ) ;
#25514 = CARTESIAN_POINT ( 'NONE',  ( -0.7325421533888573089, -294.0597661249677799, -333.6466836809093479 ) ) ;
#25515 = CARTESIAN_POINT ( 'NONE',  ( 199.4819116658660221, 63.22432295887224285, 9.188210044104504703 ) ) ;
#25516 = CARTESIAN_POINT ( 'NONE',  ( 27.36219212280433055, -284.6237833571632905, -239.2376011013261916 ) ) ;
#25517 = CARTESIAN_POINT ( 'NONE',  ( 7.829102318185203302, -297.6634640464585004, -193.6034160913901303 ) ) ;
#25518 = CARTESIAN_POINT ( 'NONE',  ( 37.64531262887317808, -279.8293697398389099, -281.1894788128539062 ) ) ;
#25519 = CARTESIAN_POINT ( 'NONE',  ( -80.67278071948570073, -286.7933854495593096, -207.2438859192855602 ) ) ;
#25520 = CARTESIAN_POINT ( 'NONE',  ( -80.40921654590333389, -289.4872022119089934, -329.3662731293612183 ) ) ;
#25521 = CARTESIAN_POINT ( 'NONE',  ( -56.76444268348722488, -278.8271484498646373, -341.5018364171720577 ) ) ;
#25522 = CARTESIAN_POINT ( 'NONE',  ( -111.1424585658010642, -274.1879552814814929, -267.6277344828209266 ) ) ;
#25523 = CARTESIAN_POINT ( 'NONE',  ( -43.25429243011743097, -275.9233979841557129, -343.5196564948855666 ) ) ;
#25524 = ORIENTED_EDGE ( 'NONE', *, *, #80334, .T. ) ;
#25525 = CARTESIAN_POINT ( 'NONE',  ( -85.19995602203759688, -297.0782090278889314, -210.0674065839109517 ) ) ;
#25526 = CARTESIAN_POINT ( 'NONE',  ( -110.0643454393489122, -292.2659387964840221, -286.3178005973772429 ) ) ;
#25527 = CARTESIAN_POINT ( 'NONE',  ( 18.95257534434676927, -295.8584623611468487, -321.7935722638098923 ) ) ;
#25528 = CARTESIAN_POINT ( 'NONE',  ( 199.2296996224750103, 68.12454877784578855, -2.107038703920835587 ) ) ;
#25529 = CARTESIAN_POINT ( 'NONE',  ( -101.7290033820603554, -290.7309109456960527, -305.0829804833109051 ) ) ;
#25530 = CARTESIAN_POINT ( 'NONE',  ( -48.18343439339133027, -252.9280701297265637, -448.2498469311837539 ) ) ;
#25531 = CARTESIAN_POINT ( 'NONE',  ( -44.75226758132235005, -290.0990284552033245, -194.9075265247618063 ) ) ;
#25532 = CIRCLE ( 'NONE', #27103, 203.9779373800640485 ) ;
#25533 = CARTESIAN_POINT ( 'NONE',  ( -36.18904121649769934, -298.3994932829491518, -193.3821985998950197 ) ) ;
#25534 = CARTESIAN_POINT ( 'NONE',  ( -110.4053383380896634, -296.2043874184640231, -271.4592006400954460 ) ) ;
#25535 = DIRECTION ( 'NONE',  ( 8.659560562352529298E-17, 0.7071067811867438602, -0.7071067811863512853 ) ) ;
#25536 = CARTESIAN_POINT ( 'NONE',  ( -77.75265931866277924, -291.1040618683761636, -335.1503460392802367 ) ) ;
#25537 = CARTESIAN_POINT ( 'NONE',  ( -72.02372285203398405, -297.9805209788416391, -342.4524372437778652 ) ) ;
#25538 = CARTESIAN_POINT ( 'NONE',  ( -105.1573998014192171, -286.9705025672874967, -238.5986683071902235 ) ) ;
#25539 = CARTESIAN_POINT ( 'NONE',  ( -54.61048727381081136, -271.8295515885110945, -197.5475381097988645 ) ) ;
#25540 = CARTESIAN_POINT ( 'NONE',  ( -92.19996849581345089, -275.1806113581057502, -220.0244057253776759 ) ) ;
#25541 = CARTESIAN_POINT ( 'NONE',  ( -55.33725925972116499, -289.8986734863300967, -198.1290333769163112 ) ) ;
#25542 = CARTESIAN_POINT ( 'NONE',  ( -112.9973048250349734, -280.3608846345426286, -274.4274377017377446 ) ) ;
#25543 = ORIENTED_EDGE ( 'NONE', *, *, #86873, .F. ) ;
#25544 = CARTESIAN_POINT ( 'NONE',  ( -3.581672725288374437, -281.9428431318284538, -335.2145838333082111 ) ) ;
#25545 = CARTESIAN_POINT ( 'NONE',  ( -96.80595820798417606, -278.9790802324217225, -318.8119841694697811 ) ) ;
#25546 = CARTESIAN_POINT ( 'NONE',  ( 34.95804673666359008, -280.0243634471505629, -244.8894512076283831 ) ) ;
#25547 = CARTESIAN_POINT ( 'NONE',  ( -99.77846524029713748, -245.9447597285579263, -331.8384115947385453 ) ) ;
#25548 = CARTESIAN_POINT ( 'NONE',  ( 25.87993695760413360, -277.0710214728277947, -313.9944411749354458 ) ) ;
#25549 = ADVANCED_FACE ( 'NONE', ( #46546 ), #38295, .T. ) ;
#25550 = APPLICATION_PROTOCOL_DEFINITION ( 'draft international standard', 'automotive_design', 1998, #83158 ) ;
#25551 = CARTESIAN_POINT ( 'NONE',  ( 9.073143622236854000, -276.1965237946996581, -209.7940474694468946 ) ) ;
#25552 = CARTESIAN_POINT ( 'NONE',  ( -6.998514795304313196, -276.9805209788415823, -207.2794874003663779 ) ) ;
#25553 = ORIENTED_EDGE ( 'NONE', *, *, #74314, .F. ) ;
#25554 = CARTESIAN_POINT ( 'NONE',  ( -36.09237171215955442, -55.96374926131388605, 21.50000000000000000 ) ) ;
#25555 = CARTESIAN_POINT ( 'NONE',  ( -110.6459840678237185, -291.6207767266403721, -271.2025624055261801 ) ) ;
#25556 = CARTESIAN_POINT ( 'NONE',  ( 36.52472489985140669, -289.5388456816189660, -288.2410043383971470 ) ) ;
#25557 = CARTESIAN_POINT ( 'NONE',  ( -104.7939251305819823, -290.2797902223945243, -242.0498235010827841 ) ) ;
#25558 = CARTESIAN_POINT ( 'NONE',  ( -36.55975511180312054, -285.5693750356871305, -193.4136011899824723 ) ) ;
#25559 = DIRECTION ( 'NONE',  ( 0.000000000000000000, 0.000000000000000000, -1.000000000000000000 ) ) ;
#25560 = CARTESIAN_POINT ( 'NONE',  ( -21.23322784865867874, -281.2420776797974895, -342.4342333873068469 ) ) ;
#25561 = CARTESIAN_POINT ( 'NONE',  ( 28.13085913905408475, -289.8828506476585858, -305.4592933652411944 ) ) ;
#25562 = CARTESIAN_POINT ( 'NONE',  ( -34.84223356253615123, -281.5000972172284719, -344.0246092364137667 ) ) ;
#25563 = CARTESIAN_POINT ( 'NONE',  ( -93.47765183090484697, -280.5370700635974117, -222.9076060274694555 ) ) ;
#25564 = CARTESIAN_POINT ( 'NONE',  ( -56.61036940264855133, -277.7995390838099752, -340.8885253938986466 ) ) ;
#25565 = CARTESIAN_POINT ( 'NONE',  ( -112.7451875362350222, -289.1764033355905212, -283.9379867042000001 ) ) ;
#25566 = CARTESIAN_POINT ( 'NONE',  ( -108.8818913653904303, -285.7127718562354062, -242.1778256472043154 ) ) ;
#25567 = CARTESIAN_POINT ( 'NONE',  ( -57.74565533973548526, -286.2879989769584199, -196.1222160341933431 ) ) ;
#25568 = CARTESIAN_POINT ( 'NONE',  ( -32.14358265104954882, -283.1514364725553605, -343.1758114118758840 ) ) ;
#25569 = ORIENTED_EDGE ( 'NONE', *, *, #68768, .T. ) ;
#25570 = FACE_OUTER_BOUND ( 'NONE', #68906, .T. ) ;
#25571 = CARTESIAN_POINT ( 'NONE',  ( -107.6433729033232538, -292.0482053882005857, -298.6096627827807879 ) ) ;
#25572 = CARTESIAN_POINT ( 'NONE',  ( 3.946974592896316025, -293.1937691885946720, -334.8326730824973652 ) ) ;
#25573 = CARTESIAN_POINT ( 'NONE',  ( 35.25532805655532087, -274.4840342527974144, -260.7133230601266973 ) ) ;
#25574 = CARTESIAN_POINT ( 'NONE',  ( -39.11381574257350024, -294.4224349072674727, -347.2387635841055271 ) ) ;
#25575 = CARTESIAN_POINT ( 'NONE',  ( -37.53249380121460632, -290.5296337344014432, -196.6554668432187896 ) ) ;
#25576 = CARTESIAN_POINT ( 'NONE',  ( -80.76719107979832302, -293.8903964171229291, -330.2960889660752741 ) ) ;
#25577 = CARTESIAN_POINT ( 'NONE',  ( -110.7654136604953550, -291.7820896920493396, -268.4667398160805760 ) ) ;
#25578 = DIRECTION ( 'NONE',  ( 1.000000000000000000, 0.000000000000000000, 0.000000000000000000 ) ) ;
#25579 = CARTESIAN_POINT ( 'NONE',  ( 3.175290891185845510, -290.5944646532404363, -206.9874687977882104 ) ) ;
#25580 = CARTESIAN_POINT ( 'NONE',  ( 37.69205350818191391, -295.5314410324865548, -268.7352367069600518 ) ) ;
#25581 = CARTESIAN_POINT ( 'NONE',  ( 20.55082093029577450, -289.1232809915065332, -315.2352391286513011 ) ) ;
#25582 = CARTESIAN_POINT ( 'NONE',  ( -23.22183395170791442, -278.8524837615598813, -344.4346601042021803 ) ) ;
#25583 = CARTESIAN_POINT ( 'NONE',  ( -25.84478731655473283, -275.7037448705905263, -346.0963786839527643 ) ) ;
#25584 = CARTESIAN_POINT ( 'NONE',  ( -100.6118826841001805, -296.3264313259777509, -226.7370499274407507 ) ) ;
#25585 = CARTESIAN_POINT ( 'NONE',  ( -8.362288971461047993, -274.9073398616443455, -338.4789411597768094 ) ) ;
#25586 = CARTESIAN_POINT ( 'NONE',  ( -60.15208332618225029, -277.8341531045858801, -199.4477485087159323 ) ) ;
#25587 = CARTESIAN_POINT ( 'NONE',  ( 5.395560307258694621, -275.8498380215813199, -210.6270688818391648 ) ) ;
#25588 = CARTESIAN_POINT ( 'NONE',  ( -8.209534443423670780, -275.0768568015299138, -340.7865961927353737 ) ) ;
#25589 = DIRECTION ( 'NONE',  ( -0.000000000000000000, -1.000000000000000000, -0.000000000000000000 ) ) ;
#25590 = CARTESIAN_POINT ( 'NONE',  ( -55.34326304613883707, -298.6175498637403507, -199.3964518560269994 ) ) ;
#25591 = AXIS2_PLACEMENT_3D ( 'NONE', #89070, #24219, #1989 ) ;
#25592 = LINE ( 'NONE', #54475, #91229 ) ;
#25594 = CARTESIAN_POINT ( 'NONE',  ( -56.85957220997867267, -273.6268068239612035, -199.9660059718328853 ) ) ;
#25593 = CARTESIAN_POINT ( 'NONE',  ( -81.90077662346757847, -287.6761211037696171, -331.1303166103268723 ) ) ;
#25595 = CARTESIAN_POINT ( 'NONE',  ( -5.626494891228408513, -288.6464334450402021, -340.5262500410424877 ) ) ;
#25596 = CARTESIAN_POINT ( 'NONE',  ( -9.574918072416505055, -288.3657980243124257, -342.1577063819490263 ) ) ;
#25597 = CARTESIAN_POINT ( 'NONE',  ( -84.67401047114253743, -275.4017879233168742, -211.9686456848743887 ) ) ;
#25598 = CARTESIAN_POINT ( 'NONE',  ( -76.64202284590486158, -293.5788096781457170, -334.1044522067512617 ) ) ;
#25599 = CARTESIAN_POINT ( 'NONE',  ( -1.202325990908861719, -279.7164282218247990, -202.5517937134897579 ) ) ;
#25600 = CARTESIAN_POINT ( 'NONE',  ( 133.0380396672494783, -299.5541904835127980, -195.3611179825600175 ) ) ;
#25601 = CARTESIAN_POINT ( 'NONE',  ( -110.5615960594187470, -276.3426869806426680, -286.6625226823388175 ) ) ;
#25602 = DIRECTION ( 'NONE',  ( 0.000000000000000000, -1.000000000000000000, 9.656854691831248164E-17 ) ) ;
#25603 = CARTESIAN_POINT ( 'NONE',  ( -72.80541811414191500, -290.3665778408421261, -206.0431734116716598 ) ) ;
#25604 = EDGE_CURVE ( 'NONE', #34180, #77042, #60786, .T. ) ;
#25605 = CARTESIAN_POINT ( 'NONE',  ( 156.2461366866179731, 19.34073763602960128, 8.651974842892217410 ) ) ;
#25606 = CARTESIAN_POINT ( 'NONE',  ( -112.3372061547354832, -288.5414404835573805, -271.1825322819155417 ) ) ;
#25607 = CARTESIAN_POINT ( 'NONE',  ( 15.93477411641185881, -276.3440126336588492, -219.3723906221099469 ) ) ;
#25608 = CARTESIAN_POINT ( 'NONE',  ( 36.97953357970315125, -283.2017377431821501, -288.1641127980598753 ) ) ;
#25610 = CARTESIAN_POINT ( 'NONE',  ( -108.4252987394931154, -284.3322923855890849, -287.0326531900352052 ) ) ;
#25609 = CARTESIAN_POINT ( 'NONE',  ( -4.285333808817019197, -296.4841077558293705, -195.0169975265855555 ) ) ;
#25611 = CARTESIAN_POINT ( 'NONE',  ( -13.89474671823018248, -275.7877336766558187, -200.6071554270697845 ) ) ;
#25612 = CARTESIAN_POINT ( 'NONE',  ( 17.39958941581236118, -275.6622237120047885, -221.7474917221501585 ) ) ;
#25613 = EDGE_CURVE ( 'NONE', #3069, #78294, #30747, .T. ) ;
#25614 = CARTESIAN_POINT ( 'NONE',  ( 21.84084554167343484, -284.1843652691930515, -316.4516850225342068 ) ) ;
#25615 = CARTESIAN_POINT ( 'NONE',  ( -69.61470576497724494, -272.5372755679247803, -204.5380279468873539 ) ) ;
#25616 = ORIENTED_EDGE ( 'NONE', *, *, #20540, .F. ) ;
#25617 = CARTESIAN_POINT ( 'NONE',  ( -43.54160339317392214, -248.0334966641272842, -472.6442049081569508 ) ) ;
#25618 = CARTESIAN_POINT ( 'NONE',  ( 33.41573010253615195, -293.7738229807613379, -300.8665737748893889 ) ) ;
#25619 = CARTESIAN_POINT ( 'NONE',  ( -110.8164321505503978, -286.7028126544021234, -257.1243312004908148 ) ) ;
#25620 = CARTESIAN_POINT ( 'NONE',  ( 207.7755975652984830, 28.53818587417392294, 12.00000000000000000 ) ) ;
#25621 = CARTESIAN_POINT ( 'NONE',  ( -2.602324593224659921, -271.9809262143061233, -198.2974183793908196 ) ) ;
#25622 = CARTESIAN_POINT ( 'NONE',  ( -72.77533261791276686, -276.7064962126826231, -338.5565551892367466 ) ) ;
#25623 = CARTESIAN_POINT ( 'NONE',  ( -109.1189367289343721, -288.6239593457595447, -296.1002536608158948 ) ) ;
#25624 = CARTESIAN_POINT ( 'NONE',  ( -53.82610694498197290, -284.7875690186324391, -342.2396782832729514 ) ) ;
#25625 = CARTESIAN_POINT ( 'NONE',  ( -79.18669764713884263, -279.3850730550349226, -331.4724289833314401 ) ) ;
#25626 = CARTESIAN_POINT ( 'NONE',  ( -36.58960276809222734, -287.4866838307142984, -193.9411072039653732 ) ) ;
#25627 = CARTESIAN_POINT ( 'NONE',  ( 14.70517680308578790, -282.7847647462911596, -216.2876277470288926 ) ) ;
#25628 = CARTESIAN_POINT ( 'NONE',  ( -29.84099491404666082, -274.3113054987382498, -193.7273171777334824 ) ) ;
#25629 = CARTESIAN_POINT ( 'NONE',  ( -70.30294375176407584, -277.3078857283183538, -339.9640346678647234 ) ) ;
#25630 = CARTESIAN_POINT ( 'NONE',  ( -41.08769931505037931, -297.0197877011902392, -344.7196237511550407 ) ) ;
#25631 = DIRECTION ( 'NONE',  ( 0.000000000000000000, 1.000000000000000000, 0.000000000000000000 ) ) ;
#25632 = DIRECTION ( 'NONE',  ( 1.000000000000000000, -1.124465274301078034E-16, 0.000000000000000000 ) ) ;
#25633 = CARTESIAN_POINT ( 'NONE',  ( -72.68301609920166584, -295.7292325444900030, -203.2860891920712163 ) ) ;
#25634 = CARTESIAN_POINT ( 'NONE',  ( -32.42267340908522044, -276.4962532529142436, -343.3068851284983793 ) ) ;
#25635 = CARTESIAN_POINT ( 'NONE',  ( -37.62039264774393388, -299.1284046588111210, -193.6707350009189668 ) ) ;
#25636 = CARTESIAN_POINT ( 'NONE',  ( -19.59428103012816180, -288.0436757755916233, -198.5070775513977424 ) ) ;
#25637 = EDGE_CURVE ( 'NONE', #35960, #43712, #41246, .T. ) ;
#25638 = CARTESIAN_POINT ( 'NONE',  ( -111.2918881712147368, -297.8340676649014540, -289.2307598041940082 ) ) ;
#25639 = CARTESIAN_POINT ( 'NONE',  ( -30.61047808688418925, -296.1738977209472523, -346.6677321666859370 ) ) ;
#25640 = CARTESIAN_POINT ( 'NONE',  ( -109.1618181126651592, -292.8241350131525564, -249.2941676546431040 ) ) ;
#25641 = CARTESIAN_POINT ( 'NONE',  ( -4.737268542336128263, -278.4824537626984124, -203.0040138855710552 ) ) ;
#25642 = CARTESIAN_POINT ( 'NONE',  ( -75.25995026235231933, -281.4631024603752962, -206.2431335187117440 ) ) ;
#25643 = CARTESIAN_POINT ( 'NONE',  ( -111.9865001276048986, -270.5725786021788508, -270.3359667857977229 ) ) ;
#25644 = CARTESIAN_POINT ( 'NONE',  ( -11.10714175854606189, -284.5743800810157609, -341.4946611779132013 ) ) ;
#25645 = CARTESIAN_POINT ( 'NONE',  ( 20.59335882061688139, -285.8424798724951756, -225.4416899004503421 ) ) ;
#25646 = CARTESIAN_POINT ( 'NONE',  ( -54.56600731238864910, -170.2994449650265096, -364.0860178467487458 ) ) ;
#25647 = VERTEX_POINT ( 'NONE', #4407 ) ;
#25648 = CARTESIAN_POINT ( 'NONE',  ( -30.52508452115705495, -285.8072984000240240, -197.6080265558017288 ) ) ;
#25649 = ORIENTED_EDGE ( 'NONE', *, *, #73796, .F. ) ;
#25650 = CARTESIAN_POINT ( 'NONE',  ( -24.57146089363258312, -283.9726479932963343, -346.0352106241145407 ) ) ;
#25651 = CARTESIAN_POINT ( 'NONE',  ( -34.48319489723353826, -298.5812350648678262, -197.2993321103043911 ) ) ;
#25652 = CARTESIAN_POINT ( 'NONE',  ( -33.73061514378654380, -284.8915767187771735, -193.8433502127151087 ) ) ;
#25653 = CARTESIAN_POINT ( 'NONE',  ( 34.10102936607029989, -282.1346251684736899, -242.1312818794532404 ) ) ;
#25654 = CARTESIAN_POINT ( 'NONE',  ( 196.0143093133015384, 19.33012701892219098, -12.49999999999999289 ) ) ;
#25655 = CARTESIAN_POINT ( 'NONE',  ( -99.69372176527166118, -280.6595780536233065, -226.3732429364199277 ) ) ;
#25656 = CARTESIAN_POINT ( 'NONE',  ( 21.04729040431934450, -281.2079403954513737, -220.1766455182886375 ) ) ;
#25657 = VECTOR ( 'NONE', #14719, 1000.000000000000000 ) ;
#25658 = CARTESIAN_POINT ( 'NONE',  ( -82.13390479932374433, -281.1952119285918457, -326.4764044574609443 ) ) ;
#25659 = CARTESIAN_POINT ( 'NONE',  ( 202.9216279488346686, 293.3251575386738068, -83.23662280983118933 ) ) ;
#25660 = ORIENTED_EDGE ( 'NONE', *, *, #8160, .F. ) ;
#25661 = CARTESIAN_POINT ( 'NONE',  ( 10.86399985531348733, -278.3837087097922449, -327.5995570998625226 ) ) ;
#25662 = CARTESIAN_POINT ( 'NONE',  ( -90.69729355805023374, -230.0588105309422247, -347.5619421900863699 ) ) ;
#25663 = VECTOR ( 'NONE', #69750, 1000.000000000000000 ) ;
#25664 = CARTESIAN_POINT ( 'NONE',  ( 36.66691670201128517, -279.4418272682470956, -260.2510634191229997 ) ) ;
#25665 = CARTESIAN_POINT ( 'NONE',  ( -16.92077093663188592, -294.0724854820045380, -197.1698639799152204 ) ) ;
#25666 = CARTESIAN_POINT ( 'NONE',  ( -92.27274552457252810, -295.2131824268811897, -318.5946428386462230 ) ) ;
#25667 = CARTESIAN_POINT ( 'NONE',  ( -34.95603508188709441, -291.5889850733971116, -193.4465122751517185 ) ) ;
#25668 = DIRECTION ( 'NONE',  ( 0.000000000000000000, 1.000000000000000000, 0.000000000000000000 ) ) ;
#25669 = EDGE_CURVE ( 'NONE', #25873, #23364, #79148, .T. ) ;
#25671 = CARTESIAN_POINT ( 'NONE',  ( -3.012198179119665920, -286.9908707911066585, -335.7470691259181876 ) ) ;
#25670 = CARTESIAN_POINT ( 'NONE',  ( -111.6967567103062322, -295.3487716004134427, -252.7562363852289309 ) ) ;
#25672 = CARTESIAN_POINT ( 'NONE',  ( 9.017714892348468680, -296.2690157128162127, -328.4071112095504645 ) ) ;
#25673 = ADVANCED_FACE ( 'NONE', ( #62181 ), #68348, .T. ) ;
#25674 = CARTESIAN_POINT ( 'NONE',  ( -109.4158608333471960, -286.0556496217638482, -255.9889630330912098 ) ) ;
#25675 = ORIENTED_EDGE ( 'NONE', *, *, #59092, .T. ) ;
#25676 = CARTESIAN_POINT ( 'NONE',  ( 29.37612370723951472, -294.9891731240032300, -308.4363064969310244 ) ) ;
#25677 = CARTESIAN_POINT ( 'NONE',  ( 29.37321052148537959, -282.4467158442050732, -300.2697392283906197 ) ) ;
#25678 = CARTESIAN_POINT ( 'NONE',  ( -58.75511502022377641, -294.1179092739052408, -343.9655358312071485 ) ) ;
#25679 = CARTESIAN_POINT ( 'NONE',  ( -111.3836305162620448, -291.0970844283563679, -290.9025727797135801 ) ) ;
#25680 = CARTESIAN_POINT ( 'NONE',  ( -50.56194987510324523, -292.3799901568387440, -194.5669763903573255 ) ) ;
#25681 = CARTESIAN_POINT ( 'NONE',  ( -88.65956010366774365, -289.9639465690058842, -322.2791038065706744 ) ) ;
#25682 = EDGE_LOOP ( 'NONE', ( #91921, #73430, #37427, #70140 ) ) ;
#25683 = CARTESIAN_POINT ( 'NONE',  ( -89.87931010611180227, -272.1253713169422781, -214.5409756786795299 ) ) ;
#25684 = CARTESIAN_POINT ( 'NONE',  ( -27.51497411582626995, -279.2386571564418887, -197.7367365232332190 ) ) ;
#25685 = EDGE_LOOP ( 'NONE', ( #23096, #77736 ) ) ;
#25686 = CARTESIAN_POINT ( 'NONE',  ( -2.579733554756037606, -274.0070829431385846, -201.7087357506077581 ) ) ;
#25687 = CARTESIAN_POINT ( 'NONE',  ( 18.37777377432308512, -278.1015011621257713, -319.4333934114329168 ) ) ;
#25688 = CARTESIAN_POINT ( 'NONE',  ( -18.94295532091393497, -272.4309482982852728, -198.3887362015445603 ) ) ;
#25689 = CARTESIAN_POINT ( 'NONE',  ( -105.1348051114124047, -298.1323903834429530, -242.2323885310863432 ) ) ;
#25690 = CARTESIAN_POINT ( 'NONE',  ( -35.82125369465582310, -299.1512985992672498, -197.0517164500904812 ) ) ;
#25691 = FACE_OUTER_BOUND ( 'NONE', #22296, .T. ) ;
#25692 = CARTESIAN_POINT ( 'NONE',  ( -112.3552029044302998, -298.3215523385778170, -256.9665363251803569 ) ) ;
#25693 = CARTESIAN_POINT ( 'NONE',  ( 73.04948978576122443, -297.4307250721599871, -195.2319741477500656 ) ) ;
#25694 = CARTESIAN_POINT ( 'NONE',  ( 21.88242546706848657, -293.6046374159868151, -227.4866480982354915 ) ) ;
#25695 = CARTESIAN_POINT ( 'NONE',  ( -12.04070959418731235, -290.9625677101679457, -201.2037262385670999 ) ) ;
#25696 = CARTESIAN_POINT ( 'NONE',  ( 209.0573810755008992, 30.16382728711827710, 15.12480380411953718 ) ) ;
#25697 = CARTESIAN_POINT ( 'NONE',  ( -13.08783334611800164, -274.8513833894338632, -197.3455247901048324 ) ) ;
#25698 = CARTESIAN_POINT ( 'NONE',  ( -109.5830769536326414, -272.8618616679830780, -259.5187654142159204 ) ) ;
#25699 = CARTESIAN_POINT ( 'NONE',  ( -8.641469825694837681, -284.6584747970617286, -340.0921619764920933 ) ) ;
#25700 = CARTESIAN_POINT ( 'NONE',  ( -27.45254589757167807, -281.6139772762828102, -346.2791674358736032 ) ) ;
#25701 = CARTESIAN_POINT ( 'NONE',  ( -97.85383888099049443, -277.2655848536886083, -317.8120805722413706 ) ) ;
#25702 = DIRECTION ( 'NONE',  ( 0.09665007798479530177, -0.000000000000000000, 0.9953184226294281567 ) ) ;
#25703 = CARTESIAN_POINT ( 'NONE',  ( -93.55268387274327324, -283.0863259365150384, -317.1898168104737010 ) ) ;
#25704 = CARTESIAN_POINT ( 'NONE',  ( 37.45113411599673015, -279.6543336534976447, -278.3496193524680962 ) ) ;
#25705 = CARTESIAN_POINT ( 'NONE',  ( 1.164400433653314249, -275.1022051699037547, -333.1318705715253259 ) ) ;
#25706 = CARTESIAN_POINT ( 'NONE',  ( -95.65078582317094913, -279.9027245443101037, -317.5515851221219350 ) ) ;
#25707 = DIRECTION ( 'NONE',  ( 0.000000000000000000, 0.000000000000000000, -1.000000000000000000 ) ) ;
#25708 = CARTESIAN_POINT ( 'NONE',  ( 153.8631963276546628, 19.40208621445597004, 11.71714748521188731 ) ) ;
#25709 = CARTESIAN_POINT ( 'NONE',  ( -9.549216625494851840, -296.6354199188683083, -194.3826371356322795 ) ) ;
#25710 = CARTESIAN_POINT ( 'NONE',  ( -109.9664595759330155, -280.8014833033493005, -250.9290821974932157 ) ) ;
#25711 = CARTESIAN_POINT ( 'NONE',  ( 156.4870464395701219, 215.0000000000000568, 17.29054515234685141 ) ) ;
#25712 = CARTESIAN_POINT ( 'NONE',  ( -67.28773519107451762, -285.3619353537811776, -339.7336571039463706 ) ) ;
#25713 = CARTESIAN_POINT ( 'NONE',  ( 156.4677141125679611, 15.48129629386866313, -7.027845929950994552 ) ) ;
#25714 = CARTESIAN_POINT ( 'NONE',  ( 14.60772790238195107, -286.3212544238138548, -324.5266233820272532 ) ) ;
#25715 = CARTESIAN_POINT ( 'NONE',  ( 206.6195589736935005, 30.30844190587212594, 14.49999999999999822 ) ) ;
#25716 = CARTESIAN_POINT ( 'NONE',  ( -71.12716255693898404, -294.3033585865081250, -335.5340088935061544 ) ) ;
#25717 = CARTESIAN_POINT ( 'NONE',  ( -37.29055519897222837, -287.1910898083224879, -344.5963041702376017 ) ) ;
#25718 = CARTESIAN_POINT ( 'NONE',  ( -49.37856652629597676, -155.6656457446864010, -366.7448178265262868 ) ) ;
#25719 = CARTESIAN_POINT ( 'NONE',  ( -94.62602932240814368, -293.8822009894938105, -318.7907966750074706 ) ) ;
#25720 = CARTESIAN_POINT ( 'NONE',  ( -78.13531591035727786, -283.9940897731921154, -205.8739978481109176 ) ) ;
#25721 = CARTESIAN_POINT ( 'NONE',  ( 34.10306240125144939, -283.3943974560218635, -288.9070856567997794 ) ) ;
#25722 = CARTESIAN_POINT ( 'NONE',  ( -44.34840006887846187, -281.3793482781901503, -346.0767118028122127 ) ) ;
#25723 = CARTESIAN_POINT ( 'NONE',  ( -102.8454316650584275, -290.1155329157977576, -302.5831780459953961 ) ) ;
#25724 = CARTESIAN_POINT ( 'NONE',  ( -34.30705430493454600, -281.5162894098867810, -196.8218395327261590 ) ) ;
#25725 = CARTESIAN_POINT ( 'NONE',  ( -7.943923662102324812, -281.2502555535783699, -203.3520995798398587 ) ) ;
#25726 = CARTESIAN_POINT ( 'NONE',  ( 21.14485214991424655, -290.1835821195315361, -317.8970111168432595 ) ) ;
#25727 = ADVANCED_FACE ( 'NONE', ( #55073 ), #75448, .T. ) ;
#25728 = VERTEX_POINT ( 'NONE', #91505 ) ;
#25729 = CARTESIAN_POINT ( 'NONE',  ( -58.12161569055139410, -273.7909900291650729, -196.1626211770820305 ) ) ;
#25731 = CARTESIAN_POINT ( 'NONE',  ( -111.0390911448227200, -292.3780697433153364, -282.2963611797865724 ) ) ;
#25730 = CIRCLE ( 'NONE', #78678, 7.500000000000012434 ) ;
#25732 = CARTESIAN_POINT ( 'NONE',  ( -43.18343439339132317, -248.4123448508205172, -502.6442049081569508 ) ) ;
#25733 = CARTESIAN_POINT ( 'NONE',  ( -88.52914483777347243, -293.9090924074131408, -206.2264541496106460 ) ) ;
#25734 = ORIENTED_EDGE ( 'NONE', *, *, #54408, .F. ) ;
#25735 = CARTESIAN_POINT ( 'NONE',  ( -17.85824711556551492, -274.8013122890735076, -342.9588003310910835 ) ) ;
#25736 = CARTESIAN_POINT ( 'NONE',  ( 140.6539576904058606, 250.0000000000000568, -12.00000000000000000 ) ) ;
#25737 = CARTESIAN_POINT ( 'NONE',  ( -30.68138555019360680, -293.3691461168232308, -346.2694879088334119 ) ) ;
#25738 = CARTESIAN_POINT ( 'NONE',  ( -63.33522389967379240, -273.0529365769760943, -202.0231641902481385 ) ) ;
#25739 = CARTESIAN_POINT ( 'NONE',  ( -76.21822789854435598, -291.1022548893236603, -332.9656173455052794 ) ) ;
#25741 = EDGE_CURVE ( 'NONE', #50317, #26361, #45929, .T. ) ;
#25740 = CARTESIAN_POINT ( 'NONE',  ( 30.24888643064024052, -283.7143058662104522, -300.6447381919217605 ) ) ;
#25742 = CARTESIAN_POINT ( 'NONE',  ( -106.7330034028650800, -292.3912392892430603, -238.2435322501283110 ) ) ;
#25743 = CARTESIAN_POINT ( 'NONE',  ( -110.7636443102908714, -292.1388055199153087, -248.8549238591254777 ) ) ;
#25744 = CARTESIAN_POINT ( 'NONE',  ( -57.65290562738642421, -291.6159439643503219, -200.1908048483340679 ) ) ;
#25745 = CARTESIAN_POINT ( 'NONE',  ( -105.3084130313718987, -286.9705025652195900, -238.5278767630905463 ) ) ;
#25746 = CARTESIAN_POINT ( 'NONE',  ( -53.76254813612103334, -280.0138378833462411, -195.0778590257286282 ) ) ;
#25747 = CARTESIAN_POINT ( 'NONE',  ( -105.2090043722127461, -295.0666929450824227, -237.1445075327571033 ) ) ;
#25748 = CARTESIAN_POINT ( 'NONE',  ( 6.923273902218037179, -282.3015927835048728, -333.4311748372482498 ) ) ;
#25749 = CARTESIAN_POINT ( 'NONE',  ( 36.60642713423293770, -277.3207133737288927, -263.2797449635788212 ) ) ;
#25750 = CARTESIAN_POINT ( 'NONE',  ( -37.37352853689063181, -282.5519495502701375, -200.3611179825600459 ) ) ;
#25751 = CARTESIAN_POINT ( 'NONE',  ( -72.29229894553861868, -275.6490838595548212, -337.5973187841282765 ) ) ;
#25752 = DIRECTION ( 'NONE',  ( -1.000000000000000000, 0.000000000000000000, 0.000000000000000000 ) ) ;
#25753 = CARTESIAN_POINT ( 'NONE',  ( -95.16898982769096449, -283.4314139382817075, -315.0356911304073151 ) ) ;
#25754 = CARTESIAN_POINT ( 'NONE',  ( -110.1769558053102003, -280.0591821721940278, -246.4643133719727643 ) ) ;
#25755 = CARTESIAN_POINT ( 'NONE',  ( 32.50294254440365194, -286.2010408273715711, -238.3811718237456034 ) ) ;
#25756 = CARTESIAN_POINT ( 'NONE',  ( 13.58438430990091561, -294.5375101294663409, -216.6535027333626999 ) ) ;
#25757 = CARTESIAN_POINT ( 'NONE',  ( 29.23851005349852983, -276.6655694952522140, -233.1916905835554132 ) ) ;
#25758 = CARTESIAN_POINT ( 'NONE',  ( 37.45967281773607738, -276.6643435583600308, -254.2352225771534222 ) ) ;
#25759 = CARTESIAN_POINT ( 'NONE',  ( -109.1317158414841799, -278.5600772795537523, -257.1250442297024961 ) ) ;
#25760 = CARTESIAN_POINT ( 'NONE',  ( -111.5577648836208766, -298.6807984470532915, -260.3767669189888920 ) ) ;
#25761 = EDGE_CURVE ( 'NONE', #47569, #23012, #62528, .T. ) ;
#25762 = CARTESIAN_POINT ( 'NONE',  ( -96.38832024477478910, -283.1841407755607065, -224.3672283150072246 ) ) ;
#25763 = CARTESIAN_POINT ( 'NONE',  ( -8.515197623694632512, -292.0860370985155328, -198.9834110643347174 ) ) ;
#25764 = CARTESIAN_POINT ( 'NONE',  ( 35.19255307683887679, -289.4489897864291947, -293.7111185641127236 ) ) ;
#25765 = CARTESIAN_POINT ( 'NONE',  ( -2.279549647253553690, -291.4480219074775391, -205.9661836086507094 ) ) ;
#25766 = ORIENTED_EDGE ( 'NONE', *, *, #92370, .T. ) ;
#25767 = CARTESIAN_POINT ( 'NONE',  ( -83.89289766830796680, -290.0019943030525269, -209.7007780552170857 ) ) ;
#25768 = CARTESIAN_POINT ( 'NONE',  ( -37.54574934532697483, -291.7162823329366574, -197.3278115807005122 ) ) ;
#25769 = VERTEX_POINT ( 'NONE', #12945 ) ;
#25770 = CARTESIAN_POINT ( 'NONE',  ( -102.0330907817240131, -291.0886148197743637, -311.6476078826511298 ) ) ;
#25771 = CARTESIAN_POINT ( 'NONE',  ( -91.31530743669969752, -279.5904776051542058, -221.1784258958365683 ) ) ;
#25772 = CARTESIAN_POINT ( 'NONE',  ( -110.0570086449736067, -295.1643557943131100, -294.7327493761372921 ) ) ;
#25773 = CARTESIAN_POINT ( 'NONE',  ( -89.82274634191698226, -285.9862872428379319, -214.0832377296034679 ) ) ;
#25774 = CARTESIAN_POINT ( 'NONE',  ( -15.42354209600849480, -286.6614657292587367, -196.5132041097130013 ) ) ;
#25775 = CARTESIAN_POINT ( 'NONE',  ( -105.2320262026618423, -284.5242119666446570, -297.3872320343882620 ) ) ;
#25776 = CARTESIAN_POINT ( 'NONE',  ( 203.3289701366145152, 295.9433977242509286, -68.67267355934257012 ) ) ;
#25777 = B_SPLINE_CURVE_WITH_KNOTS ( 'NONE', 3,
 ( #79657, #8139, #65470, #29470, #37022, #29926, #73481, #9045, #31320, #30858, #17580, #67766, #1496, #73929, #88119, #38860 ),
 .UNSPECIFIED., .F., .F.,
 ( 4, 2, 2, 2, 2, 2, 2, 4 ),
 ( 0.000000000000000000, 0.001195571706423382121, 0.001793357559635075458, 0.002391143412846768578, 0.002988929266058461699, 0.003586715119270155253, 0.004184500972481848373, 0.004782286825693541493 ),
 .UNSPECIFIED. ) ;
#25778 = CARTESIAN_POINT ( 'NONE',  ( 120.1291425852486583, 149.7169047988457748, -262.4347193084595347 ) ) ;
#25779 = CARTESIAN_POINT ( 'NONE',  ( 24.90698337435117793, -23.76329158025230015, -341.4199860761482341 ) ) ;
#25780 = CARTESIAN_POINT ( 'NONE',  ( -4.022037595628576767, -273.7004142286585306, -205.2133306798716035 ) ) ;
#25781 = CARTESIAN_POINT ( 'NONE',  ( -18.95262775744699013, -275.7301201017140215, -341.3263777229997231 ) ) ;
#25782 = CARTESIAN_POINT ( 'NONE',  ( -48.95450548983835404, -297.4157943772210047, -194.2504790863257256 ) ) ;
#25783 = CARTESIAN_POINT ( 'NONE',  ( 174.6243218329550757, 240.3365076134214178, -177.4484248103281061 ) ) ;
#25784 = EDGE_CURVE ( 'NONE', #9133, #74935, #15602, .T. ) ;
#25785 = CARTESIAN_POINT ( 'NONE',  ( 30.81858792213831677, -273.7865838961465101, -235.6123999579116344 ) ) ;
#25786 = CARTESIAN_POINT ( 'NONE',  ( -35.38570508461067732, -275.8371450463314432, -196.3609527273910373 ) ) ;
#25787 = CARTESIAN_POINT ( 'NONE',  ( -113.5570086104289658, -273.7388997161712609, -261.8335589948311508 ) ) ;
#25788 = CARTESIAN_POINT ( 'NONE',  ( -74.74202174047974268, -290.0568641876849938, -333.1388978529938640 ) ) ;
#25789 = CARTESIAN_POINT ( 'NONE',  ( -79.38005676511495778, -296.4071618938556298, -334.6801306571198893 ) ) ;
#25790 = CARTESIAN_POINT ( 'NONE',  ( -113.5907721819394141, -296.9109925778882371, -281.0275484406095643 ) ) ;
#25791 = CARTESIAN_POINT ( 'NONE',  ( -50.46912369117863051, -295.3911572754605004, -342.1710807668425787 ) ) ;
#25792 = ORIENTED_EDGE ( 'NONE', *, *, #50543, .F. ) ;
#25793 = CARTESIAN_POINT ( 'NONE',  ( -37.10642829824096367, -278.9693415054871934, -345.9335705797932974 ) ) ;
#25794 = VERTEX_POINT ( 'NONE', #41299 ) ;
#25795 = AXIS2_PLACEMENT_3D ( 'NONE', #61759, #90592, #25752 ) ;
#25796 = CARTESIAN_POINT ( 'NONE',  ( -42.41972680664798645, -279.4973746876558494, -193.5904168764288613 ) ) ;
#25797 = CARTESIAN_POINT ( 'NONE',  ( 16.71289508835151238, -277.2000932482852136, -319.7914558029112868 ) ) ;
#25798 = CARTESIAN_POINT ( 'NONE',  ( 25.24516168202696065, -277.8897785374628597, -313.5435093532957467 ) ) ;
#25799 = AXIS2_PLACEMENT_3D ( 'NONE', #69303, #41328, #27152 ) ;
#25800 = CARTESIAN_POINT ( 'NONE',  ( -109.1081219787577368, -276.2751154481544518, -293.5072813455016103 ) ) ;
#25801 = CARTESIAN_POINT ( 'NONE',  ( -32.69337472332519212, -274.6046302645801234, -197.4350603189898266 ) ) ;
#25802 = CARTESIAN_POINT ( 'NONE',  ( -92.27273266985599776, -295.8215530872476506, -221.3921831174093029 ) ) ;
#25803 = CARTESIAN_POINT ( 'NONE',  ( 222.0386546523673985, 36.13108063356137478, 10.00000000000000000 ) ) ;
#25804 = CARTESIAN_POINT ( 'NONE',  ( -93.94187354024062131, -279.3714059192312789, -224.2588363226474257 ) ) ;
#25805 = CARTESIAN_POINT ( 'NONE',  ( -37.51737777987461442, -287.7391046918958750, -346.8807552776460170 ) ) ;
#25806 = CARTESIAN_POINT ( 'NONE',  ( -60.28419677691929479, -275.7550055324873028, -198.9021465559121680 ) ) ;
#25807 = CARTESIAN_POINT ( 'NONE',  ( 196.2586151081795833, 20.67842735233990581, -13.53470692911517581 ) ) ;
#25808 = CARTESIAN_POINT ( 'NONE',  ( -109.9510235274600376, -289.6312277285310870, -279.3326218908130159 ) ) ;
#25809 = CARTESIAN_POINT ( 'NONE',  ( -110.1308739028959138, -283.5878546670392097, -295.1612987813265363 ) ) ;
#25810 = CARTESIAN_POINT ( 'NONE',  ( 34.09748294977161009, -279.5393322973619661, -250.9627124732487005 ) ) ;
#25812 = CARTESIAN_POINT ( 'NONE',  ( -75.43643540319085616, -283.6196787863938198, -206.4071865780526878 ) ) ;
#25811 = CARTESIAN_POINT ( 'NONE',  ( 33.30530965296356527, -279.8565443958207766, -249.7607556845141801 ) ) ;
#25813 = CARTESIAN_POINT ( 'NONE',  ( 24.80478984558882871, -288.9832002199053704, -228.2840840740589101 ) ) ;
#25814 = CARTESIAN_POINT ( 'NONE',  ( -94.25811432216426056, -280.4096335186494571, -224.0183483046573940 ) ) ;
#25815 = FACE_OUTER_BOUND ( 'NONE', #49889, .T. ) ;
#25816 = CARTESIAN_POINT ( 'NONE',  ( -4.227951794944921460, -294.4888015480337344, -203.0529764801314911 ) ) ;
#25817 = CARTESIAN_POINT ( 'NONE',  ( -45.14669500603307739, -278.1945928290650727, -194.7240645622421198 ) ) ;
#25818 = CARTESIAN_POINT ( 'NONE',  ( 20.92318118658734605, -276.8231024925980250, -314.5096884450998687 ) ) ;
#25819 = CARTESIAN_POINT ( 'NONE',  ( -63.25549200618215195, -285.3891191476989775, -340.9196314062497777 ) ) ;
#25820 = CARTESIAN_POINT ( 'NONE',  ( 197.4477343783226786, 67.35408903922716206, 10.31406111472453091 ) ) ;
#25821 = CARTESIAN_POINT ( 'NONE',  ( -110.8558847328221191, -292.2490257316667908, -287.8800493199952371 ) ) ;
#25822 = CARTESIAN_POINT ( 'NONE',  ( -73.90191560405894222, -293.5375007154946161, -335.8610894536354294 ) ) ;
#25823 = CARTESIAN_POINT ( 'NONE',  ( 29.99499273372738628, -286.2677321309743661, -233.2381440699909945 ) ) ;
#25824 = CARTESIAN_POINT ( 'NONE',  ( -92.25494350317529779, -289.6502297942929545, -221.0372926380688909 ) ) ;
#25825 = CARTESIAN_POINT ( 'NONE',  ( 85.55100297371609486, -373.0521521680024648, -517.1711561948568487 ) ) ;
#25826 = CARTESIAN_POINT ( 'NONE',  ( 32.98344197680759038, -274.5182354711825496, -291.7499168344537566 ) ) ;
#25827 = CARTESIAN_POINT ( 'NONE',  ( -17.91977323886857931, -292.9386378800824673, -342.0106415929492414 ) ) ;
#25828 = CARTESIAN_POINT ( 'NONE',  ( 195.8229337057643988, 41.01736685183180953, 14.50757396441050773 ) ) ;
#25829 = CARTESIAN_POINT ( 'NONE',  ( 197.3200855685783495, 41.90484851767786978, 12.40975777105213851 ) ) ;
#25830 = CARTESIAN_POINT ( 'NONE',  ( -50.42824481119912150, -290.3678449910482300, -195.1849907922274667 ) ) ;
#25831 = CARTESIAN_POINT ( 'NONE',  ( -46.84789082344370570, -287.5297181109634721, -197.1245903374295381 ) ) ;
#25832 = CARTESIAN_POINT ( 'NONE',  ( 23.31954395817320957, -286.4095506278797529, -316.1234112176571216 ) ) ;
#25833 = CARTESIAN_POINT ( 'NONE',  ( -110.9070211703337208, -285.9339657820697767, -273.6826870961493228 ) ) ;
#25834 = DIRECTION ( 'NONE',  ( 0.000000000000000000, 0.000000000000000000, 1.000000000000000000 ) ) ;
#25835 = CARTESIAN_POINT ( 'NONE',  ( -87.81327407348437930, -286.1273977716414834, -217.3967719548230662 ) ) ;
#25836 = CARTESIAN_POINT ( 'NONE',  ( 5.539117145922015872, -294.6096153730299534, -208.3962706065396731 ) ) ;
#25837 = CARTESIAN_POINT ( 'NONE',  ( -110.7815009478636057, -276.4047906252646385, -288.1892350526958353 ) ) ;
#25838 = CARTESIAN_POINT ( 'NONE',  ( 37.57227483734749285, -276.1076319789668787, -288.1278113834255805 ) ) ;
#25839 = CARTESIAN_POINT ( 'NONE',  ( 8.006600369479306423, -290.7459360878327743, -209.8570237530543920 ) ) ;
#25840 = CARTESIAN_POINT ( 'NONE',  ( -114.3849019319820002, -278.5365532289854400, -271.6083964946004130 ) ) ;
#25841 = CARTESIAN_POINT ( 'NONE',  ( -111.4339917909207429, -298.4097718335198124, -279.8391550080929733 ) ) ;
#25842 = CARTESIAN_POINT ( 'NONE',  ( -43.51344012988974441, -251.1608963058792199, -487.1372761508537224 ) ) ;
#25843 = CARTESIAN_POINT ( 'NONE',  ( -48.18343439339133027, -296.0521521680024080, -430.6442049081568939 ) ) ;
#25844 = CARTESIAN_POINT ( 'NONE',  ( -89.97807872487524605, -275.9444495014743666, -322.7817942617505196 ) ) ;
#25845 = CARTESIAN_POINT ( 'NONE',  ( 27.56872345658622336, -279.0503911176733709, -232.7893525645756938 ) ) ;
#25846 = DIRECTION ( 'NONE',  ( -0.6421047760857900855, 0.000000000000000000, -0.7666168903225505371 ) ) ;
#25847 = CARTESIAN_POINT ( 'NONE',  ( 36.61804261008658301, -273.7949141879465742, -251.5817620615348744 ) ) ;
#25848 = CARTESIAN_POINT ( 'NONE',  ( -35.61514498691887098, -296.5502584981659879, -344.0468399903400609 ) ) ;
#25849 = CARTESIAN_POINT ( 'NONE',  ( 25.66848100500453356, -281.0526126696997835, -314.1015914732294618 ) ) ;
#25850 = CARTESIAN_POINT ( 'NONE',  ( -71.02839428366141306, -296.4493392220763894, -335.4029488731391666 ) ) ;
#25851 = CARTESIAN_POINT ( 'NONE',  ( -113.4509216657957182, -297.7692705867122527, -278.1511544995717031 ) ) ;
#25852 = CARTESIAN_POINT ( 'NONE',  ( -93.79202054805612931, -272.8750204820507861, -224.0225782304559345 ) ) ;
#25853 = CARTESIAN_POINT ( 'NONE',  ( -64.82765207447191358, -293.6933763777807940, -200.5652437169594293 ) ) ;
#25854 = CARTESIAN_POINT ( 'NONE',  ( 25.54387905179369156, -287.1305618508691850, -225.9041207761447652 ) ) ;
#25855 = CARTESIAN_POINT ( 'NONE',  ( 36.69353084813054267, -273.8970994999799586, -286.5179221841542017 ) ) ;
#25856 = CARTESIAN_POINT ( 'NONE',  ( -1.802610534173727741, -288.4277567463471428, -338.6690466245649986 ) ) ;
#25857 = CARTESIAN_POINT ( 'NONE',  ( 28.43384978605038071, -287.0457024460403659, -302.5633769229399945 ) ) ;
#25858 = CARTESIAN_POINT ( 'NONE',  ( -111.3896078978784061, -288.3990361931747657, -282.2736326078452862 ) ) ;
#25859 = ORIENTED_EDGE ( 'NONE', *, *, #43329, .T. ) ;
#25860 = CARTESIAN_POINT ( 'NONE',  ( 202.9738562182569694, 296.4636489450776367, -53.99999999999997868 ) ) ;
#25861 = CARTESIAN_POINT ( 'NONE',  ( 8.013246788581509961, -287.9202810026690145, -327.6404094554928861 ) ) ;
#25862 = FACE_OUTER_BOUND ( 'NONE', #55297, .T. ) ;
#25863 = CIRCLE ( 'NONE', #78817, 1.499999999999999556 ) ;
#25864 = CARTESIAN_POINT ( 'NONE',  ( -69.07820186173226773, -284.4006734740404454, -340.2726589327171496 ) ) ;
#25865 = CARTESIAN_POINT ( 'NONE',  ( 38.62085226948885008, -292.4675736104839530, -258.9356181331404514 ) ) ;
#25866 = CARTESIAN_POINT ( 'NONE',  ( -33.97126039139428144, -281.6940120787344881, -194.2356915295061697 ) ) ;
#25867 = CARTESIAN_POINT ( 'NONE',  ( -53.67165624039790828, -281.1621470493041102, -195.5631285387612195 ) ) ;
#25868 = CARTESIAN_POINT ( 'NONE',  ( -8.496194895253452728, -282.4970530477719990, -337.4203219174742117 ) ) ;
#25869 = CARTESIAN_POINT ( 'NONE',  ( -57.10327281808218203, -279.3071096973661156, -342.7647609468566543 ) ) ;
#25870 = CARTESIAN_POINT ( 'NONE',  ( -112.3058002325742706, -296.3314603799390738, -288.0074543607191799 ) ) ;
#25871 = CARTESIAN_POINT ( 'NONE',  ( -98.71533538762201943, -287.9931263058210220, -312.8703315742963014 ) ) ;
#25872 = CARTESIAN_POINT ( 'NONE',  ( -63.17557711464727532, -296.6280401393570969, -201.7010257756815008 ) ) ;
#25873 = VERTEX_POINT ( 'NONE', #49372 ) ;
#25874 = ORIENTED_EDGE ( 'NONE', *, *, #58963, .F. ) ;
#25875 = DIRECTION ( 'NONE',  ( 0.000000000000000000, 0.000000000000000000, 1.000000000000000000 ) ) ;
#25876 = CARTESIAN_POINT ( 'NONE',  ( -110.9179070595490089, -286.3217628247462585, -281.9984686515474550 ) ) ;
#25877 = CARTESIAN_POINT ( 'NONE',  ( -71.92229973248871033, -296.5782507635937009, -338.8131058422523552 ) ) ;
#25878 = CARTESIAN_POINT ( 'NONE',  ( -109.9730360505223246, -285.0887293693722881, -279.0787349729150719 ) ) ;
#25879 = EDGE_CURVE ( 'NONE', #22798, #90266, #58001, .T. ) ;
#25880 = CARTESIAN_POINT ( 'NONE',  ( -41.38407786455062620, -276.1606034625448274, -347.0324849042550568 ) ) ;
#25881 = CARTESIAN_POINT ( 'NONE',  ( -113.9061788668451953, -291.3000616905659967, -262.6554331680857217 ) ) ;
#25882 = CARTESIAN_POINT ( 'NONE',  ( -40.73701479434670603, -284.1495964752608074, -194.6210743333838877 ) ) ;
#25883 = CARTESIAN_POINT ( 'NONE',  ( -74.67236002090217539, -291.9025490433749610, -203.0397534426279833 ) ) ;
#25884 = CARTESIAN_POINT ( 'NONE',  ( -69.97808810469915386, -289.8275995896190125, -335.6969039014205123 ) ) ;
#25885 = DIRECTION ( 'NONE',  ( 5.551115123125777653E-14, 0.000000000000000000, 1.000000000000000000 ) ) ;
#25886 = DIRECTION ( 'NONE',  ( 0.000000000000000000, 0.000000000000000000, 1.000000000000000000 ) ) ;
#25887 = CARTESIAN_POINT ( 'NONE',  ( -12.12095700411519239, -92.64272014086816398, -356.3117460650181556 ) ) ;
#25888 = CARTESIAN_POINT ( 'NONE',  ( -87.84800523043182352, -285.2628329593632657, -327.6314872641165721 ) ) ;
#25889 = CARTESIAN_POINT ( 'NONE',  ( 31.95455697924147032, -291.4809262143061233, -303.7686719486574702 ) ) ;
#25890 = ORIENTED_EDGE ( 'NONE', *, *, #33498, .F. ) ;
#25891 = CARTESIAN_POINT ( 'NONE',  ( 17.82845731876507855, -281.1583948601936527, -318.6361612399400087 ) ) ;
#25892 = CARTESIAN_POINT ( 'NONE',  ( -31.45611935868447517, -276.6466098803346085, -347.1672559327260501 ) ) ;
#25893 = CARTESIAN_POINT ( 'NONE',  ( -110.6891459279048036, -280.7440893819315306, -255.4581790320177390 ) ) ;
#25894 = CARTESIAN_POINT ( 'NONE',  ( 47.06908910409267577, 10.77964184115877444, -330.2742531180653600 ) ) ;
#25895 = CARTESIAN_POINT ( 'NONE',  ( 35.61852786047657560, -279.8394870554832892, -247.6584435863159683 ) ) ;
#25896 = CARTESIAN_POINT ( 'NONE',  ( -69.46032988677893627, -283.6474778697021293, -202.9657143351045931 ) ) ;
#25897 = CARTESIAN_POINT ( 'NONE',  ( -94.17585406997072539, -275.1019723504455214, -220.2593772175699200 ) ) ;
#25898 = CARTESIAN_POINT ( 'NONE',  ( -98.78165813105036364, -296.4966903541272245, -309.9900991268975190 ) ) ;
#25899 = ORIENTED_EDGE ( 'NONE', *, *, #27474, .T. ) ;
#25900 = CARTESIAN_POINT ( 'NONE',  ( -0.9983329195906816000, -291.2301665409301563, -206.4685099808981761 ) ) ;
#25901 = CARTESIAN_POINT ( 'NONE',  ( 21.65776030399775820, -276.8681311117747441, -319.6802466823783675 ) ) ;
#25902 = CARTESIAN_POINT ( 'NONE',  ( 5.176745952576675691, -274.6449562451687711, -210.9590948345535537 ) ) ;
#25903 = CARTESIAN_POINT ( 'NONE',  ( 4.705225719283427033, -273.5255036196151650, -206.1611522513642001 ) ) ;
#25904 = CARTESIAN_POINT ( 'NONE',  ( 221.8344101925596306, -44.55766379199612004, -21.50000000000000000 ) ) ;
#25905 = CARTESIAN_POINT ( 'NONE',  ( -73.39312330142507790, -271.5741868509902588, -204.5368220061378679 ) ) ;
#25906 = ADVANCED_FACE ( 'NONE', ( #63142 ), #92435, .F. ) ;
#25907 = DIRECTION ( 'NONE',  ( -0.6249999999999139577, -7.583341244675574300E-14, 0.7806247497998688445 ) ) ;
#25908 = CARTESIAN_POINT ( 'NONE',  ( -43.50152060878402693, -252.4623848617872852, -489.6796197559582424 ) ) ;
#25909 = CARTESIAN_POINT ( 'NONE',  ( -34.82220260114848998, -284.0994702711495279, -343.6394122138794955 ) ) ;
#25910 = CARTESIAN_POINT ( 'NONE',  ( 13.02609450617649856, -284.1204937703224687, -327.3263356395374331 ) ) ;
#25911 = CARTESIAN_POINT ( 'NONE',  ( -108.7627168652007015, -284.1068285045616904, -254.7164616514315867 ) ) ;
#25912 = CARTESIAN_POINT ( 'NONE',  ( -5.954693553600145073, -275.0324268516998245, -337.1679706702036583 ) ) ;
#25913 = CARTESIAN_POINT ( 'NONE',  ( 33.41576028726181136, -283.7072990443342633, -292.9841591951132500 ) ) ;
#25914 = CARTESIAN_POINT ( 'NONE',  ( -91.49033523150968961, -276.3202306914116662, -320.4216960292102954 ) ) ;
#25915 = CARTESIAN_POINT ( 'NONE',  ( 82.64890176555634582, -299.5541904835127980, -195.3611179825600175 ) ) ;
#25916 = CARTESIAN_POINT ( 'NONE',  ( 24.04485864437597442, -276.0788496436803712, -230.2872302795820190 ) ) ;
#25917 = DIRECTION ( 'NONE',  ( 0.000000000000000000, 0.000000000000000000, 1.000000000000000000 ) ) ;
#25918 = CARTESIAN_POINT ( 'NONE',  ( -90.95284487861292178, -280.1175249442051722, -215.2414600216427800 ) ) ;
#25919 = ORIENTED_EDGE ( 'NONE', *, *, #31277, .T. ) ;
#25920 = EDGE_LOOP ( 'NONE', ( #76931, #20040, #69555, #28259 ) ) ;
#25921 = EDGE_CURVE ( 'NONE', #27188, #46489, #5064, .T. ) ;
#25922 = LINE ( 'NONE', #83683, #65654 ) ;
#25923 = CARTESIAN_POINT ( 'NONE',  ( -98.36372191485419592, -287.0198539397164268, -225.3679876411632392 ) ) ;
#25924 = CARTESIAN_POINT ( 'NONE',  ( -80.25774089342543505, -294.8475509580432572, -329.6132501932872287 ) ) ;
#25925 = CARTESIAN_POINT ( 'NONE',  ( -78.08943754177407470, -288.9328766953452146, -335.6377647308412975 ) ) ;
#25926 = CARTESIAN_POINT ( 'NONE',  ( 36.46049290610081783, -285.8730302373453469, -276.5886039220040402 ) ) ;
#25928 = CARTESIAN_POINT ( 'NONE',  ( -90.52915840012502713, -289.5256324248924784, -218.8920175849421526 ) ) ;
#25927 = CARTESIAN_POINT ( 'NONE',  ( 24.03546739342869643, -285.5670452915640567, -229.6705733914454299 ) ) ;
#25929 = CARTESIAN_POINT ( 'NONE',  ( -91.02145377976198404, -285.0412516402019492, -320.4172320241023044 ) ) ;
#25930 = CARTESIAN_POINT ( 'NONE',  ( 35.99526119829556592, -273.3495455935378118, -254.5939179653592817 ) ) ;
#25931 = CARTESIAN_POINT ( 'NONE',  ( -32.33838369109098920, -284.5140983906240422, -194.3125229451406710 ) ) ;
#25932 = CARTESIAN_POINT ( 'NONE',  ( -33.48931516368976702, -300.1005329123065053, -195.3597958697542651 ) ) ;
#25933 = CARTESIAN_POINT ( 'NONE',  ( 32.33313569441546065, -285.9204056174309585, -298.7032872206346497 ) ) ;
#25934 = AXIS2_PLACEMENT_3D ( 'NONE', #18318, #11215, #32992 ) ;
#25935 = CARTESIAN_POINT ( 'NONE',  ( -27.53870865084137520, -281.1208579356245423, -197.7335285178276933 ) ) ;
#25936 = CARTESIAN_POINT ( 'NONE',  ( -23.62097655468325286, -290.8774919726514554, -344.3177367053257854 ) ) ;
#25937 = CARTESIAN_POINT ( 'NONE',  ( 196.1963538710215857, 305.7026273589066250, -40.00000000000000711 ) ) ;
#25938 = CARTESIAN_POINT ( 'NONE',  ( 156.4851178187871312, 15.00000000000000000, -7.000000000000000888 ) ) ;
#25939 = CARTESIAN_POINT ( 'NONE',  ( -109.4186868777834576, -298.1814181051570927, -293.0808471850168644 ) ) ;
#25940 = VECTOR ( 'NONE', #19327, 1000.000000000000000 ) ;
#25941 = CARTESIAN_POINT ( 'NONE',  ( -24.50983114626673753, -278.2157762165726353, -196.4669789422241024 ) ) ;
#25942 = CARTESIAN_POINT ( 'NONE',  ( 30.76055634303483188, -292.2879753756741366, -234.6622587821045443 ) ) ;
#25943 = CARTESIAN_POINT ( 'NONE',  ( -97.06771932712487683, -294.3516957407734935, -313.7329324393978141 ) ) ;
#25944 = CARTESIAN_POINT ( 'NONE',  ( 34.82164466854323592, -280.0537429082800713, -256.3773019793481467 ) ) ;
#25945 = CARTESIAN_POINT ( 'NONE',  ( -16.20889725241792334, -272.4071833189682366, -198.9300645962699718 ) ) ;
#25946 = CARTESIAN_POINT ( 'NONE',  ( 30.30313881440716273, -294.4826289100929557, -241.5008806847925769 ) ) ;
#25947 = CARTESIAN_POINT ( 'NONE',  ( 10.59707575819634329, -295.1948066931273615, -210.1954327657594490 ) ) ;
#25948 = CARTESIAN_POINT ( 'NONE',  ( -93.14239701790498316, -295.7487493848604458, -218.2361083365121885 ) ) ;
#25949 = CARTESIAN_POINT ( 'NONE',  ( -25.09353482912474931, -293.1380283764050318, -345.4075125059563902 ) ) ;
#25950 = CARTESIAN_POINT ( 'NONE',  ( -110.2038140223481264, -291.8412104281912889, -280.7706324348624207 ) ) ;
#25951 = CARTESIAN_POINT ( 'NONE',  ( 170.2305261370685798, 249.5000000000000568, -24.90909090909089940 ) ) ;
#25952 = CARTESIAN_POINT ( 'NONE',  ( -34.86202760497246800, -292.8869309653617279, -197.2416749352204590 ) ) ;
#25953 = DIRECTION ( 'NONE',  ( -1.000000000000000000, 0.000000000000000000, 0.000000000000000000 ) ) ;
#25955 = CARTESIAN_POINT ( 'NONE',  ( 34.21648972488689822, -293.3617048441598740, -255.9241700721964321 ) ) ;
#25954 = CARTESIAN_POINT ( 'NONE',  ( -73.50919728821972399, -281.5492770470243613, -336.5277356159203919 ) ) ;
#25956 = CARTESIAN_POINT ( 'NONE',  ( -25.39559152602119596, -280.2004035161702404, -194.2934475221877619 ) ) ;
#25957 = CARTESIAN_POINT ( 'NONE',  ( -92.42157317789884985, -283.4809958903768461, -324.1379891848655461 ) ) ;
#25958 = CARTESIAN_POINT ( 'NONE',  ( -79.22099099712900738, -287.6181027501376093, -332.4408779614646505 ) ) ;
#25959 = FACE_OUTER_BOUND ( 'NONE', #30312, .T. ) ;
#25960 = CARTESIAN_POINT ( 'NONE',  ( 33.93293379882927496, -280.3801847030492809, -297.6124355655138061 ) ) ;
#25961 = CARTESIAN_POINT ( 'NONE',  ( 39.33131161188143210, -286.4516904057510942, -268.7052859836560401 ) ) ;
#25962 = DIRECTION ( 'NONE',  ( -0.000000000000000000, -1.000000000000000000, -0.000000000000000000 ) ) ;
#25963 = CARTESIAN_POINT ( 'NONE',  ( 29.12381975778757592, -295.5830270378971818, -302.5535620473963832 ) ) ;
#25964 = CARTESIAN_POINT ( 'NONE',  ( 34.65196760190284664, -277.3048094974898845, -296.1202706597088650 ) ) ;
#25965 = CARTESIAN_POINT ( 'NONE',  ( -76.82972323775312873, -279.1744091201867946, -208.8778553392625952 ) ) ;
#25966 = CARTESIAN_POINT ( 'NONE',  ( 38.81685847085416441, -293.8608073330497064, -281.7133845686021232 ) ) ;
#25967 = CARTESIAN_POINT ( 'NONE',  ( -93.34854435141173212, -281.9297358671645384, -321.1006031169986841 ) ) ;
#25968 = CARTESIAN_POINT ( 'NONE',  ( 22.78795225624744702, -292.0298258460766760, -228.5319202577205999 ) ) ;
#25969 = CARTESIAN_POINT ( 'NONE',  ( -86.14111594483458134, -295.3757364897904267, -213.3399077614377859 ) ) ;
#25970 = VERTEX_POINT ( 'NONE', #13403 ) ;
#25971 = CARTESIAN_POINT ( 'NONE',  ( 156.4217629211117355, 119.0463968525363327, 7.000000000000000000 ) ) ;
#25972 = CARTESIAN_POINT ( 'NONE',  ( 30.64052013739363645, -293.4190888271538142, -297.2652736617739606 ) ) ;
#25973 = CARTESIAN_POINT ( 'NONE',  ( 206.1704063851378805, -4.856322230924656715E-17, -7.166288341785295835 ) ) ;
#25974 = CARTESIAN_POINT ( 'NONE',  ( -37.30987171927208834, -289.5523547857346784, -200.3611179825600459 ) ) ;
#25975 = CARTESIAN_POINT ( 'NONE',  ( -46.09112082227374430, -297.0024990591858227, -194.0966580412323879 ) ) ;
#25976 = CARTESIAN_POINT ( 'NONE',  ( 37.20589397083265482, -279.8645778220592888, -283.9593905875534006 ) ) ;
#25977 = CARTESIAN_POINT ( 'NONE',  ( -7.550713321903794295, -287.7496544439184163, -199.8364319631869819 ) ) ;
#25978 = CARTESIAN_POINT ( 'NONE',  ( -13.28987695017997339, -288.5641777071908223, -339.2850601675242501 ) ) ;
#25979 = B_SPLINE_CURVE_WITH_KNOTS ( 'NONE', 3,
 ( #10879, #53038, #40675, #89952 ),
 .UNSPECIFIED., .F., .F.,
 ( 4, 4 ),
 ( 0.000000000000000000, 9.632970524408665937E-05 ),
 .UNSPECIFIED. ) ;
#25980 = CARTESIAN_POINT ( 'NONE',  ( -41.88012481404229703, -278.6304674994204333, -343.9272871104193996 ) ) ;
#25981 = CARTESIAN_POINT ( 'NONE',  ( -110.6565072384489667, -294.7541120833667492, -256.2651225882140693 ) ) ;
#25982 = CARTESIAN_POINT ( 'NONE',  ( -78.08829503046197829, -299.2566856577523708, -208.5120695833952595 ) ) ;
#25983 = CARTESIAN_POINT ( 'NONE',  ( -106.8156270863670159, -277.6618542183446721, -246.5301755951784628 ) ) ;
#25984 = VERTEX_POINT ( 'NONE', #78265 ) ;
#25985 = CARTESIAN_POINT ( 'NONE',  ( -34.75605588228874154, -297.7504167085210725, -193.3824032948462843 ) ) ;
#25986 = CARTESIAN_POINT ( 'NONE',  ( -64.32041632493388761, -291.3269781072776823, -339.7954894076447090 ) ) ;
#25987 = CARTESIAN_POINT ( 'NONE',  ( 14.87497259471225597, -294.3732118444519301, -214.7922058508447094 ) ) ;
#25988 = CARTESIAN_POINT ( 'NONE',  ( -113.5000000000000568, -211.8141737103562434, -420.2472828204663529 ) ) ;
#25989 = CARTESIAN_POINT ( 'NONE',  ( -109.2777500221154980, -291.0322660237165451, -283.3648633678579358 ) ) ;
#25990 = CARTESIAN_POINT ( 'NONE',  ( -48.18343439339133027, -255.1274621574002310, -454.6030467723235802 ) ) ;
#25991 = EDGE_CURVE ( 'NONE', #39736, #8402, #70013, .T. ) ;
#25992 = CARTESIAN_POINT ( 'NONE',  ( -114.2082137319480495, -297.2488066404342248, -266.7483527591360826 ) ) ;
#25993 = CARTESIAN_POINT ( 'NONE',  ( -98.88106252421087561, -288.0961862353857441, -314.5785168999652228 ) ) ;
#25994 = CARTESIAN_POINT ( 'NONE',  ( -35.83292491741726593, -298.4038377470325827, -193.3821790908798448 ) ) ;
#25995 = CARTESIAN_POINT ( 'NONE',  ( 175.2296996224750103, 250.0000000000000568, 25.00000000000000355 ) ) ;
#25996 = AXIS2_PLACEMENT_3D ( 'NONE', #60677, #17113, #33180 ) ;
#25997 = CARTESIAN_POINT ( 'NONE',  ( 195.1350936496258441, 26.65530528383335707, 15.12636463707340617 ) ) ;
#25998 = CARTESIAN_POINT ( 'NONE',  ( -26.22625983952692152, -290.4332267996190353, -345.8538642469735009 ) ) ;
#25999 = CARTESIAN_POINT ( 'NONE',  ( -55.56934967048406548, -297.7662352645559167, -350.3683826091709648 ) ) ;
#26000 = CARTESIAN_POINT ( 'NONE',  ( -109.8102806463183470, -286.7926487064293042, -251.6974295125035042 ) ) ;
#26001 = CARTESIAN_POINT ( 'NONE',  ( 19.17609989929905367, -286.8313636216280429, -321.8037927117418917 ) ) ;
#26002 = CARTESIAN_POINT ( 'NONE',  ( -60.00726863166994463, -271.7577189236351387, -198.9885707427638124 ) ) ;
#26003 = CARTESIAN_POINT ( 'NONE',  ( -104.5148179467219904, -274.8977431781710266, -238.2817408471631211 ) ) ;
#26005 = CARTESIAN_POINT ( 'NONE',  ( -111.8076809284111874, -288.6573627805786373, -268.3998938313917506 ) ) ;
#26004 = CONICAL_SURFACE ( 'NONE', #10922, 4.025000000000000355, 0.7853981633973095011 ) ;
#26006 = CARTESIAN_POINT ( 'NONE',  ( -102.5307339521301344, -279.9001831262722817, -309.0734714049813192 ) ) ;
#26007 = ORIENTED_EDGE ( 'NONE', *, *, #13993, .F. ) ;
#26009 = CARTESIAN_POINT ( 'NONE',  ( 9.348007857893522399, -280.0619235614337867, -214.0460021404753945 ) ) ;
#26008 = CARTESIAN_POINT ( 'NONE',  ( -64.81611647204123017, -279.6830500953275873, -202.7286077041536601 ) ) ;
#26010 = CARTESIAN_POINT ( 'NONE',  ( -5.400930296626684779, -277.7213310088902745, -340.0839961038166166 ) ) ;
#26011 = CARTESIAN_POINT ( 'NONE',  ( 5.972438054300714505, -279.4204340743924604, -207.1796796385847870 ) ) ;
#26012 = CARTESIAN_POINT ( 'NONE',  ( 191.7941899171395050, 277.5480571852982621, -124.4921890884961044 ) ) ;
#26013 = CARTESIAN_POINT ( 'NONE',  ( 30.34128672008207417, -276.9642122907782777, -306.6926298764308285 ) ) ;
#26014 = EDGE_CURVE ( 'NONE', #92711, #27803, #85355, .T. ) ;
#26016 = ADVANCED_FACE ( 'NONE', ( #71160 ), #30268, .F. ) ;
#26015 = CONTEXT_DEPENDENT_SHAPE_REPRESENTATION ( #12381, #5860 ) ;
#26017 = CARTESIAN_POINT ( 'NONE',  ( 17.57702608577497827, -276.3395470037212931, -217.3075452942337620 ) ) ;
#26018 = CARTESIAN_POINT ( 'NONE',  ( 31.95455697924148097, -295.6233781216988632, -236.9535640164627637 ) ) ;
#26019 = VERTEX_POINT ( 'NONE', #88004 ) ;
#26020 = CARTESIAN_POINT ( 'NONE',  ( 199.0872936271226195, 69.92583464099143953, 8.677435037599675383 ) ) ;
#26021 = CARTESIAN_POINT ( 'NONE',  ( 32.56422592585744979, -288.3399062829817012, -248.2422612819088386 ) ) ;
#26022 = CARTESIAN_POINT ( 'NONE',  ( 37.29064029720369433, -289.1312849151976252, -256.0786889738105856 ) ) ;
#26023 = CARTESIAN_POINT ( 'NONE',  ( -74.77521517568500542, -288.9132882718096198, -333.1661488197501058 ) ) ;
#26024 = CARTESIAN_POINT ( 'NONE',  ( 18.31132212942786808, -286.3320889499269128, -217.1592540323484002 ) ) ;
#26025 = LINE ( 'NONE', #76232, #15832 ) ;
#26026 = CARTESIAN_POINT ( 'NONE',  ( -15.91953365755882999, -281.1702681912662456, -340.9835733159463302 ) ) ;
#26027 = CARTESIAN_POINT ( 'NONE',  ( 35.77996097544042442, -289.2426465812927177, -257.2619838698184367 ) ) ;
#26028 = CARTESIAN_POINT ( 'NONE',  ( -92.19394283087996200, -282.3341691312779176, -319.5933136778693324 ) ) ;
#26029 = CARTESIAN_POINT ( 'NONE',  ( -103.8230523382779182, -280.2892044020557591, -238.9129695797552415 ) ) ;
#26030 = CARTESIAN_POINT ( 'NONE',  ( -96.13880100621362601, -278.4369101236103461, -313.7513074768925208 ) ) ;
#26031 = CARTESIAN_POINT ( 'NONE',  ( -111.6058214604120167, -289.5839374805772195, -251.5240505808429816 ) ) ;
#26032 = CARTESIAN_POINT ( 'NONE',  ( -76.03426885895893861, -286.3522133154978633, -203.9142718908119321 ) ) ;
#26033 = CARTESIAN_POINT ( 'NONE',  ( -67.17099252333942161, -286.1637426408757960, -199.4404565464750760 ) ) ;
#26034 = CARTESIAN_POINT ( 'NONE',  ( 31.35531949319808476, -282.0494607849622639, -295.2030881855080224 ) ) ;
#26035 = VERTEX_POINT ( 'NONE', #6288 ) ;
#26036 = CARTESIAN_POINT ( 'NONE',  ( 144.7857639756989272, -299.5541904835127980, -201.0153591320744226 ) ) ;
#26037 = CARTESIAN_POINT ( 'NONE',  ( -98.22635587058518070, -293.0220020018754781, -225.2465365023012112 ) ) ;
#26038 = CARTESIAN_POINT ( 'NONE',  ( 21.83851085360088717, -291.5817081253803735, -221.8739969824914340 ) ) ;
#26039 = CARTESIAN_POINT ( 'NONE',  ( 23.25373406459102199, -274.0405107072245414, -229.2095317962383092 ) ) ;
#26040 = CARTESIAN_POINT ( 'NONE',  ( -113.8426565258949097, -295.8030002700830892, -278.1660175096241119 ) ) ;
#26041 = CARTESIAN_POINT ( 'NONE',  ( -14.61435826916151370, -290.8320132361100718, -200.2599362279293302 ) ) ;
#26042 = CARTESIAN_POINT ( 'NONE',  ( -26.07496108187088879, -293.1465899394908092, -343.5118842319939176 ) ) ;
#26043 = CARTESIAN_POINT ( 'NONE',  ( -61.37059979273382737, -290.5764043571346633, -339.7134249763361140 ) ) ;
#26044 = CARTESIAN_POINT ( 'NONE',  ( -54.94434090351493438, -232.1443419142230766, 25.50000000000000000 ) ) ;
#26045 = CARTESIAN_POINT ( 'NONE',  ( -59.41374184840418593, -291.3381026886466429, -342.0397453468048639 ) ) ;
#26046 = CARTESIAN_POINT ( 'NONE',  ( 20.80757616961971479, -290.8968325258275058, -222.7303495992310047 ) ) ;
#26047 = CARTESIAN_POINT ( 'NONE',  ( -23.05680853957240117, -296.8697261290107576, -344.0404940969793302 ) ) ;
#26048 = CARTESIAN_POINT ( 'NONE',  ( -89.83986342218533139, -286.2300706523702729, -219.2261023316000887 ) ) ;
#26049 = CARTESIAN_POINT ( 'NONE',  ( -14.31877491325872498, -296.7544549666146736, -341.9151069641986851 ) ) ;
#26050 = CARTESIAN_POINT ( 'NONE',  ( 29.77367096495504839, -277.0811197690114795, -236.0984011776297109 ) ) ;
#26051 = CARTESIAN_POINT ( 'NONE',  ( -71.40812745150046226, -276.2869881701229247, -338.9722486371768468 ) ) ;
#26052 = CARTESIAN_POINT ( 'NONE',  ( -51.76026743750345815, -297.0694932703931386, -194.8332977247179372 ) ) ;
#26053 = CARTESIAN_POINT ( 'NONE',  ( 36.71235791054292719, -273.8084387491682605, -271.6243233130498425 ) ) ;
#26054 = CARTESIAN_POINT ( 'NONE',  ( -16.49548198456003689, -278.4034813065742355, -198.8995941773991945 ) ) ;
#26055 = CARTESIAN_POINT ( 'NONE',  ( -91.42545596482558778, -274.4656484517480521, -220.7231790146008450 ) ) ;
#26056 = CARTESIAN_POINT ( 'NONE',  ( 37.37310244894115385, -273.9243407237918291, -254.2896803181082248 ) ) ;
#26057 = CARTESIAN_POINT ( 'NONE',  ( 200.9021118021030361, 65.55478020306156850, 5.267193185414368095 ) ) ;
#26058 = CARTESIAN_POINT ( 'NONE',  ( -37.15945358355362060, -298.8573334823564096, -197.1967596271784373 ) ) ;
#26059 = DIRECTION ( 'NONE',  ( -1.000000000000000000, -0.000000000000000000, -0.000000000000000000 ) ) ;
#26061 = CARTESIAN_POINT ( 'NONE',  ( -27.28807909573529855, -274.0166624069921681, -198.0058300916056453 ) ) ;
#26060 = CARTESIAN_POINT ( 'NONE',  ( -48.64766019395676722, -287.2153937429500274, -344.9161409946593153 ) ) ;
#26062 = CIRCLE ( 'NONE', #403, 2.999999999999998224 ) ;
#26063 = CARTESIAN_POINT ( 'NONE',  ( -4.333064003954842036, -288.6290358601492585, -339.9416088546569767 ) ) ;
#26064 = CARTESIAN_POINT ( 'NONE',  ( -97.27629017015085822, -289.5709119568793426, -318.6891446004945010 ) ) ;
#26065 = CARTESIAN_POINT ( 'NONE',  ( -64.96310334541979614, -299.6731539603272836, -200.1949611922445058 ) ) ;
#26066 = CARTESIAN_POINT ( 'NONE',  ( -37.01243542350478322, -293.0478298053715207, -345.2064670110290763 ) ) ;
#26067 = TOROIDAL_SURFACE ( 'NONE', #68399, 24.50000000000000355, 0.5000000000000000000 ) ;
#26068 = CARTESIAN_POINT ( 'NONE',  ( 38.26484454770362476, -280.9219902866428811, -284.1384982832373680 ) ) ;
#26069 = DIRECTION ( 'NONE',  ( -0.000000000000000000, -1.000000000000000000, -0.000000000000000000 ) ) ;
#26070 = CIRCLE ( 'NONE', #48783, 3.038598599789554822 ) ;
#26071 = CARTESIAN_POINT ( 'NONE',  ( -109.5054175807851493, -276.8170090409134900, -249.7470011854615279 ) ) ;
#26072 = CARTESIAN_POINT ( 'NONE',  ( 175.2296996224750103, 250.5000000000000568, 25.00000000000000355 ) ) ;
#26073 = CARTESIAN_POINT ( 'NONE',  ( -18.38567190830197262, -287.5974808934334987, -341.3209646584199390 ) ) ;
#26074 = DIRECTION ( 'NONE',  ( -0.000000000000000000, -1.000000000000000000, -0.000000000000000000 ) ) ;
#26075 = CARTESIAN_POINT ( 'NONE',  ( -110.3691898909241473, -288.7721169183628831, -253.2175816028796476 ) ) ;
#26076 = CARTESIAN_POINT ( 'NONE',  ( 13.96563049481983221, -276.3083346064670422, -217.4624830674252394 ) ) ;
#26077 = CARTESIAN_POINT ( 'NONE',  ( -13.58774896038472590, -284.1749438286296368, -342.9858802593784617 ) ) ;
#26079 = CARTESIAN_POINT ( 'NONE',  ( -78.37662955577970081, -283.6216535731053909, -330.7360678116390886 ) ) ;
#26078 = CARTESIAN_POINT ( 'NONE',  ( -56.93716887924511383, -295.8209000051339785, -197.5442296542422582 ) ) ;
#26080 = CARTESIAN_POINT ( 'NONE',  ( -34.03219620597342043, -275.5198675056001889, -196.8463432638048971 ) ) ;
#26081 = CARTESIAN_POINT ( 'NONE',  ( 34.78312190811930549, -276.1924732490160750, -258.0143686126671696 ) ) ;
#26082 = EDGE_CURVE ( 'NONE', #11326, #41151, #65513, .T. ) ;
#26083 = CARTESIAN_POINT ( 'NONE',  ( 35.26228161896224123, -283.7939573929965036, -289.1670342401912990 ) ) ;
#26084 = CARTESIAN_POINT ( 'NONE',  ( -57.95958171669895620, -296.8379144666615161, -200.0879978985657033 ) ) ;
#26085 = VERTEX_POINT ( 'NONE', #28081 ) ;
#26086 = CARTESIAN_POINT ( 'NONE',  ( 203.5005663465542227, 292.0167436573144073, -53.99999999998427569 ) ) ;
#26087 = CARTESIAN_POINT ( 'NONE',  ( 21.36627390962075879, -294.0570793758699892, -320.1845440882959224 ) ) ;
#26088 = CARTESIAN_POINT ( 'NONE',  ( -97.09747876138567335, -287.1460866091586581, -225.6275318811606212 ) ) ;
#26089 = DIRECTION ( 'NONE',  ( -0.000000000000000000, -1.000000000000000000, -0.000000000000000000 ) ) ;
#26090 = CARTESIAN_POINT ( 'NONE',  ( -88.52914483777347243, -281.1952119285918457, -334.4957818155094174 ) ) ;
#26091 = CARTESIAN_POINT ( 'NONE',  ( -101.9667318183248028, -277.2017182563430424, -312.0246084118936665 ) ) ;
#26092 = CARTESIAN_POINT ( 'NONE',  ( -113.5898514270250814, -288.9414302369593770, -271.1994052677522404 ) ) ;
#26093 = CARTESIAN_POINT ( 'NONE',  ( -93.94227847450628133, -285.4089046709201511, -317.5530906591745861 ) ) ;
#26094 = CARTESIAN_POINT ( 'NONE',  ( -16.06846345869654513, -278.5335665624714352, -341.3050887445962758 ) ) ;
#26095 = CARTESIAN_POINT ( 'NONE',  ( -34.48270525082197935, -284.4421412028659688, -346.7183864147860959 ) ) ;
#26096 = CARTESIAN_POINT ( 'NONE',  ( -38.90886268173343865, -281.8671319001777533, -343.7540180332204045 ) ) ;
#26097 = CARTESIAN_POINT ( 'NONE',  ( -66.88022731131943033, -281.6652702869935752, -201.4088982050968468 ) ) ;
#26098 = CARTESIAN_POINT ( 'NONE',  ( -36.94186363751468605, -274.2237397348851573, -193.3491040225014501 ) ) ;
#26099 = CARTESIAN_POINT ( 'NONE',  ( -98.80470547715859198, -277.7675484001170503, -316.7648563595901692 ) ) ;
#26100 = CARTESIAN_POINT ( 'NONE',  ( -105.2402377331540038, -298.0677319908579079, -301.0010048126023321 ) ) ;
#26101 = CARTESIAN_POINT ( 'NONE',  ( 139.6539576904058606, 275.0000000000000568, 10.50000000000000000 ) ) ;
#26102 = CARTESIAN_POINT ( 'NONE',  ( 193.9153122143737562, 249.5000000000000568, 17.21343741151142481 ) ) ;
#26103 = CARTESIAN_POINT ( 'NONE',  ( -102.7709606978420425, -295.1981239826878323, -232.0567677047278607 ) ) ;
#26104 = CARTESIAN_POINT ( 'NONE',  ( 23.10676946594754355, -274.4893430611577969, -229.3024594146004915 ) ) ;
#26105 = CARTESIAN_POINT ( 'NONE',  ( -106.4914070761503950, -274.1819324983832189, -237.4016467116934450 ) ) ;
#26106 = CARTESIAN_POINT ( 'NONE',  ( 33.63545407948539179, -289.0379334093533998, -249.3350936155565876 ) ) ;
#26107 = CARTESIAN_POINT ( 'NONE',  ( -96.85442100317582970, -297.4262955277986293, -318.1410186158751117 ) ) ;
#26108 = CARTESIAN_POINT ( 'NONE',  ( 39.21063590991850845, -294.7922198035330439, -273.1447423540707860 ) ) ;
#26109 = CARTESIAN_POINT ( 'NONE',  ( -97.22034534473348799, -291.9374302999586916, -315.2665251349304185 ) ) ;
#26110 = CARTESIAN_POINT ( 'NONE',  ( 1.369612232640303517, -278.5700010460427052, -206.2584598251917498 ) ) ;
#26111 = CARTESIAN_POINT ( 'NONE',  ( -88.53840235861714802, -281.2480841865800016, -216.2508744886622196 ) ) ;
#26112 = CARTESIAN_POINT ( 'NONE',  ( -111.8143612772104944, -294.6537860262340587, -268.6763776530343080 ) ) ;
#26113 = CARTESIAN_POINT ( 'NONE',  ( -37.29090667048291863, -284.9118958114838165, -346.1387607599690455 ) ) ;
#26114 = CARTESIAN_POINT ( 'NONE',  ( 11.34959314314943235, -285.6659927943284742, -215.4897632967589800 ) ) ;
#26115 = CARTESIAN_POINT ( 'NONE',  ( -102.4785513481026697, -256.8849682556987659, -326.4804194469078880 ) ) ;
#26116 = ORIENTED_EDGE ( 'NONE', *, *, #15864, .T. ) ;
#26117 = CARTESIAN_POINT ( 'NONE',  ( -110.3303337026201660, -284.2476015338562547, -268.1823900040998296 ) ) ;
#26118 = ORIENTED_EDGE ( 'NONE', *, *, #86488, .T. ) ;
#26119 = CARTESIAN_POINT ( 'NONE',  ( 24.33492938005380779, -282.0236205127432072, -224.7816721431527753 ) ) ;
#26121 = CARTESIAN_POINT ( 'NONE',  ( -32.69392468982429278, -274.4455899300057240, -197.4755088537584982 ) ) ;
#26120 = VECTOR ( 'NONE', #89158, 1000.000000000000000 ) ;
#26122 = CARTESIAN_POINT ( 'NONE',  ( -43.61834939641957476, -284.7695806793934707, -193.9627842113003737 ) ) ;
#26123 = CARTESIAN_POINT ( 'NONE',  ( -35.35417049297698355, -281.0177428821261287, -193.6090484366914950 ) ) ;
#26124 = CARTESIAN_POINT ( 'NONE',  ( -77.14750778924423003, -281.0493906768019201, -205.1984387805477468 ) ) ;
#26125 = CARTESIAN_POINT ( 'NONE',  ( -4.956745876385824090, -280.8002895305701827, -200.5258902693329617 ) ) ;
#26126 = CARTESIAN_POINT ( 'NONE',  ( 34.45848030099739390, -285.0523547857347353, -270.3937649182068412 ) ) ;
#26127 = CARTESIAN_POINT ( 'NONE',  ( -109.4453526793423066, -267.4301006796197271, -307.0599045550397364 ) ) ;
#26128 = ORIENTED_EDGE ( 'NONE', *, *, #69089, .T. ) ;
#26129 = AXIS2_PLACEMENT_3D ( 'NONE', #226, #56614, #57078 ) ;
#26130 = CARTESIAN_POINT ( 'NONE',  ( -77.57072815873762295, -275.5109923778701386, -207.2607714784864470 ) ) ;
#26131 = CARTESIAN_POINT ( 'NONE',  ( 167.4490855713348481, 232.7245837427465176, -192.5400704262254976 ) ) ;
#26132 = AXIS2_PLACEMENT_3D ( 'NONE', #25227, #47452, #68793 ) ;
#26133 = CARTESIAN_POINT ( 'NONE',  ( 34.53663548003434869, -279.8325073027585859, -290.4944653137752653 ) ) ;
#26134 = CARTESIAN_POINT ( 'NONE',  ( 18.65356931988779721, -294.6040879910829062, -218.9947494755392370 ) ) ;
#26135 = CARTESIAN_POINT ( 'NONE',  ( -95.69069826749094432, -295.2827579884799434, -314.4190790278208283 ) ) ;
#26136 = CARTESIAN_POINT ( 'NONE',  ( -27.85045997660992256, -291.6771111854073411, -193.9566952136810301 ) ) ;
#26137 = AXIS2_PLACEMENT_3D ( 'NONE', #125, #71175, #27613 ) ;
#26139 = CARTESIAN_POINT ( 'NONE',  ( 10.61987620586390335, -286.7767461549710220, -326.5190247029905777 ) ) ;
#26138 = CARTESIAN_POINT ( 'NONE',  ( -108.8922377041888581, -294.7833688486718984, -297.3270354571271810 ) ) ;
#26140 = CARTESIAN_POINT ( 'NONE',  ( 35.28081334126409274, -295.6129955732050689, -285.8116592725950795 ) ) ;
#26141 = CARTESIAN_POINT ( 'NONE',  ( -95.49646321174276409, -285.2386426385939444, -315.3179101848080563 ) ) ;
#26142 = ORIENTED_EDGE ( 'NONE', *, *, #50050, .T. ) ;
#26143 = CARTESIAN_POINT ( 'NONE',  ( 30.69934612542391150, -294.9533403698755478, -305.9031527728337210 ) ) ;
#26144 = CIRCLE ( 'NONE', #53385, 4.999999999999976907 ) ;
#26145 = CARTESIAN_POINT ( 'NONE',  ( -53.69735112532745802, -283.7599596137549156, -341.6205559743822278 ) ) ;
#26146 = CARTESIAN_POINT ( 'NONE',  ( -86.15415973984993059, -294.5069593837021671, -329.3979920878251733 ) ) ;
#26147 = CARTESIAN_POINT ( 'NONE',  ( -111.7630761765779539, -291.1145909481658691, -289.5348561627811250 ) ) ;
#26148 = EDGE_CURVE ( 'NONE', #83549, #84679, #60962, .T. ) ;
#26149 = CARTESIAN_POINT ( 'NONE',  ( -111.1748761521547948, -291.3161115654262403, -248.7234420100204204 ) ) ;
#26150 = CARTESIAN_POINT ( 'NONE',  ( 33.99555490870849184, -287.5144700297938130, -254.8693121371360917 ) ) ;
#26151 = ORIENTED_EDGE ( 'NONE', *, *, #19791, .F. ) ;
#26152 = CARTESIAN_POINT ( 'NONE',  ( 208.6208076322478746, 32.98517505407394168, 12.09245862095555601 ) ) ;
#26153 = CARTESIAN_POINT ( 'NONE',  ( -107.7496587885240871, -298.7749155873104314, -242.2374380850581304 ) ) ;
#26154 = VECTOR ( 'NONE', #20504, 1000.000000000000000 ) ;
#26155 = CARTESIAN_POINT ( 'NONE',  ( -109.3808428249358542, -295.5642745168043461, -244.5995149352899887 ) ) ;
#26156 = EDGE_CURVE ( 'NONE', #78471, #75279, #15135, .T. ) ;
#26157 = CARTESIAN_POINT ( 'NONE',  ( -57.16542497158069835, -278.8487626894216191, -199.8598528817571491 ) ) ;
#26158 = ORIENTED_EDGE ( 'NONE', *, *, #19092, .F. ) ;
#26159 = CARTESIAN_POINT ( 'NONE',  ( -10.36331363604707789, -273.9024600337501170, -198.2510302314686328 ) ) ;
#26160 = CARTESIAN_POINT ( 'NONE',  ( -86.54900706896299312, -295.8333841890787994, -215.5035871002841077 ) ) ;
#26161 = CARTESIAN_POINT ( 'NONE',  ( -76.99593890458663736, -279.4495398642493456, -333.1782910029873506 ) ) ;
#26162 = CARTESIAN_POINT ( 'NONE',  ( 33.24355366231290532, -273.3898002537761158, -247.2045609470798979 ) ) ;
#26163 = CARTESIAN_POINT ( 'NONE',  ( 6.311353875102079236, -295.6497883543746639, -329.4290537440044773 ) ) ;
#26164 = CARTESIAN_POINT ( 'NONE',  ( -71.82249880952453225, -298.6648180824919336, -205.6529596047545567 ) ) ;
#26165 = DIRECTION ( 'NONE',  ( 0.000000000000000000, 0.000000000000000000, 1.000000000000000000 ) ) ;
#26166 = CARTESIAN_POINT ( 'NONE',  ( -103.1690878561906004, -298.6581110149653568, -231.8748585589185893 ) ) ;
#26167 = AXIS2_PLACEMENT_3D ( 'NONE', #35522, #56364, #29346 ) ;
#26168 = CARTESIAN_POINT ( 'NONE',  ( 17.73681752449018489, -296.7399187925757928, -195.2131683379656408 ) ) ;
#26169 = CARTESIAN_POINT ( 'NONE',  ( -62.84405102379453467, -292.3625797558493105, -201.8518283426166420 ) ) ;
#26170 = CARTESIAN_POINT ( 'NONE',  ( -110.2089398682156371, -288.9911257322809206, -280.7346875925552467 ) ) ;
#26171 = CARTESIAN_POINT ( 'NONE',  ( 175.2296996224750103, 138.1603916158177583, 24.00000000000001421 ) ) ;
#26172 = CARTESIAN_POINT ( 'NONE',  ( 39.64587940594230275, -276.0545568708947144, -271.1647373776706900 ) ) ;
#26173 = CARTESIAN_POINT ( 'NONE',  ( -69.49287347339856069, -273.7834252135151019, -204.8225640081446670 ) ) ;
#26174 = CARTESIAN_POINT ( 'NONE',  ( -85.76743759011073109, -281.3659185024981753, -212.5578739362005933 ) ) ;
#26175 = CARTESIAN_POINT ( 'NONE',  ( -21.84236188932190004, -281.5423374003972299, -345.2815343295065418 ) ) ;
#26176 = CIRCLE ( 'NONE', #80651, 24.00000000000000355 ) ;
#26177 = CARTESIAN_POINT ( 'NONE',  ( -110.5721501603655952, -277.6033801587836365, -293.9977866416802499 ) ) ;
#26178 = CARTESIAN_POINT ( 'NONE',  ( -109.3501439840259479, -283.9205375153651403, -257.3529300411557301 ) ) ;
#26179 = CARTESIAN_POINT ( 'NONE',  ( 37.69716120803162340, -279.6185947863154979, -275.5600907017386589 ) ) ;
#26180 = CARTESIAN_POINT ( 'NONE',  ( -69.73410430471044208, -272.1917306231412113, -204.2845936285694677 ) ) ;
#26181 = CARTESIAN_POINT ( 'NONE',  ( -39.13295541706094838, -279.0747583980505624, -345.3523673384785866 ) ) ;
#26182 = CARTESIAN_POINT ( 'NONE',  ( 209.9972545312790544, 27.55378999303206200, 10.50000000000000000 ) ) ;
#26183 = FACE_OUTER_BOUND ( 'NONE', #20210, .T. ) ;
#26184 = CARTESIAN_POINT ( 'NONE',  ( -54.34631544741656484, -296.0764771493508078, -196.3015671527024324 ) ) ;
#26185 = CARTESIAN_POINT ( 'NONE',  ( -53.70668583079725522, -279.2617067182699202, -343.7780391190101454 ) ) ;
#26186 = DIRECTION ( 'NONE',  ( 0.9693563597868444237, 0.2456588035076248677, -0.000000000000000000 ) ) ;
#26187 = CARTESIAN_POINT ( 'NONE',  ( -101.6789132476428250, -285.9445193253832826, -309.9848129720878660 ) ) ;
#26188 = VERTEX_POINT ( 'NONE', #36913 ) ;
#26189 = FACE_OUTER_BOUND ( 'NONE', #67270, .T. ) ;
#26190 = CARTESIAN_POINT ( 'NONE',  ( 19.81465046686824394, -284.8797099097091632, -221.7807704580023653 ) ) ;
#26191 = CARTESIAN_POINT ( 'NONE',  ( 175.2296996224750103, 20.99999999999998934, 0.000000000000000000 ) ) ;
#26192 = CARTESIAN_POINT ( 'NONE',  ( -66.22344206037546144, -294.2337965513641507, -337.8368579825529991 ) ) ;
#26193 = CARTESIAN_POINT ( 'NONE',  ( -34.55497165967804563, -287.1564851326424446, -344.5944194559388052 ) ) ;
#26194 = CARTESIAN_POINT ( 'NONE',  ( -78.59295187722810283, -208.2960365483323244, -357.4574221067172743 ) ) ;
#26195 = CARTESIAN_POINT ( 'NONE',  ( -89.49879168472884317, -295.3175821871124072, -216.3939369506339006 ) ) ;
#26196 = CARTESIAN_POINT ( 'NONE',  ( -29.51463500701300191, -284.6294643323478795, -194.4569362553195049 ) ) ;
#26197 = CARTESIAN_POINT ( 'NONE',  ( 33.49683419924278382, -282.8814565027738013, -249.6646818075370220 ) ) ;
#26198 = CARTESIAN_POINT ( 'NONE',  ( 10.20661578122992807, -278.9371163177303856, -211.0219832338596291 ) ) ;
#26199 = CARTESIAN_POINT ( 'NONE',  ( -18.47350408722288861, -288.8023627039207213, -340.9331420923449514 ) ) ;
#26200 = TOROIDAL_SURFACE ( 'NONE', #70010, 4.499999999999990230, 0.5000000000000000000 ) ;
#26201 = CARTESIAN_POINT ( 'NONE',  ( -91.74455907582854763, -280.6822924227491285, -220.8060591492271669 ) ) ;
#26202 = CARTESIAN_POINT ( 'NONE',  ( -62.37378380844673131, -280.5209874317029062, -201.5617557106566835 ) ) ;
#26203 = CARTESIAN_POINT ( 'NONE',  ( 22.53872477945380481, -288.9085317885618451, -224.5934783862951463 ) ) ;
#26204 = VECTOR ( 'NONE', #91014, 1000.000000000000114 ) ;
#26205 = ORIENTED_EDGE ( 'NONE', *, *, #22448, .F. ) ;
#26206 = AXIS2_PLACEMENT_3D ( 'NONE', #11835, #4734, #62520 ) ;
#26207 = CARTESIAN_POINT ( 'NONE',  ( -38.35741159830598690, -274.0397491378665791, -193.3678174284907243 ) ) ;
#26208 = CARTESIAN_POINT ( 'NONE',  ( -76.71541153931548251, -291.5619509896136492, -333.7768703753266095 ) ) ;
#26209 = DIRECTION ( 'NONE',  ( 0.000000000000000000, -0.000000000000000000, -1.000000000000000000 ) ) ;
#26210 = CARTESIAN_POINT ( 'NONE',  ( 13.79469577742117714, -289.1948066931273615, -206.1857440867352693 ) ) ;
#26211 = ORIENTED_EDGE ( 'NONE', *, *, #35647, .F. ) ;
#26212 = CARTESIAN_POINT ( 'NONE',  ( 13.62102484138827840, -274.3405803007165673, -325.6843491442355116 ) ) ;
#26213 = DIRECTION ( 'NONE',  ( -0.000000000000000000, -1.000000000000000000, -0.000000000000000000 ) ) ;
#26214 = CARTESIAN_POINT ( 'NONE',  ( -11.34944951100359134, -293.1190857903790743, -342.0469987695511236 ) ) ;
#26215 = CARTESIAN_POINT ( 'NONE',  ( -35.80766856760973837, -297.5795176019383348, -197.2997115092137790 ) ) ;
#26216 = AXIS2_PLACEMENT_3D ( 'NONE', #7336, #5949, #5487 ) ;
#26217 = CARTESIAN_POINT ( 'NONE',  ( 24.09814257179160180, -289.6318585424685921, -311.0763553971066244 ) ) ;
#26218 = PRODUCT ( 'Square Mounting Plate', 'Square Mounting Plate', '', ( #17057 ) ) ;
#26219 = CARTESIAN_POINT ( 'NONE',  ( -13.17763998383056112, -284.4941976333578282, -340.3731186695097222 ) ) ;
#26220 = CARTESIAN_POINT ( 'NONE',  ( -86.15070591020423763, -292.8161348075420847, -211.5022055586851195 ) ) ;
#26221 = CARTESIAN_POINT ( 'NONE',  ( -101.8762173958342032, -291.3240794711874742, -311.5510866003369301 ) ) ;
#26222 = CARTESIAN_POINT ( 'NONE',  ( -4.957521955928856805, -288.4785857780137235, -202.6988564975496558 ) ) ;
#26223 = CARTESIAN_POINT ( 'NONE',  ( -95.90718960166142892, -279.3932942819733398, -220.3500321010474465 ) ) ;
#26224 = CARTESIAN_POINT ( 'NONE',  ( -107.5415120038456820, -294.9949542721644207, -242.2688745684934304 ) ) ;
#26225 = CARTESIAN_POINT ( 'NONE',  ( -30.21700538607526454, -282.7976833110919301, -347.0307907961067144 ) ) ;
#26226 = AXIS2_PLACEMENT_3D ( 'NONE', #59272, #37923, #67312 ) ;
#26227 = CARTESIAN_POINT ( 'NONE',  ( 32.26848328570245883, -277.0743390925360359, -244.5679436159495879 ) ) ;
#26228 = CARTESIAN_POINT ( 'NONE',  ( -6.998514795304313196, -276.9805209788415823, -207.2794874003663779 ) ) ;
#26229 = CARTESIAN_POINT ( 'NONE',  ( -71.04305100123842465, -275.6317540362420004, -338.2177641835416466 ) ) ;
#26230 = CARTESIAN_POINT ( 'NONE',  ( 154.3435542972835322, 20.31589174421842614, -11.82430550600266628 ) ) ;
#26231 = CARTESIAN_POINT ( 'NONE',  ( 25.19220096963838529, -280.5390123121077863, -232.4807961771055886 ) ) ;
#26232 = CIRCLE ( 'NONE', #79182, 1.000000000000000888 ) ;
#26233 = CARTESIAN_POINT ( 'NONE',  ( -104.6194925268544296, -279.2807441141486606, -306.9904418572131135 ) ) ;
#26234 = CARTESIAN_POINT ( 'NONE',  ( -70.95236317204168586, -284.6782047952333414, -201.3455868035404137 ) ) ;
#26235 = CARTESIAN_POINT ( 'NONE',  ( 24.17114297115016086, -294.7484841682050387, -229.2011356279915333 ) ) ;
#26236 = CARTESIAN_POINT ( 'NONE',  ( 37.94857302815160693, -277.3048287523072872, -282.4323135914204386 ) ) ;
#26237 = CARTESIAN_POINT ( 'NONE',  ( 0.9341010739579499456, -275.8668556970181953, -204.1019794387270849 ) ) ;
#26238 = CARTESIAN_POINT ( 'NONE',  ( -74.94434090351494149, -282.8906705383787994, 74.50000000000001421 ) ) ;
#26239 = CARTESIAN_POINT ( 'NONE',  ( 35.58709516685505037, -275.3298018247866139, -266.1410867121336423 ) ) ;
#26240 = CARTESIAN_POINT ( 'NONE',  ( -111.0867660119768061, -298.7159470455799806, -257.6452347675588044 ) ) ;
#26241 = CARTESIAN_POINT ( 'NONE',  ( -38.63158897254069046, -284.0358156053305834, -195.5261024270406836 ) ) ;
#26242 = CARTESIAN_POINT ( 'NONE',  ( 34.44464787985057086, -292.8650257537631774, -242.4205436915711687 ) ) ;
#26243 = CARTESIAN_POINT ( 'NONE',  ( 37.50056638392412367, -288.9712979445082510, -256.0406584779146897 ) ) ;
#26244 = AXIS2_PLACEMENT_3D ( 'NONE', #26462, #47751, #89906 ) ;
#26245 = CARTESIAN_POINT ( 'NONE',  ( 34.62521702829261727, -292.6559072008711269, -284.3249609128792486 ) ) ;
#26246 = VERTEX_POINT ( 'NONE', #65831 ) ;
#26247 = CARTESIAN_POINT ( 'NONE',  ( 12.90476180693938879, -291.3124891340683575, -212.7946402857659223 ) ) ;
#26248 = CARTESIAN_POINT ( 'NONE',  ( 23.36118198553759839, -292.6553995129997929, -229.7748199266951588 ) ) ;
#26249 = VERTEX_POINT ( 'NONE', #70694 ) ;
#26250 = CARTESIAN_POINT ( 'NONE',  ( 38.37206299093478634, -288.7891116113618182, -282.8875521945520859 ) ) ;
#26251 = CARTESIAN_POINT ( 'NONE',  ( -76.83686048527216883, -279.8408640855582803, -208.8824401048894686 ) ) ;
#26252 = CARTESIAN_POINT ( 'NONE',  ( -56.00840384629794499, -294.2074439675961912, -344.7455698604939016 ) ) ;
#26253 = CARTESIAN_POINT ( 'NONE',  ( -60.48715447031707981, -286.4111992367593302, -196.9734871406977277 ) ) ;
#26254 = CARTESIAN_POINT ( 'NONE',  ( -35.15309205289024419, -286.4121743407843041, -193.4002407481139301 ) ) ;
#26255 = CARTESIAN_POINT ( 'NONE',  ( -42.93030043953837094, -283.4577701810317194, -343.2181901583103354 ) ) ;
#26256 = CARTESIAN_POINT ( 'NONE',  ( 203.1404359220460094, 295.9636561932003929, -68.66402283083226621 ) ) ;
#26257 = CARTESIAN_POINT ( 'NONE',  ( -85.03340929734007148, -218.4748483833227510, -351.2754620631345119 ) ) ;
#26258 = CARTESIAN_POINT ( 'NONE',  ( 120.5147935217607369, 148.1047250371406108, -260.3425545554943028 ) ) ;
#26259 = CARTESIAN_POINT ( 'NONE',  ( 31.27329421153728006, -274.4115196545928370, -244.9724536127689589 ) ) ;
#26260 = CARTESIAN_POINT ( 'NONE',  ( -39.17923399095218429, -275.9960779647041704, -343.6471981327445633 ) ) ;
#26261 = CARTESIAN_POINT ( 'NONE',  ( -113.5925088572683421, -295.9264570160129892, -281.0151233285136527 ) ) ;
#26262 = CARTESIAN_POINT ( 'NONE',  ( -110.3569200167271731, -272.2263580403405285, -270.3569698429222399 ) ) ;
#26263 = CARTESIAN_POINT ( 'NONE',  ( 21.34152340402464887, -274.9018619669350869, -319.4485659730281100 ) ) ;
#26264 = CARTESIAN_POINT ( 'NONE',  ( -95.42165565302137509, -274.9507823595713489, -224.4841871472521291 ) ) ;
#26265 = ORIENTED_EDGE ( 'NONE', *, *, #20409, .F. ) ;
#26266 = CARTESIAN_POINT ( 'NONE',  ( -36.91058164494567961, -298.9986726998774884, -193.5963432578485310 ) ) ;
#26267 = CARTESIAN_POINT ( 'NONE',  ( 31.89691442077901584, -287.7349170331864343, -247.0372525869651383 ) ) ;
#26268 = CARTESIAN_POINT ( 'NONE',  ( -44.76981581364312035, -295.9465974294657826, -346.8930492274545827 ) ) ;
#26269 = CARTESIAN_POINT ( 'NONE',  ( -93.62202212357776432, -297.7608938521111099, -217.8233932158630637 ) ) ;
#26270 = CARTESIAN_POINT ( 'NONE',  ( 18.83445677758343351, -294.3800209773427241, -316.9791338116584143 ) ) ;
#26271 = ORIENTED_EDGE ( 'NONE', *, *, #78636, .F. ) ;
#26272 = CARTESIAN_POINT ( 'NONE',  ( 13.92446225311632446, -278.2602636349503769, -325.9399616888951527 ) ) ;
#26273 = ORIENTED_EDGE ( 'NONE', *, *, #19380, .T. ) ;
#26274 = CARTESIAN_POINT ( 'NONE',  ( 20.08693444838612407, -280.3649296713189187, -219.1409270331742221 ) ) ;
#26275 = VECTOR ( 'NONE', #14079, 1000.000000000000000 ) ;
#26276 = CARTESIAN_POINT ( 'NONE',  ( 21.03170101262399072, -277.1128943885149170, -314.5872922240578191 ) ) ;
#26277 = CARTESIAN_POINT ( 'NONE',  ( -9.561140581058900523, -278.4542155220726727, -341.0874534253259185 ) ) ;
#26278 = CARTESIAN_POINT ( 'NONE',  ( -111.3753964750786167, -276.7527005194771164, -256.2416556145506092 ) ) ;
#26279 = CARTESIAN_POINT ( 'NONE',  ( -60.55611930151117406, -298.3944916406449011, -200.9895843317770243 ) ) ;
#26280 = CARTESIAN_POINT ( 'NONE',  ( -55.96985377278768681, -293.8713545529170688, -341.6063911346960822 ) ) ;
#26281 = CARTESIAN_POINT ( 'NONE',  ( 153.2628468892384888, 20.37991841447901109, -11.93555113919333266 ) ) ;
#26282 = CARTESIAN_POINT ( 'NONE',  ( 23.69465426782590711, -281.4189287664364088, -223.4984796440012360 ) ) ;
#26283 = CARTESIAN_POINT ( 'NONE',  ( -110.2800522210475691, -278.6792653490147700, -273.3605843429757556 ) ) ;
#26284 = AXIS2_PLACEMENT_3D ( 'NONE', #14693, #29360, #35047 ) ;
#26285 = CARTESIAN_POINT ( 'NONE',  ( 33.57885181016307286, -286.6052818202414301, -299.2001241953170734 ) ) ;
#26286 = CARTESIAN_POINT ( 'NONE',  ( -86.73877593368048622, -275.3659278562917052, -213.8568694637461647 ) ) ;
#26287 = LINE ( 'NONE', #68920, #70161 ) ;
#26288 = CIRCLE ( 'NONE', #15757, 2.500000000000008882 ) ;
#26289 = CARTESIAN_POINT ( 'NONE',  ( -84.79752433890394059, -288.9230149066366380, -326.1105451711822525 ) ) ;
#26290 = VECTOR ( 'NONE', #50479, 999.9999999999998863 ) ;
#26291 = CARTESIAN_POINT ( 'NONE',  ( -88.26026055514134327, -283.0916473165418097, -328.0569839667695646 ) ) ;
#26292 = CARTESIAN_POINT ( 'NONE',  ( 35.21975468809848309, -279.9826426000877859, -285.0127886254265945 ) ) ;
#26294 = CARTESIAN_POINT ( 'NONE',  ( -59.39767046211024137, -281.4196310038104230, -341.5127707078032699 ) ) ;
#26293 = CARTESIAN_POINT ( 'NONE',  ( 32.54184616499231453, -279.8213389707801184, -247.1425293020669187 ) ) ;
#26295 = CARTESIAN_POINT ( 'NONE',  ( -55.21721882969501394, -287.8225279027227543, -197.4696047219434547 ) ) ;
#26296 = CARTESIAN_POINT ( 'NONE',  ( -108.6792038926475641, -279.9837929090616626, -253.0958041212535932 ) ) ;
#26297 = CARTESIAN_POINT ( 'NONE',  ( 175.2296996224750103, 275.5000000000000568, 25.00000000000000355 ) ) ;
#26298 = CARTESIAN_POINT ( 'NONE',  ( 20.64628258383619297, -294.8965061006154542, -222.7964828649481603 ) ) ;
#26300 = CARTESIAN_POINT ( 'NONE',  ( -68.61902918569309406, -275.6974156703191738, -339.6263475907481961 ) ) ;
#26299 = VECTOR ( 'NONE', #76744, 1000.000000000000000 ) ;
#26301 = CARTESIAN_POINT ( 'NONE',  ( 32.99820258467713785, -276.4668849976455931, -290.3114866442770108 ) ) ;
#26302 = CARTESIAN_POINT ( 'NONE',  ( -110.0939359457274520, -286.3094202302920053, -289.3102426970918941 ) ) ;
#26303 = CARTESIAN_POINT ( 'NONE',  ( 198.0025355114448757, 65.94618789579841689, 9.918135210125075929 ) ) ;
#26304 = CARTESIAN_POINT ( 'NONE',  ( -108.5010049489971351, -292.1436745756881237, -295.9260817014101121 ) ) ;
#26305 = CARTESIAN_POINT ( 'NONE',  ( -101.4931958176359359, -294.0302014091283809, -309.3126913038948373 ) ) ;
#26306 = CIRCLE ( 'NONE', #74632, 25.00000000000000355 ) ;
#26307 = DIRECTION ( 'NONE',  ( 0.000000000000000000, 0.000000000000000000, 1.000000000000000000 ) ) ;
#26308 = CARTESIAN_POINT ( 'NONE',  ( 34.86110644327963826, -274.0573143454735714, -256.6498743373807088 ) ) ;
#26309 = CARTESIAN_POINT ( 'NONE',  ( -28.77659480126357749, -293.0821270705926054, -344.1524296968357817 ) ) ;
#26310 = DIRECTION ( 'NONE',  ( -0.000000000000000000, -1.000000000000000000, -0.000000000000000000 ) ) ;
#26311 = DIRECTION ( 'NONE',  ( 0.000000000000000000, 0.000000000000000000, 1.000000000000000000 ) ) ;
#26312 = CARTESIAN_POINT ( 'NONE',  ( -61.45100030471474639, -290.2245802948023083, -197.9076169380507224 ) ) ;
#26313 = CARTESIAN_POINT ( 'NONE',  ( -81.97845966521933292, -287.0321949051790966, -211.5903760177906747 ) ) ;
#26314 = CARTESIAN_POINT ( 'NONE',  ( -79.99064857901045400, -287.8600200346054407, -333.3138133357191464 ) ) ;
#26315 = CARTESIAN_POINT ( 'NONE',  ( -52.22570088316209080, -287.2831139814683752, -198.2928070756119610 ) ) ;
#26316 = DIRECTION ( 'NONE',  ( -0.000000000000000000, 1.000000000000000000, -0.000000000000000000 ) ) ;
#26317 = CARTESIAN_POINT ( 'NONE',  ( -95.90131998200267560, -285.9692173225861893, -226.5048453415226675 ) ) ;
#26318 = CARTESIAN_POINT ( 'NONE',  ( 0.8443782721789957479, -294.5383403931590465, -205.3381969002995788 ) ) ;
#26319 = CARTESIAN_POINT ( 'NONE',  ( 37.07818616452597382, -273.4644007121743812, -257.2105570007907431 ) ) ;
#26320 = CARTESIAN_POINT ( 'NONE',  ( 30.52642916392602856, -276.3563393324366189, -306.8008231461516289 ) ) ;
#26321 = CARTESIAN_POINT ( 'NONE',  ( -28.00236521333965811, -290.2495343561877235, -195.3278414869026278 ) ) ;
#26322 = CARTESIAN_POINT ( 'NONE',  ( -71.23459404651939053, -279.6170165848312195, -201.2216087144612402 ) ) ;
#26323 = CARTESIAN_POINT ( 'NONE',  ( -67.94705255485008877, -297.4357834180092937, -338.4571338914789749 ) ) ;
#26324 = FACE_OUTER_BOUND ( 'NONE', #52478, .T. ) ;
#26325 = DIRECTION ( 'NONE',  ( 1.000000000000000000, 0.000000000000000000, 0.000000000000000000 ) ) ;
#26326 = CARTESIAN_POINT ( 'NONE',  ( -62.71753342243975737, -284.3997853769526500, -201.3335911245622754 ) ) ;
#26327 = CARTESIAN_POINT ( 'NONE',  ( -110.2609925786772749, -276.5103471030346327, -284.3439342227755446 ) ) ;
#26328 = EDGE_CURVE ( 'NONE', #70640, #82273, #34698, .T. ) ;
#26329 = CARTESIAN_POINT ( 'NONE',  ( 37.53077405354408569, -279.6185947847861826, -275.5486191957865003 ) ) ;
#26330 = EDGE_CURVE ( 'NONE', #79924, #68047, #8485, .T. ) ;
#26331 = LINE ( 'NONE', #19686, #1410 ) ;
#26332 = CARTESIAN_POINT ( 'NONE',  ( 22.22934109539131597, -273.3872836693557815, -222.6539268636627469 ) ) ;
#26333 = CARTESIAN_POINT ( 'NONE',  ( -110.0062987976195075, -277.7896554108201599, -278.7933480222311573 ) ) ;
#26334 = CARTESIAN_POINT ( 'NONE',  ( 14.82059547345917316, -295.8212091062537183, -322.4886528285321106 ) ) ;
#26335 = CARTESIAN_POINT ( 'NONE',  ( -39.56446820536647380, -278.9452208197390632, -193.6894486889392226 ) ) ;
#26336 = CARTESIAN_POINT ( 'NONE',  ( -96.59173980530474068, -296.8926654562826002, -313.4271606224881452 ) ) ;
#26337 = CARTESIAN_POINT ( 'NONE',  ( -84.92288838259740658, -298.7263989168827152, -210.4501106825119336 ) ) ;
#26338 = CARTESIAN_POINT ( 'NONE',  ( -52.63301758662038310, -297.6842090015859412, -198.9287340268444950 ) ) ;
#26339 = CARTESIAN_POINT ( 'NONE',  ( -44.51620921233904227, -293.9616707821442105, -195.6528484282623310 ) ) ;
#26340 = CARTESIAN_POINT ( 'NONE',  ( -15.41548952005958206, -286.4948914133883591, -196.4935233328399136 ) ) ;
#26341 = CARTESIAN_POINT ( 'NONE',  ( 36.43760177122948107, -273.4720743667242004, -253.0732350519316469 ) ) ;
#26342 = CARTESIAN_POINT ( 'NONE',  ( 5.555563528388226757, -288.3217801799153790, -334.3050369684871725 ) ) ;
#26343 = CARTESIAN_POINT ( 'NONE',  ( -65.45853539776376806, -281.6626226006118827, -201.2142425780098165 ) ) ;
#26344 = CARTESIAN_POINT ( 'NONE',  ( -0.8846859871772232431, -287.6144534260129717, -333.9355825978587973 ) ) ;
#26345 = CARTESIAN_POINT ( 'NONE',  ( -95.88598520365640354, -289.1967194205273586, -223.4828998136632663 ) ) ;
#26346 = VERTEX_POINT ( 'NONE', #5824 ) ;
#26347 = CARTESIAN_POINT ( 'NONE',  ( -75.88346903603265048, -208.4961600436150491, -353.2410745688453062 ) ) ;
#26348 = VECTOR ( 'NONE', #42354, 1000.000000000000000 ) ;
#26349 = CARTESIAN_POINT ( 'NONE',  ( -71.20684811354948351, -289.0195022834400902, -335.1142689583439847 ) ) ;
#26350 = DIRECTION ( 'NONE',  ( -0.000000000000000000, -0.000000000000000000, -1.000000000000000000 ) ) ;
#26351 = CARTESIAN_POINT ( 'NONE',  ( -47.21419329412872656, -284.1159239877375740, -346.4883410451242867 ) ) ;
#26352 = CARTESIAN_POINT ( 'NONE',  ( -90.61399526793843506, -290.3784373443359073, -215.0163613484924952 ) ) ;
#26353 = CARTESIAN_POINT ( 'NONE',  ( 30.00512399797122498, -282.6858058148495161, -234.5997591034260665 ) ) ;
#26354 = CARTESIAN_POINT ( 'NONE',  ( 21.58012721499826370, -282.2070399355927748, -221.5603337975484237 ) ) ;
#26355 = CARTESIAN_POINT ( 'NONE',  ( 31.97727590711572887, -281.0797282946595033, -247.3133679471492599 ) ) ;
#26356 = CARTESIAN_POINT ( 'NONE',  ( -4.453409786974630968, -276.4856637636619894, -202.9424595835075138 ) ) ;
#26357 = CARTESIAN_POINT ( 'NONE',  ( -86.39531758579973086, -295.7118411637598001, -329.7138147562689028 ) ) ;
#26358 = CIRCLE ( 'NONE', #5221, 21.95310499597075804 ) ;
#26359 = CARTESIAN_POINT ( 'NONE',  ( -108.9665960450441133, -288.8447249982889389, -249.2986243628762395 ) ) ;
#26360 = CARTESIAN_POINT ( 'NONE',  ( -110.7387727487133446, -271.3472703583528869, -270.3458102218887120 ) ) ;
#26361 = VERTEX_POINT ( 'NONE', #12451 ) ;
#26362 = ORIENTED_EDGE ( 'NONE', *, *, #67205, .F. ) ;
#26363 = CARTESIAN_POINT ( 'NONE',  ( -89.89389982017860348, -285.7208645413335262, -323.1551704498491517 ) ) ;
#26364 = AXIS2_PLACEMENT_3D ( 'NONE', #72331, #65247, #34940 ) ;
#26365 = CARTESIAN_POINT ( 'NONE',  ( -68.08957639106087356, -296.5262102990658946, -340.6182216507805833 ) ) ;
#26366 = TOROIDAL_SURFACE ( 'NONE', #85299, 8.222204860432958284, 1.000000000000000000 ) ;
#26367 = CARTESIAN_POINT ( 'NONE',  ( 11.99158077817589607, -282.9956912279861285, -324.3066466475954144 ) ) ;
#26368 = CARTESIAN_POINT ( 'NONE',  ( 35.83470535471820284, -274.9033446749280074, -293.5566756073033616 ) ) ;
#26369 = CARTESIAN_POINT ( 'NONE',  ( -96.50576685131620991, -291.8651355981500046, -221.2192231310186799 ) ) ;
#26370 = CARTESIAN_POINT ( 'NONE',  ( -75.46437946928794815, -283.6893944842710766, -204.8257800826843891 ) ) ;
#26371 = CARTESIAN_POINT ( 'NONE',  ( 6.480709740987499856, -292.9632695087938714, -207.0733570431969497 ) ) ;
#26372 = CARTESIAN_POINT ( 'NONE',  ( -53.40905182814710628, -289.5972684268609214, -341.5926257303513580 ) ) ;
#26373 = FACE_OUTER_BOUND ( 'NONE', #87456, .T. ) ;
#26374 = AXIS2_PLACEMENT_3D ( 'NONE', #11384, #55885, #77662 ) ;
#26375 = DIRECTION ( 'NONE',  ( 0.4878460013594548283, 0.3579938043661797242, -0.7961449082880704964 ) ) ;
#26376 = CARTESIAN_POINT ( 'NONE',  ( 201.4066894621335280, 289.8166775212674224, -82.35935531522035546 ) ) ;
#26377 = CARTESIAN_POINT ( 'NONE',  ( -55.51810208605158437, -284.8020765033892303, -344.4713477943891462 ) ) ;
#26378 = CARTESIAN_POINT ( 'NONE',  ( 35.78497577281001440, -278.8380690714489560, -253.7030783399848985 ) ) ;
#26379 = ORIENTED_EDGE ( 'NONE', *, *, #23961, .T. ) ;
#26380 = CARTESIAN_POINT ( 'NONE',  ( 34.06459102718468301, -280.2544932693967894, -253.7669124225878647 ) ) ;
#26381 = CARTESIAN_POINT ( 'NONE',  ( -6.587047800884924698, -276.3259785197055862, -340.9437455100886041 ) ) ;
#26382 = CARTESIAN_POINT ( 'NONE',  ( -8.565318823985945684, -282.4298136066522602, -201.2818279806009230 ) ) ;
#26383 = CARTESIAN_POINT ( 'NONE',  ( 7.652886109949530002, -59.88684688645761156, -352.9270608465728856 ) ) ;
#26384 = CARTESIAN_POINT ( 'NONE',  ( -3.898980447687987461, -279.0593657860032408, -201.6430641607024938 ) ) ;
#26385 = CARTESIAN_POINT ( 'NONE',  ( -97.89467229529081749, -283.1694792728249013, -226.6909045270137995 ) ) ;
#26386 = CARTESIAN_POINT ( 'NONE',  ( -43.23384418626412184, -299.7389936128457180, -194.5507258692761354 ) ) ;
#26387 = CONICAL_SURFACE ( 'NONE', #73233, 9.550761578869391144, 0.7853981633974327359 ) ;
#26388 = CARTESIAN_POINT ( 'NONE',  ( 34.12908445250047151, -294.2451482167011250, -285.5841125330833847 ) ) ;
#26389 = ORIENTED_EDGE ( 'NONE', *, *, #30098, .F. ) ;
#26390 = CARTESIAN_POINT ( 'NONE',  ( -106.1666134912603070, -289.5802534498914156, -244.4413347145414264 ) ) ;
#26391 = CARTESIAN_POINT ( 'NONE',  ( 29.01218391079727255, -276.7101048117015125, -309.2259460319469895 ) ) ;
#26392 = CARTESIAN_POINT ( 'NONE',  ( 20.68153027937933430, -274.9289478228903363, -226.0426334068589540 ) ) ;
#26393 = CARTESIAN_POINT ( 'NONE',  ( 36.93591799251217367, -274.7123195487147314, -289.4484948865908791 ) ) ;
#26394 = DIRECTION ( 'NONE',  ( 0.000000000000000000, 0.000000000000000000, 1.000000000000000000 ) ) ;
#26395 = CARTESIAN_POINT ( 'NONE',  ( -109.9060790237128344, -270.7979523233628925, -251.2056178072172941 ) ) ;
#26396 = DIRECTION ( 'NONE',  ( -0.000000000000000000, -0.000000000000000000, -1.000000000000000000 ) ) ;
#26397 = CARTESIAN_POINT ( 'NONE',  ( -43.40350038011558809, -262.7128720674827491, -501.1256881030387262 ) ) ;
#26398 = CARTESIAN_POINT ( 'NONE',  ( 18.73967121504439604, -283.2998504914871774, -317.5940168848536018 ) ) ;
#26399 = CARTESIAN_POINT ( 'NONE',  ( 34.65625571128948224, -283.6242464919540112, -294.8202209381691432 ) ) ;
#26400 = CARTESIAN_POINT ( 'NONE',  ( -110.1980361825345653, -283.8218637189545461, -276.3483514582993621 ) ) ;
#26401 = CARTESIAN_POINT ( 'NONE',  ( 25.97253327641737997, -273.4349648419598680, -232.3444398746385389 ) ) ;
#26402 = CARTESIAN_POINT ( 'NONE',  ( 17.96755236496446173, -282.7158978469478257, -220.8459478810472660 ) ) ;
#26403 = CARTESIAN_POINT ( 'NONE',  ( 27.36637378483180782, -274.5101507844141224, -305.7320739244359515 ) ) ;
#26404 = CARTESIAN_POINT ( 'NONE',  ( 154.6618539303304658, 20.39582633401224498, 12.36945559417337215 ) ) ;
#26405 = CARTESIAN_POINT ( 'NONE',  ( 11.74333479298099014, -275.8322769167834281, -215.8420162428405717 ) ) ;
#26406 = CARTESIAN_POINT ( 'NONE',  ( -83.63170945779077670, -296.0521521680024080, -413.1172536214571096 ) ) ;
#26407 = CARTESIAN_POINT ( 'NONE',  ( -73.69828186844009110, -280.3849564428605277, -202.6530829540375009 ) ) ;
#26408 = ORIENTED_EDGE ( 'NONE', *, *, #23274, .F. ) ;
#26409 = FACE_OUTER_BOUND ( 'NONE', #3280, .T. ) ;
#26410 = CARTESIAN_POINT ( 'NONE',  ( -73.05211475263534737, -287.4448424621183449, -203.4818108167443427 ) ) ;
#26411 = CARTESIAN_POINT ( 'NONE',  ( -63.63655701532286457, -294.6009067051807619, -338.6876494883055102 ) ) ;
#26412 = CARTESIAN_POINT ( 'NONE',  ( -113.7133381119638074, -289.7827442907640147, -279.7835390527013715 ) ) ;
#26413 = CARTESIAN_POINT ( 'NONE',  ( 36.28469113919991429, -285.6936628434098111, -262.8027768066472163 ) ) ;
#26415 = CARTESIAN_POINT ( 'NONE',  ( -109.6965320845570346, -288.9947285975260911, -254.7806074367004499 ) ) ;
#26414 = CARTESIAN_POINT ( 'NONE',  ( 33.60210927526537006, -285.8705693364300942, -250.8073248591778395 ) ) ;
#26416 = CARTESIAN_POINT ( 'NONE',  ( -106.5429952969378036, -285.4316695667433805, -294.9727740246291319 ) ) ;
#26417 = CARTESIAN_POINT ( 'NONE',  ( -17.90150196408593430, -274.8013122873251177, -342.7978444491726577 ) ) ;
#26418 = CARTESIAN_POINT ( 'NONE',  ( -49.19991959951759952, -284.3034606604090868, -195.0362803112939787 ) ) ;
#26419 = CARTESIAN_POINT ( 'NONE',  ( -99.89601474075350040, -299.1113143508848111, -228.9619021200954876 ) ) ;
#26420 = CARTESIAN_POINT ( 'NONE',  ( 10.92043478843026172, -284.7174067739193219, -212.6668424218146924 ) ) ;
#26421 = CARTESIAN_POINT ( 'NONE',  ( 19.00949645153776046, -281.8319373625953403, -223.5661195490816908 ) ) ;
#26422 = CARTESIAN_POINT ( 'NONE',  ( -59.46284473111802527, -291.3381026873716451, -342.1990145676941779 ) ) ;
#26423 = DIRECTION ( 'NONE',  ( -0.000000000000000000, 1.000000000000000000, -0.000000000000000000 ) ) ;
#26424 = PLANE ( 'NONE',  #47330 ) ;
#26425 = CARTESIAN_POINT ( 'NONE',  ( -22.35871999816993494, -296.7818865975477252, -344.4207189917935921 ) ) ;
#26426 = CARTESIAN_POINT ( 'NONE',  ( -109.1344211384381566, -276.8316147073302886, -248.6630567903306144 ) ) ;
#26427 = CARTESIAN_POINT ( 'NONE',  ( -0.8714687899061585030, -291.7210559669639451, -202.7291651278841300 ) ) ;
#26428 = CARTESIAN_POINT ( 'NONE',  ( -109.3771439809073627, -294.7427000464688263, -286.4027901715789994 ) ) ;
#26429 = CARTESIAN_POINT ( 'NONE',  ( 10.21514642313670329, -281.0652302525782602, -326.4600721717990837 ) ) ;
#26430 = CARTESIAN_POINT ( 'NONE',  ( 22.65603105917831073, -273.0266130720748379, -226.2976812982627735 ) ) ;
#26431 = CARTESIAN_POINT ( 'NONE',  ( 34.69657940652931671, -294.6766661292332401, -255.8101812088421241 ) ) ;
#26432 = CARTESIAN_POINT ( 'NONE',  ( -37.30987171927208124, -297.5519495502701943, -345.3611179825600175 ) ) ;
#26433 = CARTESIAN_POINT ( 'NONE',  ( -113.6731869624870939, -295.0059029413213239, -272.4314892816096858 ) ) ;
#26435 = CARTESIAN_POINT ( 'NONE',  ( 22.36139224206100096, -292.4292534763379763, -317.3874628399476592 ) ) ;
#26434 =( BOUNDED_SURFACE ( )  B_SPLINE_SURFACE ( 3, 2, ( 
 ( #67300, #45957, #46876 ),
 ( #2428, #32228, #81935 ),
 ( #54001, #2880, #45015 ),
 ( #31765, #17089, #82870 ),
 ( #46417, #16163, #89494 ),
 ( #81019, #31308, #18023 ) ),
 .UNSPECIFIED., .F., .F., .F. ) 
 B_SPLINE_SURFACE_WITH_KNOTS ( ( 4, 2, 4 ),
 ( 3, 3 ),
 ( -2.088173384207081540E-16, 0.001011815784625562549, 0.002023631569251334132 ),
 ( 0.000000000000000000, 1.000000000000000000 ),
 .UNSPECIFIED. ) 
 GEOMETRIC_REPRESENTATION_ITEM ( )  RATIONAL_B_SPLINE_SURFACE ( (
 ( 1.000000000000000000, 0.6287211027133666752, 1.000000000000000000),
 ( 1.000000000000000000, 0.5832186976974050863, 1.000000000000000000),
 ( 1.000000000000000000, 0.5529292259169074075, 1.000000000000000000),
 ( 1.000000000000000000, 0.5121682666463089895, 1.000000000000000000),
 ( 1.000000000000000000, 0.5021481801630829356, 1.000000000000000000),
 ( 1.000000000000000000, 0.5021841165015863417, 1.000000000000000000) ) ) 
 REPRESENTATION_ITEM ( '' )  SURFACE ( )  );
#26436 = CARTESIAN_POINT ( 'NONE',  ( -100.8029659881560889, -291.4687410338707423, -307.7178867496866701 ) ) ;
#26437 = ADVANCED_FACE ( 'NONE', ( #58698 ), #77317, .F. ) ;
#26438 = DIRECTION ( 'NONE',  ( 1.000000000000000000, 0.000000000000000000, 0.000000000000000000 ) ) ;
#26439 = CARTESIAN_POINT ( 'NONE',  ( -103.7070790576606214, -291.7697287510218302, -239.5676413039495571 ) ) ;
#26440 = DIRECTION ( 'NONE',  ( 0.000000000000000000, 0.000000000000000000, -1.000000000000000000 ) ) ;
#26442 = CARTESIAN_POINT ( 'NONE',  ( 26.23455502610557843, -293.0598504924863619, -234.3822895747496773 ) ) ;
#26441 = CARTESIAN_POINT ( 'NONE',  ( 3.629792614694514086, -280.5244457648807384, -333.6663039421703729 ) ) ;
#26443 = CARTESIAN_POINT ( 'NONE',  ( 8.546538727886705544, -280.6610364103018469, -208.4622460652895484 ) ) ;
#26444 = CARTESIAN_POINT ( 'NONE',  ( -70.46486825586555369, -283.1435913071669574, -339.8637045638298559 ) ) ;
#26445 = CARTESIAN_POINT ( 'NONE',  ( -56.56040196355512251, -287.3001343400755445, -342.7383702791111091 ) ) ;
#26446 = CARTESIAN_POINT ( 'NONE',  ( -108.1713766829209789, -282.4020454386303527, -292.5877326523000193 ) ) ;
#26447 = ADVANCED_FACE ( 'NONE', ( #15595 ), #70094, .T. ) ;
#26448 = CARTESIAN_POINT ( 'NONE',  ( -67.07429098632485420, -278.1492807548430619, -200.0853697151221695 ) ) ;
#26449 = AXIS2_PLACEMENT_3D ( 'NONE', #73417, #30315, #88051 ) ;
#26450 = CARTESIAN_POINT ( 'NONE',  ( 36.39783940363580683, -286.2051470655875960, -249.1017686944038587 ) ) ;
#26451 = CARTESIAN_POINT ( 'NONE',  ( 195.2805408448962510, 40.11065606325327337, 14.93368823901625930 ) ) ;
#26452 = CARTESIAN_POINT ( 'NONE',  ( 36.44263436832511616, -295.1932846108848025, -273.5029255886173587 ) ) ;
#26453 = CARTESIAN_POINT ( 'NONE',  ( -37.11038484630563516, -278.4745399033110402, -346.7845003415363294 ) ) ;
#26454 = CARTESIAN_POINT ( 'NONE',  ( -109.9866872626672887, -278.3228762974750907, -262.4745185282186526 ) ) ;
#26455 = CARTESIAN_POINT ( 'NONE',  ( -99.20585895683687738, -291.3285398980592049, -224.4933552157917234 ) ) ;
#26456 = CARTESIAN_POINT ( 'NONE',  ( -94.26629997111695047, -281.9472363966891635, -320.0491862950931932 ) ) ;
#26457 = CARTESIAN_POINT ( 'NONE',  ( 13.07378857589137766, -291.8365520526449473, -217.2415646481958049 ) ) ;
#26458 = CARTESIAN_POINT ( 'NONE',  ( -110.9214670853182980, -294.7393583532002026, -255.7687070272976939 ) ) ;
#26459 = VERTEX_POINT ( 'NONE', #89399 ) ;
#26460 = CARTESIAN_POINT ( 'NONE',  ( 197.5319251031163219, 24.91057433061638093, 12.19320131867666746 ) ) ;
#26461 = CARTESIAN_POINT ( 'NONE',  ( -6.744843068460973257, -294.1469356056429092, -336.7073370152170924 ) ) ;
#26462 = CARTESIAN_POINT ( 'NONE',  ( 17.06571399127465583, -89.54582641780471874, 22.50000000000000000 ) ) ;
#26463 = CARTESIAN_POINT ( 'NONE',  ( 7.450504543161054372, -284.1952119285919025, -214.2458315076590907 ) ) ;
#26464 = CARTESIAN_POINT ( 'NONE',  ( -73.16013433214311590, -296.6482473316476671, -202.4065082351918647 ) ) ;
#26465 = CARTESIAN_POINT ( 'NONE',  ( 35.00342103530817184, -279.4044136373784113, -247.8558091756340218 ) ) ;
#26466 = CARTESIAN_POINT ( 'NONE',  ( -60.37749554774559613, -287.0748531455805619, -197.3493967724697313 ) ) ;
#26467 = CARTESIAN_POINT ( 'NONE',  ( -71.17464494521304630, -289.3451167832467945, -335.0616523255988568 ) ) ;
#26468 = CARTESIAN_POINT ( 'NONE',  ( -110.5909649590966382, -279.9608405907517295, -278.8890940655768986 ) ) ;
#26469 = CARTESIAN_POINT ( 'NONE',  ( -97.75412229689837318, -293.9719932934322628, -314.2256865053174693 ) ) ;
#26470 = CARTESIAN_POINT ( 'NONE',  ( -101.0271346666929162, -297.7999964378646496, -308.1732457859682199 ) ) ;
#26471 = CARTESIAN_POINT ( 'NONE',  ( -110.3594849809585696, -277.4512222227780853, -262.4229063633192709 ) ) ;
#26472 = ORIENTED_EDGE ( 'NONE', *, *, #48886, .T. ) ;
#26473 = CARTESIAN_POINT ( 'NONE',  ( 19.37362162970248747, -298.4107710989599127, -193.3853472190476737 ) ) ;
#26474 = CARTESIAN_POINT ( 'NONE',  ( -111.1308226261956236, -292.6043353087607102, -260.1554553659917133 ) ) ;
#26475 = CARTESIAN_POINT ( 'NONE',  ( 30.20273208727713055, -295.6121107140541540, -305.6341968131068256 ) ) ;
#26476 = CARTESIAN_POINT ( 'NONE',  ( -113.9037752538512365, -273.8091386319557046, -270.3771224311939818 ) ) ;
#26477 = CARTESIAN_POINT ( 'NONE',  ( 12.23100940161551087, -288.9919839168108524, -324.1555013309709352 ) ) ;
#26478 = CARTESIAN_POINT ( 'NONE',  ( -48.18343439339133027, -253.2159931059258042, -461.7098312862245280 ) ) ;
#26479 = CARTESIAN_POINT ( 'NONE',  ( -93.59385938653188930, -297.9199342052745578, -217.8524608410955352 ) ) ;
#26480 = CARTESIAN_POINT ( 'NONE',  ( -96.48426051456434038, -289.3364413222395797, -223.0064662996730931 ) ) ;
#26481 = CARTESIAN_POINT ( 'NONE',  ( -37.25787227667515111, -298.3864558371908515, -193.3814936317900504 ) ) ;
#26482 = CARTESIAN_POINT ( 'NONE',  ( 184.7149167944524493, 8.542400036368780647, -9.000000000000001776 ) ) ;
#26483 = B_SPLINE_CURVE_WITH_KNOTS ( 'NONE', 3,
 ( #47844, #76283, #5266, #11409 ),
 .UNSPECIFIED., .F., .F.,
 ( 4, 4 ),
 ( 0.000000000000000000, 0.001237645497661998958 ),
 .UNSPECIFIED. ) ;
#26484 = FACE_OUTER_BOUND ( 'NONE', #90988, .T. ) ;
#26485 = CARTESIAN_POINT ( 'NONE',  ( -71.57788828196257214, -291.0163332232990001, -338.5563610408362933 ) ) ;
#26486 = CARTESIAN_POINT ( 'NONE',  ( 36.60358173371528068, -284.4805209788416391, -305.9350535429201159 ) ) ;
#26487 = CARTESIAN_POINT ( 'NONE',  ( -4.979328192849334478, -279.8157544748613645, -200.6044719207231992 ) ) ;
#26488 = CARTESIAN_POINT ( 'NONE',  ( -94.67573691093001287, -287.2184767517394448, -222.2691575733643390 ) ) ;
#26489 = CARTESIAN_POINT ( 'NONE',  ( 37.71483743257300603, -285.9463863177180656, -256.0390209431961352 ) ) ;
#26490 = CARTESIAN_POINT ( 'NONE',  ( 35.62697380994278262, -273.3376967091575125, -253.7025017441659145 ) ) ;
#26491 = CARTESIAN_POINT ( 'NONE',  ( -68.91516944485796614, -275.5539532124696507, -202.9347589601644302 ) ) ;
#26492 = CARTESIAN_POINT ( 'NONE',  ( -109.1207670723014900, -288.3741955690873056, -290.2764115782188128 ) ) ;
#26493 = CARTESIAN_POINT ( 'NONE',  ( -90.44610022641995783, -279.6543113907909515, -324.4736994991283723 ) ) ;
#26494 = VERTEX_POINT ( 'NONE', #16070 ) ;
#26496 = CARTESIAN_POINT ( 'NONE',  ( 35.78954898484706604, -280.8773950475191441, -268.5893716310541777 ) ) ;
#26495 = CARTESIAN_POINT ( 'NONE',  ( 22.11349279239495047, -280.9604616252137248, -228.0045360289964833 ) ) ;
#26497 = CARTESIAN_POINT ( 'NONE',  ( 36.94277344190060575, -276.8713131571805661, -289.4217973297370463 ) ) ;
#26498 = CARTESIAN_POINT ( 'NONE',  ( 21.67465908354142101, -279.6871979201942509, -221.5238569468187961 ) ) ;
#26499 = CARTESIAN_POINT ( 'NONE',  ( -32.16148137795721595, -124.0225950033424880, -361.1636328524395481 ) ) ;
#26500 = CARTESIAN_POINT ( 'NONE',  ( 39.14707202085495652, -276.5749793860932186, -276.8640363753513611 ) ) ;
#26501 = CARTESIAN_POINT ( 'NONE',  ( -23.51092029594954269, -299.6473766074118998, -193.9470657638637192 ) ) ;
#26502 = CARTESIAN_POINT ( 'NONE',  ( 21.31550574532285580, -290.6948066931273615, -317.0979686699210447 ) ) ;
#26503 = VERTEX_POINT ( 'NONE', #44924 ) ;
#26504 = CARTESIAN_POINT ( 'NONE',  ( 200.2296996224750103, 68.12454877777268791, 4.413917820073312015 ) ) ;
#26505 = CARTESIAN_POINT ( 'NONE',  ( 32.61271130941165097, -288.9231535424723916, -292.4529101380038583 ) ) ;
#26506 = CARTESIAN_POINT ( 'NONE',  ( 21.63305556083389902, -289.9638667322107040, -318.2976992908221519 ) ) ;
#26507 = CARTESIAN_POINT ( 'NONE',  ( -108.7640941326033328, -289.6947882137466763, -285.9992733807759464 ) ) ;
#26508 = CARTESIAN_POINT ( 'NONE',  ( -107.5840519861814073, -285.7688144943634256, -249.4626722518927409 ) ) ;
#26509 = CARTESIAN_POINT ( 'NONE',  ( -2.245378395762407386, -286.0116838537664421, -201.8790478997052560 ) ) ;
#26510 = CARTESIAN_POINT ( 'NONE',  ( -29.97397971420965490, -124.9943380580637040, -364.2934218382724794 ) ) ;
#26511 = CARTESIAN_POINT ( 'NONE',  ( 20.79876770051471979, -280.5858102905837654, -315.8157813100587532 ) ) ;
#26512 = CARTESIAN_POINT ( 'NONE',  ( 33.84787573538152827, -289.1381919327232595, -249.2709037235404139 ) ) ;
#26513 = CARTESIAN_POINT ( 'NONE',  ( -2.114097185898930586, -281.0567505037315641, -335.1036166233522522 ) ) ;
#26514 = CARTESIAN_POINT ( 'NONE',  ( -109.7692447497787782, -279.7029641874109416, -282.9051393760942688 ) ) ;
#26515 = CARTESIAN_POINT ( 'NONE',  ( 3.173436779058369073, -276.9837799162163492, -331.1600663529284816 ) ) ;
#26516 = CARTESIAN_POINT ( 'NONE',  ( -81.68796297553329566, -290.2579340431400965, -207.8997884333085437 ) ) ;
#26517 = AXIS2_PLACEMENT_3D ( 'NONE', #32087, #39623, #54786 ) ;
#26518 = CARTESIAN_POINT ( 'NONE',  ( -110.9503421328437156, -285.0772499776066979, -292.4505304951155154 ) ) ;
#26519 = CARTESIAN_POINT ( 'NONE',  ( -110.8690832948050797, -285.3312678423222906, -247.5267119884094029 ) ) ;
#26520 = CARTESIAN_POINT ( 'NONE',  ( 35.51973029490412870, -281.6595265698347248, -265.8653465021923807 ) ) ;
#26521 = ORIENTED_EDGE ( 'NONE', *, *, #92612, .F. ) ;
#26522 = LINE ( 'NONE', #61581, #58003 ) ;
#26523 = CARTESIAN_POINT ( 'NONE',  ( -111.7170394036605501, -292.5970046144173011, -255.8499364584392879 ) ) ;
#26524 = CARTESIAN_POINT ( 'NONE',  ( -7.367873120264879283, -291.1218943247145035, -199.9560634122750855 ) ) ;
#26525 = CARTESIAN_POINT ( 'NONE',  ( 35.58723100020613117, -274.6988866956650668, -277.0528630635745344 ) ) ;
#26526 = CARTESIAN_POINT ( 'NONE',  ( -64.23831415584729143, -294.7426565363705322, -342.4019740322032135 ) ) ;
#26527 = CARTESIAN_POINT ( 'NONE',  ( -36.17592627345034373, -290.5468699734470306, -196.6644088236953110 ) ) ;
#26528 = CARTESIAN_POINT ( 'NONE',  ( -70.19373344906404100, -293.7310247842222566, -336.6839490670975579 ) ) ;
#26529 = CARTESIAN_POINT ( 'NONE',  ( -84.93088073728347354, -290.9306001197653586, -326.3066328120752360 ) ) ;
#26530 = CARTESIAN_POINT ( 'NONE',  ( 200.4972393895363041, 64.43555889006553627, -7.250946725472672050 ) ) ;
#26531 = CARTESIAN_POINT ( 'NONE',  ( -88.11823665433593078, -291.7630158053539162, -325.5584366206380196 ) ) ;
#26532 = CARTESIAN_POINT ( 'NONE',  ( 21.68464018457738263, -290.9141717036186492, -223.8010994277454699 ) ) ;
#26533 = CARTESIAN_POINT ( 'NONE',  ( -63.89893834446905174, -297.3984842723367024, -340.5564354515693708 ) ) ;
#26534 = CARTESIAN_POINT ( 'NONE',  ( -46.76699100961059941, -286.8709478556596650, -197.6839273504741641 ) ) ;
#26535 = CARTESIAN_POINT ( 'NONE',  ( 16.27219540724796332, -296.2938587505097985, -323.1189366517678536 ) ) ;
#26536 = CARTESIAN_POINT ( 'NONE',  ( 25.54375624049132298, -276.9741158277753925, -228.8421322068949735 ) ) ;
#26537 = CARTESIAN_POINT ( 'NONE',  ( 24.04023758294295376, -274.9599163340035943, -316.1897819657462492 ) ) ;
#26538 = CARTESIAN_POINT ( 'NONE',  ( -46.10129540644673796, -297.1408961589830824, -194.0235236347846239 ) ) ;
#26539 = CARTESIAN_POINT ( 'NONE',  ( 19.06636603510410666, -274.4640639476404544, -318.2787983033752539 ) ) ;
#26540 = CARTESIAN_POINT ( 'NONE',  ( -86.41550047006222712, -277.4442672832196308, -214.3872283979690962 ) ) ;
#26541 = CARTESIAN_POINT ( 'NONE',  ( -107.5809884703223531, -274.0397678758758389, -248.8896469012588852 ) ) ;
#26542 = CARTESIAN_POINT ( 'NONE',  ( -106.5350642620218196, -297.6445838101986965, -295.5638594249705307 ) ) ;
#26543 = EDGE_CURVE ( 'NONE', #61209, #83756, #82162, .T. ) ;
#26544 = CARTESIAN_POINT ( 'NONE',  ( 133.0872704186301405, -299.5541904835127980, -195.3611179825600175 ) ) ;
#26545 = CARTESIAN_POINT ( 'NONE',  ( -108.9392745071751847, -297.5538113406017828, -255.2546091852232450 ) ) ;
#26546 = DIRECTION ( 'NONE',  ( 0.000000000000000000, 0.000000000000000000, 1.000000000000000000 ) ) ;
#26548 = CARTESIAN_POINT ( 'NONE',  ( -33.81211282506870219, -298.0975490310236182, -197.3611180786018906 ) ) ;
#26547 = CARTESIAN_POINT ( 'NONE',  ( 26.04724258167656714, -286.1196050401511570, -311.2034313418628244 ) ) ;
#26549 = CARTESIAN_POINT ( 'NONE',  ( 14.24688035217459614, -286.7531436488690701, -213.1264980538594784 ) ) ;
#26550 = CARTESIAN_POINT ( 'NONE',  ( -99.85557839221172571, -289.6230742935561011, -315.3031793183994296 ) ) ;
#26551 = CARTESIAN_POINT ( 'NONE',  ( -111.5244497003094040, -298.7012547784190701, -257.1200277484309709 ) ) ;
#26552 = CARTESIAN_POINT ( 'NONE',  ( 35.85563456518634240, -291.7530438902615515, -285.9845753726145858 ) ) ;
#26553 = CARTESIAN_POINT ( 'NONE',  ( 38.50679924301480384, -280.9044393674689104, -282.7381164179409438 ) ) ;
#26554 = CARTESIAN_POINT ( 'NONE',  ( 198.4468466364687060, 42.00370313906616104, 10.58981561310753250 ) ) ;
#26555 = CARTESIAN_POINT ( 'NONE',  ( -103.2055037226382126, -277.0298764946494998, -234.3796325430344041 ) ) ;
#26556 = CARTESIAN_POINT ( 'NONE',  ( -26.41588298435790350, -486.4924983417995463, -507.6442049081570076 ) ) ;
#26557 = CARTESIAN_POINT ( 'NONE',  ( -56.18224285526869011, -288.0950911280332321, -341.3517143386196722 ) ) ;
#26558 = CARTESIAN_POINT ( 'NONE',  ( 140.6539576904058606, 249.5000000000000568, -12.00000000000000000 ) ) ;
#26559 = CARTESIAN_POINT ( 'NONE',  ( -109.6609731769846690, -288.2942020699566683, -290.4254254028564333 ) ) ;
#26560 = CARTESIAN_POINT ( 'NONE',  ( 52.87650880464764214, -300.8000763623448961, -196.5360689618387653 ) ) ;
#26561 = CARTESIAN_POINT ( 'NONE',  ( -5.682957858946411811, -284.0691747476666364, -339.9048476258201390 ) ) ;
#26563 = CARTESIAN_POINT ( 'NONE',  ( 5.592090758289988806, -282.4520845465209504, -329.4008469802894297 ) ) ;
#26562 = CARTESIAN_POINT ( 'NONE',  ( -48.69670390260161241, -295.9284888967570737, -195.8138301115931199 ) ) ;
#26564 = CARTESIAN_POINT ( 'NONE',  ( -68.54883825244230877, -275.0591516243557066, -203.7028078640957744 ) ) ;
#26565 = ADVANCED_FACE ( 'NONE', ( #74762 ), #46779, .F. ) ;
#26566 = CARTESIAN_POINT ( 'NONE',  ( 2.731262588749159725, -282.5894332169731342, -206.9029527851270132 ) ) ;
#26567 = CARTESIAN_POINT ( 'NONE',  ( -99.53548307293127095, -272.0058865167704880, -231.5518480033855440 ) ) ;
#26568 = ORIENTED_EDGE ( 'NONE', *, *, #21510, .F. ) ;
#26569 = DIRECTION ( 'NONE',  ( -0.000000000000000000, -1.000000000000000000, -0.000000000000000000 ) ) ;
#26570 = CARTESIAN_POINT ( 'NONE',  ( -97.92420053106265243, -287.1286239239596512, -226.7318789255200215 ) ) ;
#26571 = CARTESIAN_POINT ( 'NONE',  ( 195.7510731661265595, -142.7221692137691775, -32.50000000000000711 ) ) ;
#26572 = CARTESIAN_POINT ( 'NONE',  ( -72.08107566293803359, -274.9809262143061233, -342.4248175857292154 ) ) ;
#26573 = CARTESIAN_POINT ( 'NONE',  ( -93.22359948505962279, -277.0270378273148140, -323.1761956177509774 ) ) ;
#26574 = CARTESIAN_POINT ( 'NONE',  ( -69.04326074436966110, -287.8620039541802953, -339.6679004253663265 ) ) ;
#26575 = CARTESIAN_POINT ( 'NONE',  ( -70.50980722328270645, -285.0177218327364699, -336.1824039134395434 ) ) ;
#26576=STYLED_ITEM('',(#93745),#91220);
#26577 = CARTESIAN_POINT ( 'NONE',  ( -5.825046441744500036, -278.3921525149904141, -337.3427927951235574 ) ) ;
#26578 = CARTESIAN_POINT ( 'NONE',  ( -113.6188819958375831, -285.9102025247194092, -275.6948728675853886 ) ) ;
#26579 = CARTESIAN_POINT ( 'NONE',  ( -51.10733440467242161, -282.0268015300047182, -342.5076214538783574 ) ) ;
#26580 = CARTESIAN_POINT ( 'NONE',  ( 29.55406908845921521, -283.1027979530119296, -236.3350273926781995 ) ) ;
#26581 = CARTESIAN_POINT ( 'NONE',  ( -26.99862114891847753, -274.3467363944650970, -194.0055208881272790 ) ) ;
#26582 = CARTESIAN_POINT ( 'NONE',  ( -109.7374885423401309, -278.0524649331115370, -296.7439976247471805 ) ) ;
#26583 = CARTESIAN_POINT ( 'NONE',  ( -108.9821371495358875, -298.2101449321713744, -290.5839264639818680 ) ) ;
#26584 = DIRECTION ( 'NONE',  ( -0.000000000000000000, -0.000000000000000000, -1.000000000000000000 ) ) ;
#26585 = CARTESIAN_POINT ( 'NONE',  ( 156.4870464395701219, 215.0000000000000568, 17.29054515234685141 ) ) ;
#26586 = CARTESIAN_POINT ( 'NONE',  ( -113.1025904759236056, -294.7015227549535439, -269.5910715669770639 ) ) ;
#26587 = CARTESIAN_POINT ( 'NONE',  ( 16.57233386806656128, -275.7667254891260882, -319.6876392050527329 ) ) ;
#26588 = CARTESIAN_POINT ( 'NONE',  ( -95.73501774525767871, -274.4292146643537080, -220.7603842714128746 ) ) ;
#26589 = CARTESIAN_POINT ( 'NONE',  ( 13.82411070878751325, -288.5412276956427604, -216.8111478844424767 ) ) ;
#26590 = CARTESIAN_POINT ( 'NONE',  ( -2.268766472257749189, -296.1165910632869327, -338.1298207832799676 ) ) ;
#26591 = CARTESIAN_POINT ( 'NONE',  ( 6.399918719456080041, -295.6778618717204381, -333.3120023830723540 ) ) ;
#26592 = CARTESIAN_POINT ( 'NONE',  ( -106.4046333997188043, -292.9309371335982064, -241.4105453432695469 ) ) ;
#26593 = CARTESIAN_POINT ( 'NONE',  ( -102.3932453609285744, -277.0462243160820321, -233.3702422569386954 ) ) ;
#26594 = CARTESIAN_POINT ( 'NONE',  ( -54.85483508047848744, -281.7455735179509588, -197.9573212376795084 ) ) ;
#26595 = CARTESIAN_POINT ( 'NONE',  ( -81.01906985839417530, -293.7304093400820761, -330.6404806920920691 ) ) ;
#26596 = CARTESIAN_POINT ( 'NONE',  ( -94.38882485583700088, -285.7271955080646535, -320.2202299134325472 ) ) ;
#26597 = CARTESIAN_POINT ( 'NONE',  ( -93.48299884858347752, -284.1391430164480880, -223.2189855270897851 ) ) ;
#26598 = CARTESIAN_POINT ( 'NONE',  ( -46.16520984643562997, -156.0173353556437803, -364.2845566487454789 ) ) ;
#26599 = EDGE_LOOP ( 'NONE', ( #34419, #83919, #42062, #40906, #93406, #9727 ) ) ;
#26600 = CARTESIAN_POINT ( 'NONE',  ( -52.08905897353218961, -285.5248435149476336, -198.8446660727839230 ) ) ;
#26601 = ORIENTED_EDGE ( 'NONE', *, *, #40288, .F. ) ;
#26602 = CARTESIAN_POINT ( 'NONE',  ( 37.25094498424395084, -282.8561927816836032, -288.2337364978654932 ) ) ;
#26603 = CARTESIAN_POINT ( 'NONE',  ( -51.56973345032491096, -274.1985478715116642, -198.6877339617595339 ) ) ;
#26604 = CARTESIAN_POINT ( 'NONE',  ( -64.39254046066720605, -284.5017778985966288, -198.6793139480549542 ) ) ;
#26605 = CARTESIAN_POINT ( 'NONE',  ( -50.90985073277121842, -280.8240876805172661, -194.8050096821539512 ) ) ;
#26606 = CARTESIAN_POINT ( 'NONE',  ( 194.3571872280090815, 19.99999999999999645, -14.59147969791757582 ) ) ;
#26607 = CARTESIAN_POINT ( 'NONE',  ( -81.85028284571910717, -280.9779593741140502, -208.3797190346592174 ) ) ;
#26608 = CARTESIAN_POINT ( 'NONE',  ( -4.994423991111502481, -281.1183700868226651, -200.5974704747835631 ) ) ;
#26609 = CARTESIAN_POINT ( 'NONE',  ( 30.91033621190086578, -278.8380690714489560, -254.8156830097664738 ) ) ;
#26610 = CARTESIAN_POINT ( 'NONE',  ( 203.1353409855606174, 293.1658297356431717, -83.22860506881615095 ) ) ;
#26611 = ORIENTED_EDGE ( 'NONE', *, *, #22911, .T. ) ;
#26612 = CARTESIAN_POINT ( 'NONE',  ( 10.64158200923520603, -276.7166477349687739, -212.8682576112067864 ) ) ;
#26613 = CARTESIAN_POINT ( 'NONE',  ( 199.2237029682673040, 289.5565456333249585, -97.44563473156274824 ) ) ;
#26614 = CARTESIAN_POINT ( 'NONE',  ( -107.9935472655180035, -276.8871626603749405, -246.1159714119290243 ) ) ;
#26615 = CARTESIAN_POINT ( 'NONE',  ( -35.01420788653632599, -293.8411093123329465, -194.3971249997707389 ) ) ;
#26616 = CARTESIAN_POINT ( 'NONE',  ( -100.2584255176955423, -295.3888303900021697, -307.6814793703455280 ) ) ;
#26617 = CARTESIAN_POINT ( 'NONE',  ( -108.3079553782693267, -290.4381402463579889, -240.6404598667304811 ) ) ;
#26618 = DIRECTION ( 'NONE',  ( 1.000000000000000000, 0.000000000000000000, 0.000000000000000000 ) ) ;
#26620 = CARTESIAN_POINT ( 'NONE',  ( 34.78828026051343159, -286.1564502513272714, -286.0314063445531474 ) ) ;
#26619 = CARTESIAN_POINT ( 'NONE',  ( -90.31674821449534818, -294.3584517662027338, -325.4998569303264162 ) ) ;
#26621 = CARTESIAN_POINT ( 'NONE',  ( 21.51680376796998573, -296.0388320105424782, -315.6206612025129061 ) ) ;
#26622 = CARTESIAN_POINT ( 'NONE',  ( 36.04617335688610780, -286.1742074106616087, -265.5711379855692940 ) ) ;
#26623 = CARTESIAN_POINT ( 'NONE',  ( -110.1028095986347921, -286.0029120330531214, -260.0139238334185166 ) ) ;
#26624 = CARTESIAN_POINT ( 'NONE',  ( -36.39335253043677199, -293.0050168633503063, -193.5892769763656815 ) ) ;
#26625 = CARTESIAN_POINT ( 'NONE',  ( 1.139045458816819067, -283.0159751336047975, -332.5267231827461387 ) ) ;
#26626 = MANIFOLD_SOLID_BREP ( 'Chamfer1', #44620 ) ;
#26627 = CARTESIAN_POINT ( 'NONE',  ( -74.42764890964282642, -294.3286134549203439, -337.4476952199739230 ) ) ;
#26628 = CARTESIAN_POINT ( 'NONE',  ( -98.22659652858438051, -291.9819867019043045, -223.4656495923142643 ) ) ;
#26629 = CARTESIAN_POINT ( 'NONE',  ( -99.81662905474614433, -290.4485692968793842, -315.2881433868143972 ) ) ;
#26630 = CARTESIAN_POINT ( 'NONE',  ( 9.028855969126675873, -286.8762175665992800, -213.9805226352355021 ) ) ;
#26631 = ORIENTED_EDGE ( 'NONE', *, *, #35543, .F. ) ;
#26632 = DIRECTION ( 'NONE',  ( 0.6421047760857910847, 0.000000000000000000, 0.7666168903225496489 ) ) ;
#26633 = CARTESIAN_POINT ( 'NONE',  ( -112.1733633310270619, -298.5642851474183317, -258.4243337670610572 ) ) ;
#26634 = CARTESIAN_POINT ( 'NONE',  ( -40.40363980321603776, -296.6993820149667727, -193.8637701130283233 ) ) ;
#26635 = EDGE_CURVE ( 'NONE', #2170, #52231, #15667, .T. ) ;
#26636 = CARTESIAN_POINT ( 'NONE',  ( 11.47153953092307788, -279.8079787482593588, -215.7655496504346502 ) ) ;
#26637 = ORIENTED_EDGE ( 'NONE', *, *, #38745, .T. ) ;
#26638 = CARTESIAN_POINT ( 'NONE',  ( 39.56160809400698497, -275.1059432973352727, -274.0472738088151345 ) ) ;
#26639 = CARTESIAN_POINT ( 'NONE',  ( -47.34791026978283668, -296.4027107693032690, -197.2985773678334454 ) ) ;
#26640 = CARTESIAN_POINT ( 'NONE',  ( -64.76781208370880449, -279.2744307884012187, -339.3988418925890187 ) ) ;
#26641 = CARTESIAN_POINT ( 'NONE',  ( -3.521145360883818132, -272.6430019281157797, -204.2632959257987864 ) ) ;
#26642 = CARTESIAN_POINT ( 'NONE',  ( -94.24067830949607583, -297.1042624233357401, -316.7450419354605060 ) ) ;
#26643 = CARTESIAN_POINT ( 'NONE',  ( -37.16260514514985402, -299.1341274580777849, -197.0491090442832274 ) ) ;
#26644 = DIRECTION ( 'NONE',  ( -0.8195702660916290849, 0.000000000000000000, -0.5729786897769377774 ) ) ;
#26645 = CARTESIAN_POINT ( 'NONE',  ( -2.316862567297136799, -296.1965845442257432, -338.0346074098131339 ) ) ;
#26646 = CARTESIAN_POINT ( 'NONE',  ( -26.51331991724878634, -296.1872443344852286, -195.1981240880892585 ) ) ;
#26647 = CARTESIAN_POINT ( 'NONE',  ( -64.11665814124751250, -292.3448467768403702, -202.3255520286885769 ) ) ;
#26648 = CARTESIAN_POINT ( 'NONE',  ( -92.99027580637627466, -289.8075467350213330, -222.2091611867411132 ) ) ;
#26649 = CYLINDRICAL_SURFACE ( 'NONE', #72991, 4.000000000000003553 ) ;
#26650 = CARTESIAN_POINT ( 'NONE',  ( 26.09027815450861354, -275.4691217511748960, -226.7957087249940287 ) ) ;
#26651 = CARTESIAN_POINT ( 'NONE',  ( -88.14350127068128415, -297.6506479540262262, -217.8380217683297531 ) ) ;
#26652 = CARTESIAN_POINT ( 'NONE',  ( 30.52883827193004507, -283.1014426512995783, -237.4997932801988156 ) ) ;
#26653 = AXIS2_PLACEMENT_3D ( 'NONE', #92153, #41003, #62364 ) ;
#26654 = CARTESIAN_POINT ( 'NONE',  ( 33.87157781651384880, -279.8785624894327384, -242.2527628918645064 ) ) ;
#26655 = CARTESIAN_POINT ( 'NONE',  ( -51.30226326775083123, -276.5747454194122952, -345.9813233718141987 ) ) ;
#26656 = CARTESIAN_POINT ( 'NONE',  ( -33.49794300959267446, -282.1997323130977406, -343.4341540528075143 ) ) ;
#26657 = CARTESIAN_POINT ( 'NONE',  ( 35.41078938508652385, -279.7942832994010587, -289.2583055848575668 ) ) ;
#26658 = EDGE_CURVE ( 'NONE', #51979, #40097, #12640, .T. ) ;
#26659 = CARTESIAN_POINT ( 'NONE',  ( -29.91247694883873365, -272.7227504864325738, -197.1478571631043621 ) ) ;
#26660 = CARTESIAN_POINT ( 'NONE',  ( -110.5025717868261950, -280.7649202286031596, -253.7968955414481229 ) ) ;
#26661 = CARTESIAN_POINT ( 'NONE',  ( -46.11236658152585477, -296.0521521680024080, -507.6442049081570076 ) ) ;
#26662 = CARTESIAN_POINT ( 'NONE',  ( 2.197429475817664013, -229.5268262511776527, 22.50000000000000000 ) ) ;
#26663 = CARTESIAN_POINT ( 'NONE',  ( -77.64574571157193361, -295.7588089152417297, -205.9440556284513661 ) ) ;
#26664 = CARTESIAN_POINT ( 'NONE',  ( -110.4309002539738032, -290.8589900752696167, -245.9668213614052661 ) ) ;
#26665 = CARTESIAN_POINT ( 'NONE',  ( 31.35481885158082704, -277.9511857978322382, -300.8704067920850775 ) ) ;
#26666 = CARTESIAN_POINT ( 'NONE',  ( 16.91066350521142070, -272.8242979144282572, -218.5009557823775310 ) ) ;
#26667 = CARTESIAN_POINT ( 'NONE',  ( 29.33919985515026596, -285.8906705383787994, 27.50000000000000000 ) ) ;
#26668 = CARTESIAN_POINT ( 'NONE',  ( -102.8053316724463855, -286.9733583429897976, -232.5233784389450307 ) ) ;
#26669 = VERTEX_POINT ( 'NONE', #31668 ) ;
#26670 = CARTESIAN_POINT ( 'NONE',  ( 156.3365481965735455, 16.61859728808169834, -10.14856962220658154 ) ) ;
#26671 = CARTESIAN_POINT ( 'NONE',  ( 28.08357908928204694, -286.0414683489416916, -307.1334348813559245 ) ) ;
#26672 = CARTESIAN_POINT ( 'NONE',  ( 206.9189553108847406, 30.70889394204682432, 14.49999999999999822 ) ) ;
#26673 = CARTESIAN_POINT ( 'NONE',  ( -15.48916135804726935, -293.5579849021808059, -340.4830915405719338 ) ) ;
#26674 = CARTESIAN_POINT ( 'NONE',  ( 14.01083334673153935, -284.9212536848378363, -216.6825002618953135 ) ) ;
#26675 = CARTESIAN_POINT ( 'NONE',  ( 20.69763459394507876, -20.92298310053570987, -343.0354172471594438 ) ) ;
#26676 = CARTESIAN_POINT ( 'NONE',  ( -28.68987852629980395, -292.9424050472306931, -344.9128340944349702 ) ) ;
#26677 = CARTESIAN_POINT ( 'NONE',  ( -5.049601808426840144, -284.9494797728412436, -201.2240935930309718 ) ) ;
#26678 = CARTESIAN_POINT ( 'NONE',  ( -109.6753821937728333, -280.3441219744390764, -255.6593066754535073 ) ) ;
#26679 = CARTESIAN_POINT ( 'NONE',  ( 37.63169741978722271, -288.5588532396723167, -254.5814832043031402 ) ) ;
#26680 = CARTESIAN_POINT ( 'NONE',  ( 35.63291226925915822, -279.5223145476238074, -249.1323558094555608 ) ) ;
#26681 = CARTESIAN_POINT ( 'NONE',  ( -58.68913036541010086, -289.3359118507994481, -340.2228556556863737 ) ) ;
#26682 = CARTESIAN_POINT ( 'NONE',  ( -79.40642690274627569, -280.8968608245478435, -209.9795506195519010 ) ) ;
#26683 = CARTESIAN_POINT ( 'NONE',  ( -57.16676531630589864, -280.5925665085519540, -199.9369139275347891 ) ) ;
#26684 = EDGE_CURVE ( 'NONE', #76858, #4814, #24473, .T. ) ;
#26685 = CARTESIAN_POINT ( 'NONE',  ( -80.02770050428505044, -287.4579966027558271, -208.1989085970629105 ) ) ;
#26686 = EDGE_LOOP ( 'NONE', ( #72283, #80038, #84095, #47063, #92348, #73770, #32301 ) ) ;
#26687 = CARTESIAN_POINT ( 'NONE',  ( -85.80823110288866928, -273.4019493347999514, -210.5280554229012182 ) ) ;
#26688 = CARTESIAN_POINT ( 'NONE',  ( -106.2305628964040380, -292.9106721050465012, -241.4833040373116830 ) ) ;
#26689 = CARTESIAN_POINT ( 'NONE',  ( 208.6208076322478746, 32.98517505407394168, 12.09245862095555601 ) ) ;
#26690 = CARTESIAN_POINT ( 'NONE',  ( -72.02372285203398405, -297.9805209788416391, -342.4524372437778652 ) ) ;
#26691 = VERTEX_POINT ( 'NONE', #8939 ) ;
#26692 = CARTESIAN_POINT ( 'NONE',  ( 10.63557830801703474, -272.7126596835998953, -212.4297516463423960 ) ) ;
#26693 = DIRECTION ( 'NONE',  ( -0.5335274993777934238, 0.8457827187922903889, 0.000000000000000000 ) ) ;
#26694 = CARTESIAN_POINT ( 'NONE',  ( -109.5937020379772093, -294.6439827360587174, -294.5703855230362365 ) ) ;
#26695 = CARTESIAN_POINT ( 'NONE',  ( -105.8613594928522588, -296.3993908458012925, -244.8568972348122941 ) ) ;
#26696 = CARTESIAN_POINT ( 'NONE',  ( -31.80007785805864629, -290.5012212748150091, -343.8969021430283988 ) ) ;
#26697 = CARTESIAN_POINT ( 'NONE',  ( 21.83340476600337965, -283.9281828454697916, -314.8374508501866558 ) ) ;
#26698 = CARTESIAN_POINT ( 'NONE',  ( -48.76286128286598398, -290.6200099286714362, -345.9670361056142838 ) ) ;
#26699 = CARTESIAN_POINT ( 'NONE',  ( -112.4441006938225911, -292.0518508526362780, -255.7007530701744145 ) ) ;
#26700 = CARTESIAN_POINT ( 'NONE',  ( -22.07700354926762998, -288.2477330005200429, -196.8776510896352363 ) ) ;
#26701 = CARTESIAN_POINT ( 'NONE',  ( -79.91254976740866312, -279.6605278899509699, -206.1354645271921413 ) ) ;
#26702 = CARTESIAN_POINT ( 'NONE',  ( -111.9634914974103737, -294.7843254702183913, -258.4090831289626067 ) ) ;
#26703 = CARTESIAN_POINT ( 'NONE',  ( -70.47204212879293550, -283.3101654618914722, -339.8837119342994697 ) ) ;
#26704 = CARTESIAN_POINT ( 'NONE',  ( 35.93017762072240373, -277.5712424504486648, -282.5927812587456174 ) ) ;
#26705 = EDGE_CURVE ( 'NONE', #73161, #45887, #71982, .T. ) ;
#26706 = CARTESIAN_POINT ( 'NONE',  ( -37.37352853689063892, -300.5519495502701943, -195.3611179825600175 ) ) ;
#26707 = CARTESIAN_POINT ( 'NONE',  ( 35.90279160379202494, -274.0493711301563167, -290.6387294181315042 ) ) ;
#26708 = CARTESIAN_POINT ( 'NONE',  ( 128.9467878515196162, -299.5541904835127980, -200.7046326357662167 ) ) ;
#26709 = CARTESIAN_POINT ( 'NONE',  ( 33.70852362246065326, -281.2849055538088692, -287.4394281841307475 ) ) ;
#26710 = CARTESIAN_POINT ( 'NONE',  ( -113.9808707652687332, -279.7773802568665928, -268.7579503831991019 ) ) ;
#26711 = CARTESIAN_POINT ( 'NONE',  ( -60.42770478585716631, -284.8187905249547498, -197.0946735001964782 ) ) ;
#26712 = CARTESIAN_POINT ( 'NONE',  ( 31.76667377241848556, -294.9632711882800891, -243.8657095369515844 ) ) ;
#26713 = CARTESIAN_POINT ( 'NONE',  ( -103.5446941996294612, -274.6486547209605078, -232.5245009089235282 ) ) ;
#26714 = CARTESIAN_POINT ( 'NONE',  ( -67.35769383500377216, -274.9818023116616246, -199.9882652951150135 ) ) ;
#26715 = DIRECTION ( 'NONE',  ( -1.000000000000000000, -0.000000000000000000, -0.000000000000000000 ) ) ;
#26716 = CARTESIAN_POINT ( 'NONE',  ( 29.15339240532204101, -275.7914696594816064, -300.4842432098263885 ) ) ;
#26717 = CARTESIAN_POINT ( 'NONE',  ( -103.0656304090098558, -298.0758436247911050, -306.1437033027143002 ) ) ;
#26718 = CARTESIAN_POINT ( 'NONE',  ( -98.04749957200297672, -283.1492142525569307, -226.5804470698925570 ) ) ;
#26719 = CARTESIAN_POINT ( 'NONE',  ( 39.20557941290697812, -293.1109296196158880, -261.7325060403586008 ) ) ;
#26720 = CARTESIAN_POINT ( 'NONE',  ( 28.09020284683080249, -273.0911317999635344, -234.3296155778404568 ) ) ;
#26721 = CARTESIAN_POINT ( 'NONE',  ( 0.3415919811142267837, -290.1594153328171615, -336.6507297303911059 ) ) ;
#26722 = CARTESIAN_POINT ( 'NONE',  ( 30.14567044497053061, -292.0881689145955420, -241.6011181777199681 ) ) ;
#26723 = ORIENTED_EDGE ( 'NONE', *, *, #42150, .F. ) ;
#26724 = CARTESIAN_POINT ( 'NONE',  ( 8.511947109087856234, -291.2407382222393153, -209.1718393089742563 ) ) ;
#26725 = VERTEX_POINT ( 'NONE', #31215 ) ;
#26726 = CARTESIAN_POINT ( 'NONE',  ( -101.1400853280757275, -290.7056938149839880, -234.7346959321048416 ) ) ;
#26727 = ORIENTED_EDGE ( 'NONE', *, *, #18614, .T. ) ;
#26728 = CARTESIAN_POINT ( 'NONE',  ( 19.40482051515830619, -289.3359029226850794, -321.9687132998352581 ) ) ;
#26729 = CARTESIAN_POINT ( 'NONE',  ( -109.9876022629710519, -278.9893312455164960, -262.4829533495619671 ) ) ;
#26730 = CARTESIAN_POINT ( 'NONE',  ( -47.60387215835924479, -294.1000392679046058, -346.3623043837709474 ) ) ;
#26731 = CARTESIAN_POINT ( 'NONE',  ( -57.73689604186656510, -286.4470393917743536, -196.1617298398948037 ) ) ;
#26732 = CARTESIAN_POINT ( 'NONE',  ( -114.3336063875097039, -284.8542623932090123, -272.8527847642692450 ) ) ;
#26733 = CARTESIAN_POINT ( 'NONE',  ( -61.53772696028209310, -283.7084779206152803, -339.3102300259312756 ) ) ;
#26734 = CARTESIAN_POINT ( 'NONE',  ( 202.2819390781037328, 293.6457075726772246, -83.22913366109028743 ) ) ;
#26735 = CARTESIAN_POINT ( 'NONE',  ( -114.3334814850269652, -272.1971439235380785, -284.0165574570778517 ) ) ;
#26736 = CARTESIAN_POINT ( 'NONE',  ( 178.3113800505042263, 252.0692767011776141, -164.4075532967166282 ) ) ;
#26737 = VECTOR ( 'NONE', #1790, 1000.000000000000000 ) ;
#26738 = CARTESIAN_POINT ( 'NONE',  ( 32.66794128697139143, -275.0304942085265907, -291.6472148795279509 ) ) ;
#26739 = CARTESIAN_POINT ( 'NONE',  ( 35.00997217543812212, -274.6316298465533237, -282.4768840196937276 ) ) ;
#26740 = CARTESIAN_POINT ( 'NONE',  ( -113.8826363757102342, -295.9620406538865609, -278.1721346557389438 ) ) ;
#26741 = CARTESIAN_POINT ( 'NONE',  ( 168.6450565192255908, 229.6397774369325191, -190.3058657457524987 ) ) ;
#26742 = CARTESIAN_POINT ( 'NONE',  ( 5.580683173876516356, -275.1687501424511311, -333.6933158240120747 ) ) ;
#26743 = CARTESIAN_POINT ( 'NONE',  ( -109.5281245247177395, -274.5249336607064379, -254.0181026674689235 ) ) ;
#26744 = EDGE_LOOP ( 'NONE', ( #32317, #87743, #85385, #58832 ) ) ;
#26745 = CARTESIAN_POINT ( 'NONE',  ( -68.09424279708272820, -298.5995022204775182, -199.9688556016709242 ) ) ;
#26746 = CARTESIAN_POINT ( 'NONE',  ( 12.20213218960536317, -288.8329435094427140, -324.1271433072680566 ) ) ;
#26747 = CARTESIAN_POINT ( 'NONE',  ( -37.67798924117062143, -295.8590548613066176, -347.2119575608210198 ) ) ;
#26748 = CARTESIAN_POINT ( 'NONE',  ( -114.1719552471954842, -296.9821601478535058, -275.3416426531995285 ) ) ;
#26749 = CARTESIAN_POINT ( 'NONE',  ( -20.07422210092791559, -292.4468366246763935, -199.3804751816619785 ) ) ;
#26750 = VERTEX_POINT ( 'NONE', #88939 ) ;
#26751 = CARTESIAN_POINT ( 'NONE',  ( 36.53225936691014653, -277.2692256905613704, -254.4270362188295564 ) ) ;
#26752 = EDGE_CURVE ( 'NONE', #11101, #37419, #3725, .T. ) ;
#26753 = ORIENTED_EDGE ( 'NONE', *, *, #54874, .F. ) ;
#26754 = CARTESIAN_POINT ( 'NONE',  ( 38.73484462456460165, -280.9117392967417004, -258.5312220010501392 ) ) ;
#26755 = CARTESIAN_POINT ( 'NONE',  ( -8.635436142503104762, -277.6082965895639063, -337.7494695137468739 ) ) ;
#26756 = CARTESIAN_POINT ( 'NONE',  ( -28.69380377777484981, -278.7042004190103626, -345.9069553965588852 ) ) ;
#26757 = CARTESIAN_POINT ( 'NONE',  ( -53.79716647774889537, -275.2822944587104530, -343.9511463772141724 ) ) ;
#26758 = CARTESIAN_POINT ( 'NONE',  ( -75.27061711250985354, -298.1838275818548141, -207.8101070488927178 ) ) ;
#26759 = CARTESIAN_POINT ( 'NONE',  ( -109.9472088980176352, -294.9699439457618269, -282.3534077577143080 ) ) ;
#26760 = CARTESIAN_POINT ( 'NONE',  ( 152.6996702291409633, 19.85642976176117358, -8.932053473878653449 ) ) ;
#26761 = CARTESIAN_POINT ( 'NONE',  ( -69.94201088550713052, -280.1265866060051621, -200.6563771082540200 ) ) ;
#26762 = CARTESIAN_POINT ( 'NONE',  ( 13.73284503741700924, -276.4787771678597323, -322.5888861671180621 ) ) ;
#26763 = CARTESIAN_POINT ( 'NONE',  ( 18.27474897256593067, -286.9591091875677193, -322.8978561957890747 ) ) ;
#26764 = CARTESIAN_POINT ( 'NONE',  ( -43.17355122162680203, -299.9789741424969520, -195.3690785949184487 ) ) ;
#26765 = CARTESIAN_POINT ( 'NONE',  ( 82.61703178011177329, -302.0572532870764917, -195.4731947519462381 ) ) ;
#26766 = CARTESIAN_POINT ( 'NONE',  ( 21.29679143005557762, -287.3620939802576686, -314.1328459475130899 ) ) ;
#26767 = CARTESIAN_POINT ( 'NONE',  ( 7.777565281487036408, -278.9173574572075722, -211.6257724223393950 ) ) ;
#26769 = CARTESIAN_POINT ( 'NONE',  ( -54.03593491015463712, -281.3478465225171021, -342.9581291951858475 ) ) ;
#26768 = CARTESIAN_POINT ( 'NONE',  ( -98.47304628710297436, -277.6924307189788692, -229.3031982849115877 ) ) ;
#26770 = CARTESIAN_POINT ( 'NONE',  ( 19.78164113593015472, -288.8793855325270101, -221.7419617896272257 ) ) ;
#26771 = CARTESIAN_POINT ( 'NONE',  ( -109.5253815661579750, -279.9316113518907514, -257.0702700157197569 ) ) ;
#26772 = DIRECTION ( 'NONE',  ( -1.000000000000000000, 0.000000000000000000, 0.000000000000000000 ) ) ;
#26773 = CARTESIAN_POINT ( 'NONE',  ( 9.840308027229815124, -294.7015614803166841, -211.9945877116911674 ) ) ;
#26774 = CARTESIAN_POINT ( 'NONE',  ( -111.5004251917811757, -276.5820645079326141, -286.9278773107641882 ) ) ;
#26775 = CARTESIAN_POINT ( 'NONE',  ( -35.10621908121218837, -277.6747570548651538, -343.4288625280283327 ) ) ;
#26776 = CARTESIAN_POINT ( 'NONE',  ( -0.01927517540570689372, -284.5569116127358598, -335.6221778246190297 ) ) ;
#26777 = CARTESIAN_POINT ( 'NONE',  ( 196.4521542616569434, 72.01334855021748638, 11.25845938509887034 ) ) ;
#26778 = CARTESIAN_POINT ( 'NONE',  ( -51.39309154084573095, -291.1506368762147190, -344.6031047197599264 ) ) ;
#26779 = CARTESIAN_POINT ( 'NONE',  ( -93.43172067399453340, -295.2448062213551339, -220.5533411413741192 ) ) ;
#26780 = CARTESIAN_POINT ( 'NONE',  ( -68.42604364488623503, -284.8512438904770647, -200.0764205640718671 ) ) ;
#26781 = CARTESIAN_POINT ( 'NONE',  ( 209.3190042249899250, 30.23012903947020646, 14.26380412667039010 ) ) ;
#26782 = CARTESIAN_POINT ( 'NONE',  ( -74.50841538816288789, -272.2318228359258114, -206.8996594922552390 ) ) ;
#26783 = CARTESIAN_POINT ( 'NONE',  ( -32.04591552392162157, -290.2592168845200717, -196.3022163802394289 ) ) ;
#26784 = LINE ( 'NONE', #69395, #69956 ) ;
#26785 = CARTESIAN_POINT ( 'NONE',  ( 29.33919985515026596, -280.8906705383787994, 27.50000000000000000 ) ) ;
#26786 = CARTESIAN_POINT ( 'NONE',  ( -25.11330357806730618, -290.6852544266612313, -195.0406422206420416 ) ) ;
#26787 = CARTESIAN_POINT ( 'NONE',  ( -100.3023504785266908, -286.6781908489620605, -231.7618021565259596 ) ) ;
#26788 = CARTESIAN_POINT ( 'NONE',  ( 21.32233432843219134, -285.1345184668953721, -222.0651028445196857 ) ) ;
#26789 = CARTESIAN_POINT ( 'NONE',  ( -65.33403583430848016, -287.1043540183163714, -202.2495104004988491 ) ) ;
#26790 = DIRECTION ( 'NONE',  ( 0.000000000000000000, 0.000000000000000000, -1.000000000000000000 ) ) ;
#26791 = CARTESIAN_POINT ( 'NONE',  ( -22.43690667272922923, -287.0505977705300893, -198.6819724489680823 ) ) ;
#26792 = CARTESIAN_POINT ( 'NONE',  ( -14.39190050869001070, -294.3280006531069830, -198.5309070168546839 ) ) ;
#26793 = CARTESIAN_POINT ( 'NONE',  ( 35.10569085269639089, -273.9069397194713247, -291.8704007981729092 ) ) ;
#26794 = CARTESIAN_POINT ( 'NONE',  ( 38.16245962426862803, -276.0730230554119657, -285.3566557088650484 ) ) ;
#26795 = CARTESIAN_POINT ( 'NONE',  ( -9.027696117552387989, -290.4994204145099843, -200.3066293631628128 ) ) ;
#26796 = CARTESIAN_POINT ( 'NONE',  ( -112.4844053670614841, -278.3419207576978920, -287.1710510391713456 ) ) ;
#26797 = CARTESIAN_POINT ( 'NONE',  ( -110.6660317147119201, -298.7132563259610833, -256.3147549761018809 ) ) ;
#26798 = CARTESIAN_POINT ( 'NONE',  ( -48.18343439339133027, -250.5789762915055405, -484.9196478893141489 ) ) ;
#26799 = CARTESIAN_POINT ( 'NONE',  ( 41.08708295871279859, -296.0521521680024080, -465.6442049081569508 ) ) ;
#26800 = CARTESIAN_POINT ( 'NONE',  ( -107.4613583187515502, -282.9471993809232231, -292.3719565269367990 ) ) ;
#26801 = CARTESIAN_POINT ( 'NONE',  ( 11.70403046443786543, -278.7329559851858107, -213.6203305672067643 ) ) ;
#26802 = LINE ( 'NONE', #55688, #40710 ) ;
#26803 = CARTESIAN_POINT ( 'NONE',  ( 23.09566817772254765, -273.4044882982954618, -223.7562380433323597 ) ) ;
#26804 = CARTESIAN_POINT ( 'NONE',  ( -70.50644846288548706, -276.8500975787258085, -335.5070475284564964 ) ) ;
#26805 = CARTESIAN_POINT ( 'NONE',  ( -28.79654450267103272, -296.4621202232191877, -343.6088471089033192 ) ) ;
#26806 = CARTESIAN_POINT ( 'NONE',  ( 19.90713851165421744, -279.7777003198740999, -219.3113472844424336 ) ) ;
#26807 = CARTESIAN_POINT ( 'NONE',  ( -84.62089232753784529, -296.6632429145123524, -326.3569905383864693 ) ) ;
#26808 = CARTESIAN_POINT ( 'NONE',  ( -99.59738945185569037, -297.2734305052078980, -314.9197229273113408 ) ) ;
#26809 = CARTESIAN_POINT ( 'NONE',  ( -94.62665685498387802, -272.8576989399874719, -225.0784367492727256 ) ) ;
#26810 = CARTESIAN_POINT ( 'NONE',  ( -110.6712509847548915, -292.7544217102014841, -254.6201642601380684 ) ) ;
#26811 = CARTESIAN_POINT ( 'NONE',  ( -109.0292583420370107, -285.0767217503002371, -242.1110506428756821 ) ) ;
#26812 = CARTESIAN_POINT ( 'NONE',  ( -4.551223575848055702, -274.7643480253225334, -338.6768466695388611 ) ) ;
#26813 = CARTESIAN_POINT ( 'NONE',  ( 37.50391401686425041, -287.6123362159589760, -288.5036594769578642 ) ) ;
#26814 = CARTESIAN_POINT ( 'NONE',  ( -38.40199223413036833, -282.0186904250356861, -195.7111638853811257 ) ) ;
#26815 = ADVANCED_FACE ( 'NONE', ( #61500 ), #60561, .T. ) ;
#26816 = CARTESIAN_POINT ( 'NONE',  ( 19.70600566168781143, -285.9635036919077606, -224.4177466393263671 ) ) ;
#26817 = CARTESIAN_POINT ( 'NONE',  ( -37.75769415766401238, -290.0467844270335718, -195.3622673089417106 ) ) ;
#26818 = CARTESIAN_POINT ( 'NONE',  ( 143.8719904363247224, 176.7915900130879550, -240.1109971732525139 ) ) ;
#26819 = CARTESIAN_POINT ( 'NONE',  ( 2.485805911679377367, -286.1097186457844828, -209.1095204178920142 ) ) ;
#26820 = CARTESIAN_POINT ( 'NONE',  ( 198.9670582353434156, 298.8125465311976541, -6.365364976313826695 ) ) ;
#26821 = CARTESIAN_POINT ( 'NONE',  ( -112.6916892114120969, -289.7957896498892865, -255.6230206211112659 ) ) ;
#26822 = CARTESIAN_POINT ( 'NONE',  ( -31.15920254897837438, -281.7290107928711791, -194.3601949015528874 ) ) ;
#26823 = CARTESIAN_POINT ( 'NONE',  ( -113.2301690418536708, -279.9945947957406815, -260.2497534472397547 ) ) ;
#26824 = CARTESIAN_POINT ( 'NONE',  ( 33.76087186793013473, -281.1673367844774134, -253.8255726304529674 ) ) ;
#26825 = CARTESIAN_POINT ( 'NONE',  ( -1.992923467461159781, -276.5204772878800554, -204.2138229537782479 ) ) ;
#26826 = CARTESIAN_POINT ( 'NONE',  ( -22.09754671479725729, -294.8620415794547966, -345.8370465075689708 ) ) ;
#26827 = CARTESIAN_POINT ( 'NONE',  ( -93.78404694279149112, -289.2530164745510319, -221.5133105489995557 ) ) ;
#26828 = CARTESIAN_POINT ( 'NONE',  ( -103.5567290587240592, -271.7730163139419233, -238.6956723466515768 ) ) ;
#26829 = ORIENTED_EDGE ( 'NONE', *, *, #56718, .T. ) ;
#26830 = CARTESIAN_POINT ( 'NONE',  ( -92.72027240347070176, -285.7738895905237086, -320.1249180760857485 ) ) ;
#26831 = CARTESIAN_POINT ( 'NONE',  ( 37.45675393577254653, -294.4185431453886395, -253.3705475995725465 ) ) ;
#26832 = CARTESIAN_POINT ( 'NONE',  ( 19.43645414211531275, -282.8543406865946395, -316.4257628595906340 ) ) ;
#26833 = CARTESIAN_POINT ( 'NONE',  ( 15.87258305593260488, -273.8429382517226145, -215.0342684632966836 ) ) ;
#26834 = CARTESIAN_POINT ( 'NONE',  ( -111.8977884956055959, -291.4401261739023425, -251.4745095140122260 ) ) ;
#26835 = CARTESIAN_POINT ( 'NONE',  ( -18.46647227692133697, -284.4322324114499452, -196.9309369347271002 ) ) ;
#26836 = CARTESIAN_POINT ( 'NONE',  ( 19.39720699260034564, -293.1774582755224401, -218.3376549078637368 ) ) ;
#26837 = CARTESIAN_POINT ( 'NONE',  ( 28.82732507518608855, -287.4685382405709788, -239.4783138623467664 ) ) ;
#26838 = FACE_OUTER_BOUND ( 'NONE', #29382, .T. ) ;
#26839 = DIRECTION ( 'NONE',  ( 0.000000000000000000, 1.000000000000000000, 0.000000000000000000 ) ) ;
#26840 = CARTESIAN_POINT ( 'NONE',  ( -47.25908889419609693, -155.3473324462872256, -361.3472553374705853 ) ) ;
#26841 = CARTESIAN_POINT ( 'NONE',  ( -96.62141794101545145, -285.4217361794195540, -318.4297758286915609 ) ) ;
#26842 = CARTESIAN_POINT ( 'NONE',  ( -95.99890600148557951, -281.4094976428775681, -317.0979686699210447 ) ) ;
#26843 = ORIENTED_EDGE ( 'NONE', *, *, #62073, .T. ) ;
#26844 = CARTESIAN_POINT ( 'NONE',  ( 25.40796231749686385, -279.9517827164313530, -232.3588101084200730 ) ) ;
#26845 = CARTESIAN_POINT ( 'NONE',  ( -35.71621215618927181, -276.6990367714955710, -347.3359302886096316 ) ) ;
#26846 = CARTESIAN_POINT ( 'NONE',  ( -11.12412658756482209, -282.3946609980220046, -200.2159046499775741 ) ) ;
#26847 = CARTESIAN_POINT ( 'NONE',  ( -53.93747043463056201, -170.5330345533709817, -362.6169925651183803 ) ) ;
#26848 = CARTESIAN_POINT ( 'NONE',  ( 20.63100012324902721, -279.4496711621522422, -220.5639895147556047 ) ) ;
#26849 = CARTESIAN_POINT ( 'NONE',  ( -42.76911677567638748, -284.0034641821418973, -195.9009786142026712 ) ) ;
#26850 = CARTESIAN_POINT ( 'NONE',  ( -111.2934068659050553, -298.5336694902977115, -252.8934596384129350 ) ) ;
#26851 = CARTESIAN_POINT ( 'NONE',  ( 16.20850676895009101, -294.7582654708452310, -320.0638722622853152 ) ) ;
#26852 = ORIENTED_EDGE ( 'NONE', *, *, #10935, .T. ) ;
#26853 = CARTESIAN_POINT ( 'NONE',  ( -70.42783299816018427, -290.2912985678847804, -204.7367986250583840 ) ) ;
#26854 = CARTESIAN_POINT ( 'NONE',  ( 19.80701368685719288, -276.9030616083088603, -321.8331081465513535 ) ) ;
#26855 = CARTESIAN_POINT ( 'NONE',  ( -39.17045607675562024, -298.1952824628344842, -197.3716191773571040 ) ) ;
#26856 = ORIENTED_EDGE ( 'NONE', *, *, #57902, .T. ) ;
#26857 = CARTESIAN_POINT ( 'NONE',  ( -95.78317314525202164, -272.1448369148741904, -220.6811935807979239 ) ) ;
#26858 = DIRECTION ( 'NONE',  ( 0.000000000000000000, -1.000000000000000000, 0.000000000000000000 ) ) ;
#26859 = CARTESIAN_POINT ( 'NONE',  ( 175.2296996224749250, 275.0000000000000568, -24.99999999999999289 ) ) ;
#26860 = DIRECTION ( 'NONE',  ( 5.551115123125777653E-14, 0.000000000000000000, 1.000000000000000000 ) ) ;
#26861 = CARTESIAN_POINT ( 'NONE',  ( 21.26527303377238809, -283.2478230585751930, -314.4210398522913579 ) ) ;
#26862 = CARTESIAN_POINT ( 'NONE',  ( 38.39983156410941945, -283.2350025256452000, -264.2623977158010575 ) ) ;
#26863 = CARTESIAN_POINT ( 'NONE',  ( -107.5772015095370904, -283.8866144012503128, -249.4396665204372709 ) ) ;
#26864 = CARTESIAN_POINT ( 'NONE',  ( 35.89741892663457179, -274.0758245481443964, -279.8491786707871256 ) ) ;
#26865 = CARTESIAN_POINT ( 'NONE',  ( 24.70206849985540387, -282.8557346562886323, -229.5077386161238167 ) ) ;
#26866 = CARTESIAN_POINT ( 'NONE',  ( 34.25557951501436094, -274.2607410098478340, -287.8652135231621969 ) ) ;
#26867 = EDGE_CURVE ( 'NONE', #44141, #34864, #11218, .T. ) ;
#26868 = CARTESIAN_POINT ( 'NONE',  ( 179.7289557593406357, 250.0000000000000568, -24.91818181818184641 ) ) ;
#26869 = CARTESIAN_POINT ( 'NONE',  ( 29.36161962560460381, -276.2220507363093702, -239.8263110182279831 ) ) ;
#26870 = EDGE_CURVE ( 'NONE', #12173, #25231, #27589, .T. ) ;
#26871 = CARTESIAN_POINT ( 'NONE',  ( -104.8288747155036305, -278.8785657172734886, -307.0985659920087301 ) ) ;
#26872 = ORIENTED_EDGE ( 'NONE', *, *, #27217, .T. ) ;
#26873 = ORIENTED_EDGE ( 'NONE', *, *, #82203, .T. ) ;
#26874 = PLANE ( 'NONE',  #64107 ) ;
#26875 = CARTESIAN_POINT ( 'NONE',  ( -112.6731653155462993, -286.3097194944880926, -278.4528317648333200 ) ) ;
#26876 = CARTESIAN_POINT ( 'NONE',  ( -88.62230904007013521, -294.9910732068373704, -322.6137471060431494 ) ) ;
#26877 = CARTESIAN_POINT ( 'NONE',  ( -57.27248934188107654, -288.6512440413138165, -344.6864449927168152 ) ) ;
#26878 = CARTESIAN_POINT ( 'NONE',  ( -22.23135365226562143, -284.4880363566454093, -197.8540352875978101 ) ) ;
#26879 = EDGE_CURVE ( 'NONE', #17769, #45666, #47215, .T. ) ;
#26881 = CARTESIAN_POINT ( 'NONE',  ( -42.76016990518110106, -287.3611652722732970, -344.2271534680248237 ) ) ;
#26880 = CARTESIAN_POINT ( 'NONE',  ( -108.3343556861541970, -282.8723850060145537, -289.7844381861559100 ) ) ;
#26882 = CARTESIAN_POINT ( 'NONE',  ( -91.95026354765967369, -285.0589267341172786, -319.4211842818626224 ) ) ;
#26883 = CARTESIAN_POINT ( 'NONE',  ( 37.14800832392594998, -273.6697087532749038, -279.5293646701454691 ) ) ;
#26884 = CARTESIAN_POINT ( 'NONE',  ( 23.23796148366297487, -285.3290903211996579, -224.1169414945194944 ) ) ;
#26885 = CARTESIAN_POINT ( 'NONE',  ( -110.9313838304562410, -298.7390324570658890, -255.8188038662694908 ) ) ;
#26886 = CARTESIAN_POINT ( 'NONE',  ( -112.3210213468869938, -282.6287637666725914, -264.3684214495649485 ) ) ;
#26887 = CARTESIAN_POINT ( 'NONE',  ( 33.33752256824769233, -282.2402889203216318, -251.1335982237621351 ) ) ;
#26888 = CARTESIAN_POINT ( 'NONE',  ( -92.23606277049911739, -291.8342549185520056, -321.7842996216700726 ) ) ;
#26889 = DIRECTION ( 'NONE',  ( 0.000000000000000000, 0.000000000000000000, 1.000000000000000000 ) ) ;
#26890 = CARTESIAN_POINT ( 'NONE',  ( 208.6208076322478746, 32.98517505407394168, 15.00000000000000000 ) ) ;
#26891 = CARTESIAN_POINT ( 'NONE',  ( -11.52577693407175907, -296.6388007047333417, -341.4296799426973621 ) ) ;
#26892 = CARTESIAN_POINT ( 'NONE',  ( -75.50204382171713746, -277.5434202744431218, -205.7352763166446437 ) ) ;
#26893 = CARTESIAN_POINT ( 'NONE',  ( -109.0814529087638505, -294.7253750149093889, -287.7305967525836650 ) ) ;
#26894 = CARTESIAN_POINT ( 'NONE',  ( -2.903275930910505398, -279.2021027020170436, -205.4219755186740883 ) ) ;
#26895 = CARTESIAN_POINT ( 'NONE',  ( 27.91034656212066167, -273.1508603088242921, -234.4278689206720401 ) ) ;
#26896 = CARTESIAN_POINT ( 'NONE',  ( 34.96537223064265731, -294.6941036798717732, -257.1409115309351705 ) ) ;
#26897 = CARTESIAN_POINT ( 'NONE',  ( 21.31550574532285580, -290.6948066931273615, -317.0979686699210447 ) ) ;
#26898 = CARTESIAN_POINT ( 'NONE',  ( -77.81814523701829955, -295.9987894828858543, -205.6744490061366264 ) ) ;
#26899 = CARTESIAN_POINT ( 'NONE',  ( 34.50197405081497948, -291.4740911172476672, -245.4537650808617570 ) ) ;
#26900 = CARTESIAN_POINT ( 'NONE',  ( -109.8605565985053971, -292.1448901237440055, -257.5641528542200263 ) ) ;
#26901 = CARTESIAN_POINT ( 'NONE',  ( 120.8395553409046528, -299.5541904835127980, -195.3611179825600175 ) ) ;
#26902 = CARTESIAN_POINT ( 'NONE',  ( -109.8615812104604998, -291.4871940426499464, -260.3170556970085840 ) ) ;
#26903 = DIRECTION ( 'NONE',  ( -0.000000000000000000, -0.000000000000000000, -1.000000000000000000 ) ) ;
#26904 = AXIS2_PLACEMENT_3D ( 'NONE', #64489, #14734, #72039 ) ;
#26905 = CARTESIAN_POINT ( 'NONE',  ( -113.6130288952681582, -291.8536350093470446, -262.6920504382006811 ) ) ;
#26907 = CARTESIAN_POINT ( 'NONE',  ( 33.94980566938370714, -293.3442674938572168, -254.6023236270237931 ) ) ;
#26906 = CARTESIAN_POINT ( 'NONE',  ( 37.55107935066549629, -279.4598822186044913, -261.5674888522430024 ) ) ;
#26908 = CARTESIAN_POINT ( 'NONE',  ( 20.12868591505343119, -280.8571973516890807, -219.0952707735880267 ) ) ;
#26909 = CARTESIAN_POINT ( 'NONE',  ( -50.09418622537307897, -282.8772141248481944, -346.3301839254096421 ) ) ;
#26910 = CARTESIAN_POINT ( 'NONE',  ( 25.02364740037101143, -286.1121439429087445, -311.7438139391302343 ) ) ;
#26911 = CARTESIAN_POINT ( 'NONE',  ( -67.07571345920861461, -281.5856783223593993, -338.3951675371041006 ) ) ;
#26912 = CARTESIAN_POINT ( 'NONE',  ( 207.6175730408114930, 30.32598770090644180, 14.41714557868295898 ) ) ;
#26913 = CARTESIAN_POINT ( 'NONE',  ( 31.40531251692992853, -279.6019916771198268, -237.1252048540661121 ) ) ;
#26914 = CARTESIAN_POINT ( 'NONE',  ( -29.48089718485516642, -285.0698438799033738, -194.0741578481965348 ) ) ;
#26915 = CARTESIAN_POINT ( 'NONE',  ( 195.6860740630249893, 40.71007109152891701, 14.68571759922588704 ) ) ;
#26916 = CARTESIAN_POINT ( 'NONE',  ( -2.074870657405986751, -294.1273887602113177, -205.5186025678350461 ) ) ;
#26917 = CARTESIAN_POINT ( 'NONE',  ( 23.99595064063498029, -276.3668564437114696, -224.7946951208070345 ) ) ;
#26918 = CARTESIAN_POINT ( 'NONE',  ( -35.12124398369961398, -276.6902219015913147, -343.3484940236178886 ) ) ;
#26919 = CARTESIAN_POINT ( 'NONE',  ( -112.5648884630178088, -290.5131509328750781, -286.8071491530723733 ) ) ;
#26920 = CARTESIAN_POINT ( 'NONE',  ( -37.33931516258178362, -281.1319380449236291, -345.9339424150234663 ) ) ;
#26921 = CARTESIAN_POINT ( 'NONE',  ( 19.53608827460852382, -291.9601006936595127, -224.2074999027515503 ) ) ;
#26922 = CARTESIAN_POINT ( 'NONE',  ( -98.39563956292968783, -293.9586314611743774, -314.0079825295288742 ) ) ;
#26923 = ORIENTED_EDGE ( 'NONE', *, *, #32342, .T. ) ;
#26924 = CARTESIAN_POINT ( 'NONE',  ( 152.8567950062511329, 19.85971597382930298, 11.17893457256845657 ) ) ;
#26925 = CARTESIAN_POINT ( 'NONE',  ( -2.404497430382225076, -292.0352512285432454, -206.1800939655338141 ) ) ;
#26926 = CARTESIAN_POINT ( 'NONE',  ( -53.35057174420112602, -292.7666405000204577, -340.3538533559490702 ) ) ;
#26927 = CARTESIAN_POINT ( 'NONE',  ( -112.3679711185133812, -295.8154061841117937, -254.0554609655942215 ) ) ;
#26928 = CARTESIAN_POINT ( 'NONE',  ( -1.695295401843315952, -278.6590157914766337, -203.5057568470470244 ) ) ;
#26929 = CARTESIAN_POINT ( 'NONE',  ( 25.93998426618589903, -288.2964805407460176, -227.3409005452003271 ) ) ;
#26930 = CARTESIAN_POINT ( 'NONE',  ( -41.32080669932226158, -285.8340145623815829, -197.4571474487749470 ) ) ;
#26931 = CARTESIAN_POINT ( 'NONE',  ( -67.06472314849371230, -278.9691491034104160, -337.7944158142855713 ) ) ;
#26932 = CARTESIAN_POINT ( 'NONE',  ( -58.90699438193156112, -293.3526306158723855, -341.8228901694071737 ) ) ;
#26933 = CARTESIAN_POINT ( 'NONE',  ( -89.19602700144785956, -297.5536340744403105, -323.2450780946124951 ) ) ;
#26934 = CARTESIAN_POINT ( 'NONE',  ( -105.6428833645554874, -276.9896679005503302, -297.2326432929233988 ) ) ;
#26935 = VERTEX_POINT ( 'NONE', #8371 ) ;
#26936 = DIRECTION ( 'NONE',  ( -0.000000000000000000, 1.000000000000000000, 0.000000000000000000 ) ) ;
#26937 = CARTESIAN_POINT ( 'NONE',  ( -95.56828596756385252, -295.5384795456581060, -320.7139629176973017 ) ) ;
#26938 = CARTESIAN_POINT ( 'NONE',  ( -109.1472655586457563, -292.7266160176934591, -250.7326954000629939 ) ) ;
#26939 = CARTESIAN_POINT ( 'NONE',  ( 202.4561393373856220, 292.0274278529104208, -53.99999999997706368 ) ) ;
#26940 = CARTESIAN_POINT ( 'NONE',  ( 29.52164596457567569, -288.6021802054856948, -300.0364547155749051 ) ) ;
#26941 = CARTESIAN_POINT ( 'NONE',  ( -48.18343439339133027, -253.0206516619178956, -463.6604981723916694 ) ) ;
#26942 = ORIENTED_EDGE ( 'NONE', *, *, #52600, .F. ) ;
#26943 = CARTESIAN_POINT ( 'NONE',  ( 18.99565118791591800, -279.8984700940976040, -218.2178244569315666 ) ) ;
#26944 = CARTESIAN_POINT ( 'NONE',  ( -99.92071017042533754, -296.6097769036731506, -315.1406164243404646 ) ) ;
#26945 = CARTESIAN_POINT ( 'NONE',  ( -97.35509213141698126, -289.3191698664828664, -224.0940724576813921 ) ) ;
#26946 = CARTESIAN_POINT ( 'NONE',  ( -36.54515751558398051, -298.3951488193342811, -193.3822181063758592 ) ) ;
#26947 = CARTESIAN_POINT ( 'NONE',  ( 34.92805796460896772, -293.7476428251430320, -259.9126945604775756 ) ) ;
#26948 = DIRECTION ( 'NONE',  ( 0.000000000000000000, 1.000000000000000000, 0.000000000000000000 ) ) ;
#26949 = SURFACE_SIDE_STYLE ('',( #5188 ) ) ;
#26950 = DIRECTION ( 'NONE',  ( 1.000000000000000000, 0.000000000000000000, 0.000000000000000000 ) ) ;
#26951 = CARTESIAN_POINT ( 'NONE',  ( -31.85710892106038372, -290.5043823095820699, -346.5225100210599862 ) ) ;
#26952 = CARTESIAN_POINT ( 'NONE',  ( -111.2869819898779866, -281.4805209788416960, -234.7871824221999191 ) ) ;
#26953 = ORIENTED_EDGE ( 'NONE', *, *, #34457, .F. ) ;
#26954 = CARTESIAN_POINT ( 'NONE',  ( 36.88879320862066891, -280.6483970606656726, -250.2326502778686290 ) ) ;
#26955 = CARTESIAN_POINT ( 'NONE',  ( -60.57131821045653908, -287.7502956340750302, -199.2245361945525985 ) ) ;
#26956 = CARTESIAN_POINT ( 'NONE',  ( 25.07436444961066258, -285.5388665922002929, -226.2608800461145790 ) ) ;
#26957 = CARTESIAN_POINT ( 'NONE',  ( -94.29287010943507141, -271.2258015976106549, -221.7965970094414274 ) ) ;
#26958 = CARTESIAN_POINT ( 'NONE',  ( -8.433762185400381028, -276.3535585208446719, -201.7084461572123359 ) ) ;
#26959 = CARTESIAN_POINT ( 'NONE',  ( -95.39892191071538718, -289.2779651031976300, -223.7503861869165291 ) ) ;
#26960 = CARTESIAN_POINT ( 'NONE',  ( -84.08539553021272184, -279.5468794929855676, -330.0543740339704755 ) ) ;
#26961 = ORIENTED_EDGE ( 'NONE', *, *, #51060, .F. ) ;
#26963 = CARTESIAN_POINT ( 'NONE',  ( 2.766833846158528676, -279.9542100094539023, -209.1841064299111679 ) ) ;
#26962 = CARTESIAN_POINT ( 'NONE',  ( -67.30628832385720273, -279.6479354901900365, -203.7808274495207570 ) ) ;
#26964 = CARTESIAN_POINT ( 'NONE',  ( 39.00817925293942068, -276.5343402955103329, -262.5979085935651938 ) ) ;
#26965 = CARTESIAN_POINT ( 'NONE',  ( -105.8137324909532850, -277.7925123785902315, -235.8978731656794707 ) ) ;
#26966 = CARTESIAN_POINT ( 'NONE',  ( 199.7521944962045666, 291.7792511365457813, -82.56829223883464408 ) ) ;
#26967 = CARTESIAN_POINT ( 'NONE',  ( -106.6359884490323680, -273.9181512150559570, -237.3289848638757462 ) ) ;
#26968 = CARTESIAN_POINT ( 'NONE',  ( -20.68810176410567081, -299.6820650060397497, -193.9463967560282640 ) ) ;
#26969 = CARTESIAN_POINT ( 'NONE',  ( 31.98288692825981272, -284.4805209788416960, -303.7098442033569654 ) ) ;
#26970 = AXIS2_PLACEMENT_3D ( 'NONE', #43768, #71281, #13521 ) ;
#26971 = DIRECTION ( 'NONE',  ( -0.000000000000000000, 1.000000000000000000, -0.000000000000000000 ) ) ;
#26972 = CARTESIAN_POINT ( 'NONE',  ( 30.24142360882560965, -288.2507365597584794, -241.8264150553090133 ) ) ;
#26973 = CARTESIAN_POINT ( 'NONE',  ( 33.11133244103795192, -289.6801019631970462, -298.9679176900412472 ) ) ;
#26974 = CARTESIAN_POINT ( 'NONE',  ( -106.1312907718636751, -289.5717543808887626, -295.0974250455375341 ) ) ;
#26975 = CARTESIAN_POINT ( 'NONE',  ( -86.06824191627872267, -283.2148303486321197, -329.9031286004266690 ) ) ;
#26976 = CARTESIAN_POINT ( 'NONE',  ( 28.50428463181116356, -279.5030884062015275, -236.9198781703234999 ) ) ;
#26977 = CARTESIAN_POINT ( 'NONE',  ( -82.24422209915924498, -287.2924405619603476, -211.2457308303927732 ) ) ;
#26978 = CARTESIAN_POINT ( 'NONE',  ( 35.38470208894436553, -280.1875121436668223, -282.2597806675934748 ) ) ;
#26979 = EDGE_CURVE ( 'NONE', #37428, #70302, #12504, .T. ) ;
#26980 = CARTESIAN_POINT ( 'NONE',  ( -101.2488366394426151, -280.3610249661507510, -234.0689510607662953 ) ) ;
#26981 = CARTESIAN_POINT ( 'NONE',  ( -6.244744053618578761, -277.1245637039351664, -336.4881936594808849 ) ) ;
#26982 = CARTESIAN_POINT ( 'NONE',  ( -107.3746178472144095, -288.9474663571093629, -301.5303129079152882 ) ) ;
#26983 =( BOUNDED_SURFACE ( )  B_SPLINE_SURFACE ( 3, 2, ( 
 ( #64818, #57686, #16442 ),
 ( #15508, #38199, #22157 ),
 ( #73743, #854, #8403 ),
 ( #37281, #15988, #2247 ),
 ( #51479, #88402, #37733 ),
 ( #73291, #81296, #8855 ),
 ( #65745, #15050, #45294 ),
 ( #36825, #72357, #44840 ),
 ( #79468, #66187, #23552 ),
 ( #60017, #21695, #22604 ) ),
 .UNSPECIFIED., .F., .F., .F. ) 
 B_SPLINE_SURFACE_WITH_KNOTS ( ( 4, 2, 2, 2, 4 ),
 ( 3, 3 ),
 ( -2.168404344971008868E-19, 0.002513556688247616140, 0.005027113376495232280, 0.007540670064742848420, 0.01005422675299046456 ),
 ( 0.000000000000000000, 1.000000000000000000 ),
 .UNSPECIFIED. ) 
 GEOMETRIC_REPRESENTATION_ITEM ( )  RATIONAL_B_SPLINE_SURFACE ( (
 ( 1.000000000000000000, 0.8168508380123947754, 1.000000000000000000),
 ( 1.000000000000000000, 0.8469576315470376260, 1.000000000000000000),
 ( 1.000000000000000000, 0.8738409315859991811, 1.000000000000000000),
 ( 1.000000000000000000, 0.9200669567821229133, 1.000000000000000000),
 ( 1.000000000000000000, 0.9394145480628903755, 1.000000000000000000),
 ( 1.000000000000000000, 0.9701920524520508682, 1.000000000000000000),
 ( 1.000000000000000000, 0.9815163856013096044, 1.000000000000000000),
 ( 1.000000000000000000, 0.9964122006646789487, 1.000000000000000000),
 ( 1.000000000000000000, 1.000002041055608526, 1.000000000000000000),
 ( 1.000000000000000000, 1.000000000000000000, 1.000000000000000000) ) ) 
 REPRESENTATION_ITEM ( '' )  SURFACE ( )  );
#26984 = CARTESIAN_POINT ( 'NONE',  ( -103.9056962709803713, -285.8562167720805860, -231.8704799858673482 ) ) ;
#26985 = CARTESIAN_POINT ( 'NONE',  ( -58.46382961901134934, -283.8103215394305607, -344.3988831013352296 ) ) ;
#26986 = CARTESIAN_POINT ( 'NONE',  ( 5.593803564284941743, -282.6187377573604635, -329.3996014248699566 ) ) ;
#26987 = EDGE_LOOP ( 'NONE', ( #89711, #93376, #71721, #80635 ) ) ;
#26988 = CARTESIAN_POINT ( 'NONE',  ( -87.84405725080166860, -293.2154311974926486, -213.8826494905186451 ) ) ;
#26989 =( BOUNDED_SURFACE ( )  B_SPLINE_SURFACE ( 3, 2, ( 
 ( #28438, #21806, #43105 ),
 ( #6670, #27982, #58266 ),
 ( #63979, #80015, #72012 ),
 ( #15156, #14247, #36000 ),
 ( #13769, #28900, #93287 ),
 ( #50679, #56873, #42142 ),
 ( #35547, #64918, #71537 ),
 ( #64460, #79565, #7576 ),
 ( #57788, #57331, #92819 ),
 ( #86638, #42618, #87109 ) ),
 .UNSPECIFIED., .F., .F., .F. ) 
 B_SPLINE_SURFACE_WITH_KNOTS ( ( 4, 2, 2, 2, 4 ),
 ( 3, 3 ),
 ( 0.000000000000000000, 0.002512116609398717254, 0.005024233218797434508, 0.007536349828196151762, 0.01004846643759486902 ),
 ( 0.000000000000000000, 1.000000000000000000 ),
 .UNSPECIFIED. ) 
 GEOMETRIC_REPRESENTATION_ITEM ( )  RATIONAL_B_SPLINE_SURFACE ( (
 ( 1.000000000000000000, 0.8168508380123951085, 1.000000000000000000),
 ( 1.000000000000000000, 0.8469983227716978424, 1.000000000000000000),
 ( 1.000000000000000000, 0.8738795229725317970, 1.000000000000000000),
 ( 1.000000000000000000, 0.9200744724125300422, 1.000000000000000000),
 ( 1.000000000000000000, 0.9393932456999677383, 1.000000000000000000),
 ( 1.000000000000000000, 0.9701270577441517551, 1.000000000000000000),
 ( 1.000000000000000000, 0.9814990972768018462, 1.000000000000000000),
 ( 1.000000000000000000, 0.9964108658801225094, 1.000000000000000000),
 ( 1.000000000000000000, 1.000001410412673541, 1.000000000000000000),
 ( 1.000000000000000000, 1.000000000000000000, 1.000000000000000000) ) ) 
 REPRESENTATION_ITEM ( '' )  SURFACE ( )  );
#26990 = CARTESIAN_POINT ( 'NONE',  ( -4.798605359621682886, -291.1566862305271570, -201.1206294100695402 ) ) ;
#26991 = CARTESIAN_POINT ( 'NONE',  ( 34.35414921139504685, -274.4136814676367067, -255.3628606018893379 ) ) ;
#26992 = CARTESIAN_POINT ( 'NONE',  ( -101.5477394236903450, -295.3424703599969234, -312.7764287083693944 ) ) ;
#26993 = EDGE_CURVE ( 'NONE', #62368, #42343, #66156, .T. ) ;
#26994 = CARTESIAN_POINT ( 'NONE',  ( -96.33487913841184991, -288.4177170754038571, -314.5467917634023820 ) ) ;
#26995 = CARTESIAN_POINT ( 'NONE',  ( 36.30600289774800871, -291.6899377816716310, -262.5164834725144374 ) ) ;
#26996 = CARTESIAN_POINT ( 'NONE',  ( -72.53584868215146741, -290.7342172263004727, -334.7699870382133440 ) ) ;
#26997 = DIRECTION ( 'NONE',  ( -0.000000000000000000, 1.000000000000000000, 0.000000000000000000 ) ) ;
#26998 = CARTESIAN_POINT ( 'NONE',  ( -111.3814931968941693, -292.3987112909525194, -282.3239643039578937 ) ) ;
#26999 = CARTESIAN_POINT ( 'NONE',  ( 35.97879999499883752, -291.3392100398112348, -253.7463668269542723 ) ) ;
#27000 = CARTESIAN_POINT ( 'NONE',  ( 27.34847888445247932, -296.0606773808831349, -308.4115292890044771 ) ) ;
#27001 = CARTESIAN_POINT ( 'NONE',  ( -54.82408830424453328, -286.7632512385069390, -199.1906170051136939 ) ) ;
#27002 = CARTESIAN_POINT ( 'NONE',  ( -0.3392588022769228995, -296.5615698032382284, -335.8041264422155905 ) ) ;
#27003 = CARTESIAN_POINT ( 'NONE',  ( 36.57402137300812939, -277.7193677872832041, -285.0196622779927225 ) ) ;
#27004 = CARTESIAN_POINT ( 'NONE',  ( -37.24350971211693206, -297.2505260664353841, -193.5218439957791361 ) ) ;
#27005 = CARTESIAN_POINT ( 'NONE',  ( -59.51970141286975036, -275.5831750314205237, -340.9735125801483946 ) ) ;
#27006 = CARTESIAN_POINT ( 'NONE',  ( -1.246844991914348721, -278.6148118081109146, -205.2575417990964297 ) ) ;
#27007 = CARTESIAN_POINT ( 'NONE',  ( -40.80897648240764397, -275.2127873590252989, -196.9960161790945961 ) ) ;
#27008 = CARTESIAN_POINT ( 'NONE',  ( 34.17668587304616779, -273.7839170451136965, -243.4589478916424525 ) ) ;
#27009 = CARTESIAN_POINT ( 'NONE',  ( -41.05090993925329457, -296.5249858741252638, -343.8694783810712465 ) ) ;
#27010 = CARTESIAN_POINT ( 'NONE',  ( 200.2296996224750103, 66.43830042146294090, 0.000000000000000000 ) ) ;
#27011 = CARTESIAN_POINT ( 'NONE',  ( -110.3740837728159363, -297.4121711791267444, -266.0168498387822069 ) ) ;
#27012 = CARTESIAN_POINT ( 'NONE',  ( 184.7149167944524493, 8.542400036368780647, 9.000000000000001776 ) ) ;
#27014 = CARTESIAN_POINT ( 'NONE',  ( -89.24067963260355896, -273.1295864742683648, -219.0240365414788641 ) ) ;
#27013 = CARTESIAN_POINT ( 'NONE',  ( 21.71883313833140505, -284.9321556821907961, -223.5403258825938337 ) ) ;
#27015 = CARTESIAN_POINT ( 'NONE',  ( 30.13156083459476164, -287.0704354751360938, -233.1511719122246120 ) ) ;
#27016 = CARTESIAN_POINT ( 'NONE',  ( 0.7051482268294290146, -288.2263178266584873, -337.3405697443773761 ) ) ;
#27017 = CARTESIAN_POINT ( 'NONE',  ( -106.8479408804492152, -298.1521704616210968, -299.6042945670899940 ) ) ;
#27018 = CARTESIAN_POINT ( 'NONE',  ( -17.76481570027202039, -292.7989158339788105, -342.5883567483839443 ) ) ;
#27019 = CARTESIAN_POINT ( 'NONE',  ( 21.47979334249457040, -281.4164219004883307, -319.7998753187028456 ) ) ;
#27020 = CARTESIAN_POINT ( 'NONE',  ( -110.4683760289727132, -287.8380690714490129, -287.0191576251351080 ) ) ;
#27021 = CARTESIAN_POINT ( 'NONE',  ( -23.74566243433469737, -278.2255832233853994, -196.5515232647989308 ) ) ;
#27022 = CARTESIAN_POINT ( 'NONE',  ( -97.68405773378863444, -288.7678176850375280, -312.1675366423921218 ) ) ;
#27023 = CARTESIAN_POINT ( 'NONE',  ( 215.7837434059060229, -147.7221692137691775, 8.778910157967997563 ) ) ;
#27024 = CARTESIAN_POINT ( 'NONE',  ( -98.19591294511941726, -287.9553087231412292, -314.1990631109609353 ) ) ;
#27025 = CARTESIAN_POINT ( 'NONE',  ( -95.93654207537565526, -298.7768366597117051, -225.4731053042661131 ) ) ;
#27026 = CARTESIAN_POINT ( 'NONE',  ( 33.76935068669640572, -282.6185675392887333, -242.2556625177731462 ) ) ;
#27028 = CARTESIAN_POINT ( 'NONE',  ( 34.33424141048760703, -281.3687042817164752, -256.4547656897550496 ) ) ;
#27027 = CARTESIAN_POINT ( 'NONE',  ( -26.47972962276536890, -296.2075940571009482, -195.0095530692215391 ) ) ;
#27029 = CARTESIAN_POINT ( 'NONE',  ( -108.8893852687383088, -297.0814523879359399, -241.7585761403979063 ) ) ;
#27030 = CARTESIAN_POINT ( 'NONE',  ( -91.56891983142160996, -274.6858094713000469, -220.5952624538230111 ) ) ;
#27031 = CARTESIAN_POINT ( 'NONE',  ( 37.65808555574718497, -285.7543958104470221, -279.9648788667705048 ) ) ;
#27032 = CARTESIAN_POINT ( 'NONE',  ( 11.66556568847853548, -282.7326330439566959, -213.5871050624455449 ) ) ;
#27033 = CARTESIAN_POINT ( 'NONE',  ( -90.41092895989248746, -272.1989622165203286, -219.7672380726040160 ) ) ;
#27034 = ORIENTED_EDGE ( 'NONE', *, *, #44915, .F. ) ;
#27035 = DIRECTION ( 'NONE',  ( 0.6421047760857910847, 0.000000000000000000, 0.7666168903225496489 ) ) ;
#27036 = CARTESIAN_POINT ( 'NONE',  ( -110.2773358457840800, -286.7377079611017621, -254.4192920299765888 ) ) ;
#27037 = DIRECTION ( 'NONE',  ( -0.9693563597868447568, -0.2456588035076236187, 0.000000000000000000 ) ) ;
#27038 = CARTESIAN_POINT ( 'NONE',  ( -88.47809603358389552, -282.9094976428776249, -206.1857440867352693 ) ) ;
#27039 = CARTESIAN_POINT ( 'NONE',  ( 18.77827521832830016, -275.4666970422026111, -322.8464224743636350 ) ) ;
#27040 = CARTESIAN_POINT ( 'NONE',  ( -37.52297078781109718, -284.5746206262545570, -344.0667779758421716 ) ) ;
#27041 = CARTESIAN_POINT ( 'NONE',  ( 35.62964301964243674, -277.0072732172582732, -259.2479396345030977 ) ) ;
#27042 = CARTESIAN_POINT ( 'NONE',  ( -70.20015606914390105, -284.9018599522739805, -339.3604527272919427 ) ) ;
#27043 = CARTESIAN_POINT ( 'NONE',  ( -53.79351812100647834, -282.0628097881499912, -341.9429800810540883 ) ) ;
#27044 = CARTESIAN_POINT ( 'NONE',  ( 30.77885051945479944, -283.1388142576619771, -238.8585533059634542 ) ) ;
#27045 = CARTESIAN_POINT ( 'NONE',  ( 21.84949606180241943, -275.0564338273549652, -221.1127444242365243 ) ) ;
#27046 = CARTESIAN_POINT ( 'NONE',  ( 26.14576994433442181, -274.8102008817908199, -226.7677900761915453 ) ) ;
#27047 = EDGE_CURVE ( 'NONE', #6353, #40624, #6428, .T. ) ;
#27048 = CARTESIAN_POINT ( 'NONE',  ( -39.71084415205695706, -297.0022590172003447, -344.7760879756850159 ) ) ;
#27049 = CARTESIAN_POINT ( 'NONE',  ( 133.0872704186301405, -299.5541904835127980, -201.0153591320744226 ) ) ;
#27050 = CARTESIAN_POINT ( 'NONE',  ( 194.5881128153457098, 0.000000000000000000, 21.50000000000000000 ) ) ;
#27051 = CARTESIAN_POINT ( 'NONE',  ( -74.02934795143775659, -293.6733790819649244, -336.7095634250213152 ) ) ;
#27052 = CARTESIAN_POINT ( 'NONE',  ( 26.81779690022809604, -275.5377601327008392, -305.4175059622414210 ) ) ;
#27053 = CARTESIAN_POINT ( 'NONE',  ( -9.264863866584025942, -299.4756024643253909, -193.6652131360563658 ) ) ;
#27054 = CARTESIAN_POINT ( 'NONE',  ( -62.93401431314136829, -287.4746047551155925, -200.8585788520988729 ) ) ;
#27055 = CARTESIAN_POINT ( 'NONE',  ( 25.15799781755510267, -295.6566403369897671, -314.1617265670072925 ) ) ;
#27056 = CARTESIAN_POINT ( 'NONE',  ( 8.679908101217730376, -295.6420228036429307, -331.5985272475140277 ) ) ;
#27057 = CARTESIAN_POINT ( 'NONE',  ( -105.2299404564854797, -292.9668639532366683, -238.8775468937512585 ) ) ;
#27058 = CARTESIAN_POINT ( 'NONE',  ( 16.59809248660833703, -278.8207651292980245, -218.4167715059619468 ) ) ;
#27059 = CARTESIAN_POINT ( 'NONE',  ( -111.4013365498536814, -280.5759484167172104, -262.3498738287158289 ) ) ;
#27060 = CARTESIAN_POINT ( 'NONE',  ( -67.90843236900225577, -293.5363679146383333, -338.2499013958244518 ) ) ;
#27061 = CARTESIAN_POINT ( 'NONE',  ( 1.481871720928115810, -284.3995048165134563, -335.4229020732794879 ) ) ;
#27062 = CARTESIAN_POINT ( 'NONE',  ( -81.65454514863819213, -284.3528263942825447, -211.9607940207285708 ) ) ;
#27063 = CARTESIAN_POINT ( 'NONE',  ( -20.24027634894776284, -109.4294513019383714, -361.8272583522734180 ) ) ;
#27064 = ORIENTED_EDGE ( 'NONE', *, *, #84782, .T. ) ;
#27065 = CARTESIAN_POINT ( 'NONE',  ( -103.5028248555976802, -284.6374363640584306, -239.3415419039653784 ) ) ;
#27066 = ORIENTED_EDGE ( 'NONE', *, *, #84321, .F. ) ;
#27067 = CARTESIAN_POINT ( 'NONE',  ( 37.37321837455115769, -282.4139734262460593, -253.0068341873516431 ) ) ;
#27068 = CARTESIAN_POINT ( 'NONE',  ( -83.20715926477177504, -273.7368716614819277, -213.5416922123357892 ) ) ;
#27069 = CARTESIAN_POINT ( 'NONE',  ( -70.87847623874073122, -284.4144237659661485, -201.4895464261220752 ) ) ;
#27070 = CARTESIAN_POINT ( 'NONE',  ( -56.50952512321615728, -280.7523419835703749, -195.9731500756377898 ) ) ;
#27071 = EDGE_CURVE ( 'NONE', #19834, #62353, #38152, .T. ) ;
#27072 = CARTESIAN_POINT ( 'NONE',  ( -95.60713845284749368, -279.4021525217668795, -319.6544608993764882 ) ) ;
#27073 = CARTESIAN_POINT ( 'NONE',  ( 22.79040588354024166, -281.5607520303948945, -222.4085415732644719 ) ) ;
#27074 = CARTESIAN_POINT ( 'NONE',  ( 30.89617123739170168, -273.2666405000204009, -285.9686137636504668 ) ) ;
#27075 = CARTESIAN_POINT ( 'NONE',  ( 46.06605720673547211, 12.00925050775455105, -332.0840745435668282 ) ) ;
#27076 = ORIENTED_EDGE ( 'NONE', *, *, #29049, .F. ) ;
#27077 = CARTESIAN_POINT ( 'NONE',  ( -31.21436617461464280, -276.1298694289623654, -195.7660872308242688 ) ) ;
#27078 = CARTESIAN_POINT ( 'NONE',  ( 5.081724044709708288, -58.07489044105351184, -354.5077726519059524 ) ) ;
#27079 = CARTESIAN_POINT ( 'NONE',  ( -72.89133565225273514, -277.5987852784263055, -204.7252267440417484 ) ) ;
#27080 = CARTESIAN_POINT ( 'NONE',  ( 20.52401373771774473, -294.6391871028262130, -221.0915450451410891 ) ) ;
#27081 = CARTESIAN_POINT ( 'NONE',  ( -109.2438962974729151, -295.7260717527908582, -283.6201532793220395 ) ) ;
#27082 = CARTESIAN_POINT ( 'NONE',  ( -57.28100147874644676, -288.8102844577184101, -344.7260126453617772 ) ) ;
#27083 = DIRECTION ( 'NONE',  ( -0.000000000000000000, -0.000000000000000000, -1.000000000000000000 ) ) ;
#27085 = CARTESIAN_POINT ( 'NONE',  ( 11.68051854302299297, -285.1456195826879139, -215.1266671553816821 ) ) ;
#27084 = CARTESIAN_POINT ( 'NONE',  ( -66.71484145980906533, -294.0042132043214451, -340.9147396240794592 ) ) ;
#27086 = CARTESIAN_POINT ( 'NONE',  ( -75.63677188178273525, -293.3961697552185228, -206.7058659580672213 ) ) ;
#27087 = CARTESIAN_POINT ( 'NONE',  ( -109.9107325604008878, -286.0206096022957354, -258.6632447618484889 ) ) ;
#27088 = ORIENTED_EDGE ( 'NONE', *, *, #42244, .T. ) ;
#27089 = CARTESIAN_POINT ( 'NONE',  ( -68.24507237474850285, -292.5973546837572599, -200.0772997397733093 ) ) ;
#27090 = CARTESIAN_POINT ( 'NONE',  ( 19.40380042737718824, -282.6953004464953096, -316.4018852143359481 ) ) ;
#27091 = CARTESIAN_POINT ( 'NONE',  ( -99.69428786894694383, -294.7535877865786347, -314.9495132747550201 ) ) ;
#27092 = CARTESIAN_POINT ( 'NONE',  ( -110.6247391956302408, -291.0620713887373654, -293.6380060135784902 ) ) ;
#27093 = CARTESIAN_POINT ( 'NONE',  ( -114.3074426481026507, -291.0695130048759438, -268.3625722094486150 ) ) ;
#27094 = CARTESIAN_POINT ( 'NONE',  ( 28.22869212883852086, -288.1534561859114092, -302.4473091519167838 ) ) ;
#27095 = ORIENTED_EDGE ( 'NONE', *, *, #59092, .F. ) ;
#27096 = CARTESIAN_POINT ( 'NONE',  ( 165.2494399300530290, -11.64849832608277325, -6.403442476110241977 ) ) ;
#27097 = CARTESIAN_POINT ( 'NONE',  ( -58.48355652643064673, -297.1829074632005927, -343.1710502043929409 ) ) ;
#27098 = CARTESIAN_POINT ( 'NONE',  ( -26.28145854419760141, -296.8727291153725787, -193.8566772683458055 ) ) ;
#27099 = EDGE_CURVE ( 'NONE', #55010, #4883, #3359, .T. ) ;
#27100 = CARTESIAN_POINT ( 'NONE',  ( -39.69682902585414297, -279.0806313968635664, -197.1511409979437133 ) ) ;
#27101 = VERTEX_POINT ( 'NONE', #74164 ) ;
#27102 = CARTESIAN_POINT ( 'NONE',  ( 33.65918317144509331, -274.6810417403477231, -240.5856511379769245 ) ) ;
#27103 = AXIS2_PLACEMENT_3D ( 'NONE', #22354, #13874, #72112 ) ;
#27104 = CARTESIAN_POINT ( 'NONE',  ( -101.8118574708835808, -295.5153437075560419, -234.6636872200012647 ) ) ;
#27105 = CARTESIAN_POINT ( 'NONE',  ( 8.359146216502605142, -278.2799001800425458, -328.9270474524835777 ) ) ;
#27106 = CARTESIAN_POINT ( 'NONE',  ( 24.84088220355097221, -273.1392364663823855, -229.8124813281596914 ) ) ;
#27107 = CARTESIAN_POINT ( 'NONE',  ( -86.74598543921285909, -296.9628411107131569, -324.6413823225639703 ) ) ;
#27108 = CARTESIAN_POINT ( 'NONE',  ( -95.00811062789185257, -296.9962205168547484, -315.6249133906281941 ) ) ;
#27109 = DIRECTION ( 'NONE',  ( 0.000000000000000000, 0.000000000000000000, -1.000000000000000000 ) ) ;
#27110 = CARTESIAN_POINT ( 'NONE',  ( -37.66491856410779349, -296.6562215843950980, -346.5733780863321840 ) ) ;
#27111 = CARTESIAN_POINT ( 'NONE',  ( -67.41987226175098158, -295.6585651288866643, -201.4193128339187524 ) ) ;
#27112 = CARTESIAN_POINT ( 'NONE',  ( -41.60706777165610504, -292.6485693250633062, -197.3338131666275785 ) ) ;
#27113 = CARTESIAN_POINT ( 'NONE',  ( -71.34057051661984872, -274.4174295687763561, -201.4536754701578616 ) ) ;
#27114 = CARTESIAN_POINT ( 'NONE',  ( -93.88098888094916106, -289.7900358237721434, -223.2385464290872505 ) ) ;
#27115 = CARTESIAN_POINT ( 'NONE',  ( 207.6175730408114646, 30.32598770090645246, 14.41714557868296076 ) ) ;
#27116 = CARTESIAN_POINT ( 'NONE',  ( -52.53960631940750403, -274.3549741703365044, -194.8842391606416982 ) ) ;
#27117 = CARTESIAN_POINT ( 'NONE',  ( -108.3185624601739931, -296.6584711917766413, -287.5711214357452263 ) ) ;
#27118 = CARTESIAN_POINT ( 'NONE',  ( -73.00984370864296125, -281.5618258474715390, -203.9673435512872288 ) ) ;
#27119 = CARTESIAN_POINT ( 'NONE',  ( 37.77371620120204909, -280.0541586373303744, -255.8362254300273833 ) ) ;
#27120 = EDGE_CURVE ( 'NONE', #93680, #28617, #81263, .T. ) ;
#27121 = CARTESIAN_POINT ( 'NONE',  ( -91.26348299585882273, -277.1428869592384672, -325.2604526235271578 ) ) ;
#27122 = CARTESIAN_POINT ( 'NONE',  ( -33.93048228879852246, -278.4942724223177493, -194.2375079162283669 ) ) ;
#27123 = CARTESIAN_POINT ( 'NONE',  ( -2.506934465997397332, -280.5922660104716897, -336.9686815969719191 ) ) ;
#27124 = CARTESIAN_POINT ( 'NONE',  ( -46.23211325318499121, -272.5118806592818146, -197.3108923092862597 ) ) ;
#27125 = CARTESIAN_POINT ( 'NONE',  ( -51.49900481617321191, -279.2332408641801749, -344.0649843628651183 ) ) ;
#27126 = DIRECTION ( 'NONE',  ( 1.000000000000000000, -0.000000000000000000, 0.000000000000000000 ) ) ;
#27127 = DIRECTION ( 'NONE',  ( 0.000000000000000000, 0.000000000000000000, -1.000000000000000000 ) ) ;
#27128 = CARTESIAN_POINT ( 'NONE',  ( -29.17248944189995541, -296.3929571019469336, -194.3768531707440559 ) ) ;
#27129 = CARTESIAN_POINT ( 'NONE',  ( -11.15325247941416897, -292.3840816982365141, -197.8953764621370226 ) ) ;
#27130 = CARTESIAN_POINT ( 'NONE',  ( 22.08466284731795426, -278.1820719640847415, -316.4095562690440033 ) ) ;
#27131 = CARTESIAN_POINT ( 'NONE',  ( -1.947924874506630433, -272.5208028042094952, -204.2378896559987993 ) ) ;
#27132 = CYLINDRICAL_SURFACE ( 'NONE', #21156, 5.000000000000004441 ) ;
#27133 = CARTESIAN_POINT ( 'NONE',  ( -27.53431744379120261, -284.8487841724237910, -345.3343034640898850 ) ) ;
#27134 = SURFACE_STYLE_USAGE ( .BOTH. , #28090 ) ;
#27135 = CARTESIAN_POINT ( 'NONE',  ( 34.53366031906455902, -285.8284808977682019, -291.8280710323473954 ) ) ;
#27136 = CARTESIAN_POINT ( 'NONE',  ( 175.2296996224750103, 275.5000000000000568, 0.000000000000000000 ) ) ;
#27137 = CARTESIAN_POINT ( 'NONE',  ( 8.464066998315896484, -293.2040172695499223, -327.7758999392900137 ) ) ;
#27138 = CARTESIAN_POINT ( 'NONE',  ( 29.93927130301597472, -285.2751941564156368, -238.9901702644280874 ) ) ;
#27139 = CARTESIAN_POINT ( 'NONE',  ( 160.5350683151633291, 275.0000000000000568, -7.500000000000000000 ) ) ;
#27140 = CARTESIAN_POINT ( 'NONE',  ( -70.63416007385208673, -293.4910443560739282, -337.5668674673837018 ) ) ;
#27141 = CARTESIAN_POINT ( 'NONE',  ( -62.95036322880340407, -284.2045262477641927, -198.4799373703612275 ) ) ;
#27142 = CARTESIAN_POINT ( 'NONE',  ( -107.2086285578391198, -280.4666061661100684, -246.4332172486349180 ) ) ;
#27143 = CARTESIAN_POINT ( 'NONE',  ( 33.48639945661435036, -288.3829295627783722, -241.0440397873470033 ) ) ;
#27144 = CARTESIAN_POINT ( 'NONE',  ( 23.79003188677680569, -279.1842669142483828, -225.2292516735357424 ) ) ;
#27145 = CARTESIAN_POINT ( 'NONE',  ( 35.45189963851188963, -287.6328880002740220, -276.4813352767075116 ) ) ;
#27146 = CARTESIAN_POINT ( 'NONE',  ( -16.77428359631433352, -281.7483690541880605, -199.7045097072040392 ) ) ;
#27147 = CARTESIAN_POINT ( 'NONE',  ( 21.45265491560540383, -281.7455858576137757, -226.7989577140384085 ) ) ;
#27148 = CARTESIAN_POINT ( 'NONE',  ( -0.5419497714532174326, -288.5185094191756434, -204.5878571854532595 ) ) ;
#27149 = ORIENTED_EDGE ( 'NONE', *, *, #69768, .F. ) ;
#27150 = CARTESIAN_POINT ( 'NONE',  ( -60.14606401076753883, -297.5979643126483438, -196.7599576213100363 ) ) ;
#27151 = CARTESIAN_POINT ( 'NONE',  ( -109.3049033929112994, -292.2736117586874798, -290.3792184289671923 ) ) ;
#27152 = DIRECTION ( 'NONE',  ( 0.000000000000000000, 0.000000000000000000, 1.000000000000000000 ) ) ;
#27153 = CARTESIAN_POINT ( 'NONE',  ( 40.64545035920995986, -295.8376638359844719, -252.5284128619064461 ) ) ;
#27154 = EDGE_LOOP ( 'NONE', ( #26142, #22089, #83780, #648 ) ) ;
#27155 = CARTESIAN_POINT ( 'NONE',  ( -82.45883904449129886, -271.4379707684648224, -210.1755097386434272 ) ) ;
#27156 = CARTESIAN_POINT ( 'NONE',  ( 2.197429475817664013, -229.5268262511776527, 25.50000000000000000 ) ) ;
#27157 = CARTESIAN_POINT ( 'NONE',  ( -22.27585476842065759, -293.2621707371192770, -345.0569057958156804 ) ) ;
#27158 = CARTESIAN_POINT ( 'NONE',  ( -103.2934757685224838, -272.3265897374299129, -238.8292934603810522 ) ) ;
#27159 = CARTESIAN_POINT ( 'NONE',  ( -89.13473193361593871, -291.3171703720088885, -322.7842961399212527 ) ) ;
#27160 = CARTESIAN_POINT ( 'NONE',  ( 36.71706668637780524, -283.3245770910309602, -271.3046127958364764 ) ) ;
#27161 = CARTESIAN_POINT ( 'NONE',  ( -40.29765243386989226, -290.5138626856029873, -346.7276762444335532 ) ) ;
#27162 = CARTESIAN_POINT ( 'NONE',  ( -96.89557629440854214, -291.2191001342065988, -318.4092038235149857 ) ) ;
#27163 = CARTESIAN_POINT ( 'NONE',  ( 3.515788104972966899, -288.6018247231436362, -207.4670300057369161 ) ) ;
#27164 = CARTESIAN_POINT ( 'NONE',  ( -82.24057840012150677, -279.6247353396032622, -207.8064160457798550 ) ) ;
#27165 = CARTESIAN_POINT ( 'NONE',  ( 14.47311252195236975, -292.4098536690461287, -325.3569304242728322 ) ) ;
#27166 = CARTESIAN_POINT ( 'NONE',  ( -67.88330470271029071, -283.2754385115422906, -341.0449944645973233 ) ) ;
#27167 = CARTESIAN_POINT ( 'NONE',  ( 24.06091381193657242, -276.8417265180103186, -228.6180145796591319 ) ) ;
#27168 = CARTESIAN_POINT ( 'NONE',  ( -37.30987171927208124, -279.5519495502701375, -340.3611179825599606 ) ) ;
#27169 = VECTOR ( 'NONE', #33906, 1000.000000000000000 ) ;
#27170 = CARTESIAN_POINT ( 'NONE',  ( 12.02900407612087719, -274.6163907632532073, -328.1236281235106276 ) ) ;
#27171 = CYLINDRICAL_SURFACE ( 'NONE', #71185, 5.000000000000004441 ) ;
#27172 = CARTESIAN_POINT ( 'NONE',  ( 34.76328193353419493, -281.2151209592579448, -282.1450054410386201 ) ) ;
#27173 = CARTESIAN_POINT ( 'NONE',  ( -41.34825205859600317, -278.3065845108381495, -346.8723388795421556 ) ) ;
#27174 = CIRCLE ( 'NONE', #18107, 0.5000000000000004441 ) ;
#27175 = CARTESIAN_POINT ( 'NONE',  ( -43.54030390261068106, -275.2875319754132306, -197.0787814104780011 ) ) ;
#27176 = CARTESIAN_POINT ( 'NONE',  ( -111.4907914037313219, -283.8626972706166498, -250.2935761317594086 ) ) ;
#27177 = CARTESIAN_POINT ( 'NONE',  ( -44.41911495301716428, -293.7216902271754861, -196.6354178582184318 ) ) ;
#27178 = CARTESIAN_POINT ( 'NONE',  ( -4.192740137663658828, -276.0819946351367093, -201.7349058634811172 ) ) ;
#27179 = CARTESIAN_POINT ( 'NONE',  ( -76.19680184020130298, -274.8597966351502464, -204.3940593153448333 ) ) ;
#27180 = CARTESIAN_POINT ( 'NONE',  ( 157.4851178187871596, 1.000000000000000444, 8.171572875253808377 ) ) ;
#27181 = CARTESIAN_POINT ( 'NONE',  ( 35.60182152929297672, -275.4376259677823100, -274.3147464286044510 ) ) ;
#27182 = CARTESIAN_POINT ( 'NONE',  ( -109.2274080316977773, -298.8206270627312620, -249.5651225237248525 ) ) ;
#27183 = CARTESIAN_POINT ( 'NONE',  ( -49.69982063282382256, -283.8941529116401625, -196.5024668465094067 ) ) ;
#27184 = CARTESIAN_POINT ( 'NONE',  ( 37.06324037213543221, -292.9711000339918883, -250.5707191875494857 ) ) ;
#27185 = CARTESIAN_POINT ( 'NONE',  ( 37.34412841002156824, -273.5887231500738039, -271.6377031581768051 ) ) ;
#27186 = CARTESIAN_POINT ( 'NONE',  ( 38.29904551428222703, -289.2741106656858960, -280.0015450561255648 ) ) ;
#27187 = CARTESIAN_POINT ( 'NONE',  ( -107.2510278158380004, -289.1792097511361703, -292.5952010055052028 ) ) ;
#27188 = VERTEX_POINT ( 'NONE', #17353 ) ;
#27189 = CARTESIAN_POINT ( 'NONE',  ( -22.29194152094668624, -290.8158412550358207, -195.3931809736681089 ) ) ;
#27190 = CARTESIAN_POINT ( 'NONE',  ( -108.7303444997062769, -290.4213577064709852, -255.0069999143981931 ) ) ;
#27191 = ORIENTED_EDGE ( 'NONE', *, *, #85924, .F. ) ;
#27192 = CARTESIAN_POINT ( 'NONE',  ( 37.52619538189749449, -288.8412901908744743, -287.0431135365123509 ) ) ;
#27193 = CARTESIAN_POINT ( 'NONE',  ( -72.14352144196793404, -279.9115849072436504, -206.1667200956572401 ) ) ;
#27194 = CARTESIAN_POINT ( 'NONE',  ( -37.70138334217815412, -293.9768556387269314, -347.0641895681428650 ) ) ;
#27195 = CARTESIAN_POINT ( 'NONE',  ( -23.81200429218027281, -286.8719398440842951, -194.6084923785239482 ) ) ;
#27196 = EDGE_CURVE ( 'NONE', #4433, #78431, #53314, .T. ) ;
#27197 = CARTESIAN_POINT ( 'NONE',  ( -65.87347006701266139, -286.0222306590572430, -198.8509363197336199 ) ) ;
#27198 = CARTESIAN_POINT ( 'NONE',  ( 1.116050935498282159, -282.8569347567111549, -332.4934169854815877 ) ) ;
#27199 = CARTESIAN_POINT ( 'NONE',  ( -113.8401055986460477, -273.8937930856225194, -270.3782002851730226 ) ) ;
#27200 = CARTESIAN_POINT ( 'NONE',  ( -14.23015497029708598, -91.07820911423134191, -358.7444012829247413 ) ) ;
#27201 = CARTESIAN_POINT ( 'NONE',  ( 159.6170603531574841, 218.6245907200500938, -202.5626340042458082 ) ) ;
#27202 = CARTESIAN_POINT ( 'NONE',  ( 33.74099093003696481, -274.9779143230453542, -287.7301175321651385 ) ) ;
#27203 = CARTESIAN_POINT ( 'NONE',  ( 30.46595282356512868, -274.0990319840454958, -242.3647336413309006 ) ) ;
#27204 = CARTESIAN_POINT ( 'NONE',  ( -111.1581219643938994, -295.7869338039098466, -292.1023643087694381 ) ) ;
#27205 = CARTESIAN_POINT ( 'NONE',  ( -29.53615242528336537, -125.4933017954314209, -361.0433250153028553 ) ) ;
#27206 = CARTESIAN_POINT ( 'NONE',  ( 32.11245255324794812, -273.8224313796083038, -238.1503406651623038 ) ) ;
#27207 = CARTESIAN_POINT ( 'NONE',  ( -110.8952709848931306, -274.4194697368468496, -262.1242358750587300 ) ) ;
#27208 = CARTESIAN_POINT ( 'NONE',  ( -84.03645773215937709, -292.4722694911574763, -213.8471755882974890 ) ) ;
#27209 = ORIENTED_EDGE ( 'NONE', *, *, #52624, .T. ) ;
#27210 = CARTESIAN_POINT ( 'NONE',  ( -114.1305156203026030, -297.4668807950995415, -272.4753099720512068 ) ) ;
#27211 = CARTESIAN_POINT ( 'NONE',  ( 35.33496714404230232, -287.9457882853840829, -262.8717604799663263 ) ) ;
#27212 = CARTESIAN_POINT ( 'NONE',  ( -32.01347938135889848, -295.7894003584659117, -347.0279088065643691 ) ) ;
#27213 = CARTESIAN_POINT ( 'NONE',  ( -97.35549281811060496, -296.3986872176711813, -318.5262453155505114 ) ) ;
#27214 = CARTESIAN_POINT ( 'NONE',  ( 10.92921582374588496, -292.9085720158423101, -215.5312836712909643 ) ) ;
#27215 = ORIENTED_EDGE ( 'NONE', *, *, #89850, .F. ) ;
#27216 = CARTESIAN_POINT ( 'NONE',  ( 32.37527916553901264, -277.0931546752253212, -241.0909381586193092 ) ) ;
#27217 = EDGE_CURVE ( 'NONE', #34864, #58191, #66908, .T. ) ;
#27218 = EDGE_LOOP ( 'NONE', ( #12040, #18317, #12682, #17845 ) ) ;
#27219 = CARTESIAN_POINT ( 'NONE',  ( 36.54238063936777081, -280.7899038512508127, -248.8506603716031975 ) ) ;
#27220 = CARTESIAN_POINT ( 'NONE',  ( -76.47144089843956749, -278.5305240449147846, -332.3261004382662236 ) ) ;
#27221 = CARTESIAN_POINT ( 'NONE',  ( -0.5559044195958554591, -276.2941455033346756, -203.8573833218385118 ) ) ;
#27222 = CARTESIAN_POINT ( 'NONE',  ( -41.32330150027915039, -275.1221310374358495, -345.6239857958984203 ) ) ;
#27223 = CARTESIAN_POINT ( 'NONE',  ( -106.8062448494982135, -297.5072849462307545, -247.4284569389462831 ) ) ;
#27224 = CARTESIAN_POINT ( 'NONE',  ( -96.89586621137789280, -294.5265235765434682, -313.6108207982694580 ) ) ;
#27225 = CARTESIAN_POINT ( 'NONE',  ( 152.5497490326757202, 19.93678331745850585, -10.54177645505017935 ) ) ;
#27226 = CARTESIAN_POINT ( 'NONE',  ( 34.26484624583969918, -281.6857926547419879, -242.0727197365910115 ) ) ;
#27227 = CARTESIAN_POINT ( 'NONE',  ( 11.74927274661883203, -276.5146099098660670, -324.4581901128391337 ) ) ;
#27228 = CARTESIAN_POINT ( 'NONE',  ( 18.00638613757957884, -285.5093948314013801, -217.4653093328933835 ) ) ;
#27229 = CARTESIAN_POINT ( 'NONE',  ( -48.71827311485052547, -299.9079007227234683, -196.0079738450369575 ) ) ;
#27230 = CARTESIAN_POINT ( 'NONE',  ( 82.61707336526248469, -302.0539871969763226, -195.3101965168185075 ) ) ;
#27231 = CARTESIAN_POINT ( 'NONE',  ( 20.47879813962316220, -287.3794791383505185, -315.2076369955311748 ) ) ;
#27232 = CARTESIAN_POINT ( 'NONE',  ( -43.81772289878191629, -278.2091841065776521, -196.5807140211692285 ) ) ;
#27234 = CARTESIAN_POINT ( 'NONE',  ( -103.0536698178278385, -282.1633308060364698, -305.4459008541170988 ) ) ;
#27233 = CARTESIAN_POINT ( 'NONE',  ( -77.12526444794451663, -278.0825939376779274, -208.3920389536815776 ) ) ;
#27236 = CARTESIAN_POINT ( 'NONE',  ( 12.04145225774467320, -288.7384753318011690, -213.8455216671241885 ) ) ;
#27235 = VECTOR ( 'NONE', #29383, 1000.000000000000000 ) ;
#27237 = CARTESIAN_POINT ( 'NONE',  ( 17.74334282199198398, -277.4462668281370838, -318.8854290802125320 ) ) ;
#27238 = CARTESIAN_POINT ( 'NONE',  ( 161.2494399300530290, -11.64849832608277325, 10.00000000000000000 ) ) ;
#27239 = CARTESIAN_POINT ( 'NONE',  ( 0.6640562742306593824, -294.5586054158831075, -205.6445027228300830 ) ) ;
#27240 = CARTESIAN_POINT ( 'NONE',  ( -97.14544960480280622, -276.1570363177626746, -317.2384639609127817 ) ) ;
#27241 = AXIS2_PLACEMENT_3D ( 'NONE', #41305, #92443, #56015 ) ;
#27242 = CARTESIAN_POINT ( 'NONE',  ( 33.99456047768848066, -276.4146899477607917, -286.3877439569877197 ) ) ;
#27243 = CARTESIAN_POINT ( 'NONE',  ( 31.88760362947346039, -283.9355731600895183, -299.7743803571923422 ) ) ;
#27244 = CARTESIAN_POINT ( 'NONE',  ( 156.4851178187871312, 69.18068689461284748, 10.00000000000000000 ) ) ;
#27245 = CARTESIAN_POINT ( 'NONE',  ( -111.9345162805996239, -292.3187177920996760, -282.4120921047509682 ) ) ;
#27246 = MANIFOLD_SOLID_BREP ( 'Fillet17', #12891 ) ;
#27247 = CARTESIAN_POINT ( 'NONE',  ( -71.47367798673904815, -293.5027394604568372, -337.1586007794692819 ) ) ;
#27248 = LINE ( 'NONE', #11629, #81422 ) ;
#27249 = CARTESIAN_POINT ( 'NONE',  ( 9.814248056467786085, -273.4018467065816367, -213.9246120920402063 ) ) ;
#27250 = CARTESIAN_POINT ( 'NONE',  ( 20.31995916252685674, -291.0410855286802416, -223.5863414245100387 ) ) ;
#27251 = CARTESIAN_POINT ( 'NONE',  ( 195.4737936193521648, 39.72103918308751247, 14.98565046456482008 ) ) ;
#27252 = DIRECTION ( 'NONE',  ( -1.000000000000000000, -0.000000000000000000, -0.000000000000000000 ) ) ;
#27253 = CARTESIAN_POINT ( 'NONE',  ( -112.2406604538473687, -289.2170132661147477, -255.7036377136570593 ) ) ;
#27254 = CARTESIAN_POINT ( 'NONE',  ( -107.7429726196183566, -285.8620313682378651, -292.4993484210141901 ) ) ;
#27255 = CARTESIAN_POINT ( 'NONE',  ( 33.09447819934654689, -286.1603862431920788, -299.0093903638906454 ) ) ;
#27256 = CARTESIAN_POINT ( 'NONE',  ( -107.5425581094592786, -285.6872034938801335, -292.4340529031632627 ) ) ;
#27257 = CARTESIAN_POINT ( 'NONE',  ( -93.38537246701778827, -286.0213424944082021, -223.3323127861600597 ) ) ;
#27258 = CARTESIAN_POINT ( 'NONE',  ( -66.40487667731842691, -293.6533666926130195, -200.8360248634611196 ) ) ;
#27259 = CARTESIAN_POINT ( 'NONE',  ( -5.906575967852359277, -274.7219908507835271, -339.0717224811123174 ) ) ;
#27260 = CARTESIAN_POINT ( 'NONE',  ( 5.862923049857116986, -276.8169398349917856, -334.0722224111300420 ) ) ;
#27261 = CARTESIAN_POINT ( 'NONE',  ( -98.71519760985064806, -288.0364577609849448, -314.4583219707833450 ) ) ;
#27262 = CARTESIAN_POINT ( 'NONE',  ( -51.31261788592143347, -277.2260537685583586, -346.0830663000965615 ) ) ;
#27263 = CARTESIAN_POINT ( 'NONE',  ( -102.9001396388044611, -298.0555785965820519, -306.0533833755586670 ) ) ;
#27264 = CARTESIAN_POINT ( 'NONE',  ( -48.18343439339133738, -249.5520599237212593, -481.6766596038578427 ) ) ;
#27265 = CARTESIAN_POINT ( 'NONE',  ( 175.2296996224750103, 250.0000000000000568, 0.000000000000000000 ) ) ;
#27266 = CARTESIAN_POINT ( 'NONE',  ( -108.8414158629337720, -283.4603991874049029, -253.3059686449774972 ) ) ;
#27267 = CARTESIAN_POINT ( 'NONE',  ( -107.7203582892381348, -276.8900631815772613, -244.2913449617409185 ) ) ;
#27268 = CARTESIAN_POINT ( 'NONE',  ( 195.7212220663432163, 20.45996914382524423, -12.49744573203606279 ) ) ;
#27269 = CARTESIAN_POINT ( 'NONE',  ( 36.56237143450444194, -274.2719402145314689, -289.3583799184990539 ) ) ;
#27270 = CARTESIAN_POINT ( 'NONE',  ( -66.85140617073518854, -276.7979650304584425, -337.2421311158539652 ) ) ;
#27271 = CARTESIAN_POINT ( 'NONE',  ( -45.14508731213439319, -296.6727513510831500, -343.6910946173409798 ) ) ;
#27272 = CARTESIAN_POINT ( 'NONE',  ( 12.80049110095817433, -279.6532969102798347, -212.3330802105268447 ) ) ;
#27273 = CARTESIAN_POINT ( 'NONE',  ( -36.98239379526970794, -295.9887657759894068, -343.6079961080988028 ) ) ;
#27274 = CARTESIAN_POINT ( 'NONE',  ( -66.71949139904042170, -296.7442169117479693, -341.0168837673675171 ) ) ;
#27275 = CARTESIAN_POINT ( 'NONE',  ( -90.04439469925162598, -297.1151031139099246, -219.7771372823663114 ) ) ;
#27276 = CARTESIAN_POINT ( 'NONE',  ( -63.52210236830130441, -293.7111094891626522, -200.0789211828130476 ) ) ;
#27277 = CARTESIAN_POINT ( 'NONE',  ( -71.06814580863060371, -285.7859574561193767, -201.1402622648361103 ) ) ;
#27278 = CARTESIAN_POINT ( 'NONE',  ( 35.40663502596412826, -273.4198770511666226, -249.0119162494369220 ) ) ;
#27279 = CARTESIAN_POINT ( 'NONE',  ( 12.41421110037587461, -288.2143355142272867, -329.1263228431822085 ) ) ;
#27280 = CARTESIAN_POINT ( 'NONE',  ( -30.12797466507436539, -282.1236338135403230, -196.0142116669283041 ) ) ;
#27281 = EDGE_CURVE ( 'NONE', #36646, #19844, #8821, .T. ) ;
#27282 = CARTESIAN_POINT ( 'NONE',  ( -105.7805722437432223, -283.9578323582138637, -244.2933365036481632 ) ) ;
#27283 = CARTESIAN_POINT ( 'NONE',  ( -109.9912506668829053, -288.3120511554026848, -289.0416670026615407 ) ) ;
#27284 = CARTESIAN_POINT ( 'NONE',  ( -101.7183354143585632, -264.3591293023451385, -316.7762957234928649 ) ) ;
#27285 = CARTESIAN_POINT ( 'NONE',  ( -52.09524032839020435, -285.3658030966421393, -198.8046962370723918 ) ) ;
#27286 = CARTESIAN_POINT ( 'NONE',  ( 156.0603832538696452, 17.29324094227561304, 10.42473456490728267 ) ) ;
#27287 = CARTESIAN_POINT ( 'NONE',  ( 35.39002270344933976, -282.8054892677800467, -295.0807508349498676 ) ) ;
#27288 = CARTESIAN_POINT ( 'NONE',  ( -99.00839927858632450, -290.2207869571089986, -224.6221640959064700 ) ) ;
#27289 = CARTESIAN_POINT ( 'NONE',  ( -108.9776323251525270, -279.8189887089838521, -296.4909942747548257 ) ) ;
#27290 = CARTESIAN_POINT ( 'NONE',  ( -71.03261470167893776, -280.9319777028852059, -201.6718135009071773 ) ) ;
#27291 = CARTESIAN_POINT ( 'NONE',  ( 17.60345822387882464, -282.0712386883000704, -318.4238850502009655 ) ) ;
#27292 = CARTESIAN_POINT ( 'NONE',  ( 37.70037354433792132, -277.5681354000283250, -271.5930769435605043 ) ) ;
#27293 = CARTESIAN_POINT ( 'NONE',  ( -0.7061756425740647325, -294.5792951268875299, -338.1022046013854379 ) ) ;
#27294 = CARTESIAN_POINT ( 'NONE',  ( -110.8020079200934305, -288.4013858065329714, -283.6061164272788915 ) ) ;
#27295 = CARTESIAN_POINT ( 'NONE',  ( -109.6701288752704357, -295.3154890322894062, -282.3120371511369058 ) ) ;
#27296 = ORIENTED_EDGE ( 'NONE', *, *, #49214, .T. ) ;
#27297 = ORIENTED_EDGE ( 'NONE', *, *, #73162, .F. ) ;
#27298 = CARTESIAN_POINT ( 'NONE',  ( 23.78085754748449077, -284.0530328643782809, -312.8504947958872435 ) ) ;
#27299 = CARTESIAN_POINT ( 'NONE',  ( -106.0085204806748322, -295.8863136437994967, -295.3484049681551369 ) ) ;
#27300 = CARTESIAN_POINT ( 'NONE',  ( 38.91721238381406778, -294.5236544807613086, -261.7469259622861273 ) ) ;
#27301 = CARTESIAN_POINT ( 'NONE',  ( -66.59275217290401372, -284.0971014425639964, -337.3692488707681605 ) ) ;
#27302 = CARTESIAN_POINT ( 'NONE',  ( 36.36333780702232588, -274.3388925976531141, -248.7186136124020095 ) ) ;
#27303 = CARTESIAN_POINT ( 'NONE',  ( -108.2763090439945017, -291.5817165116959586, -240.6694685799345450 ) ) ;
#27304 = CARTESIAN_POINT ( 'NONE',  ( -65.39758372173835710, -283.8288876396491673, -199.9684111732740632 ) ) ;
#27305 = AXIS2_PLACEMENT_3D ( 'NONE', #75038, #46592, #24842 ) ;
#27306 = CARTESIAN_POINT ( 'NONE',  ( -85.14822228928255754, -290.0247389172650401, -330.7638640423928109 ) ) ;
#27307 = CARTESIAN_POINT ( 'NONE',  ( 30.50640403082802266, -288.2481497407778761, -297.4923682335670492 ) ) ;
#27308 = LINE ( 'NONE', #70418, #6653 ) ;
#27309 = CARTESIAN_POINT ( 'NONE',  ( 183.0442525570908288, 300.2961574867697436, -4.888549259831427740 ) ) ;
#27310 = CARTESIAN_POINT ( 'NONE',  ( 167.4109119493085700, 229.8605661533808870, -189.8721647499563687 ) ) ;
#27311 = VECTOR ( 'NONE', #37606, 1000.000000000000000 ) ;
#27312 = CARTESIAN_POINT ( 'NONE',  ( -21.84768608329982342, -284.3771770459457571, -345.0782062535183741 ) ) ;
#27313 = CARTESIAN_POINT ( 'NONE',  ( -4.829096099716524648, -280.1237833571632336, -337.9475929042657754 ) ) ;
#27314 = VERTEX_POINT ( 'NONE', #16871 ) ;
#27315 = CARTESIAN_POINT ( 'NONE',  ( 30.61595329125420761, -280.8391301712606491, -297.8562705483535638 ) ) ;
#27316 = CARTESIAN_POINT ( 'NONE',  ( 12.68765748498152668, -276.0430211412867152, -328.8658841838119429 ) ) ;
#27317 = CARTESIAN_POINT ( 'NONE',  ( -95.87140642681021063, -279.9096711071192090, -317.0109887043710160 ) ) ;
#27318 = CARTESIAN_POINT ( 'NONE',  ( 194.9847507448477586, 275.9312710741783690, -124.5726050330940495 ) ) ;
#27319 = CARTESIAN_POINT ( 'NONE',  ( 16.81837667705199024, -279.3792732367631970, -216.3861421213827896 ) ) ;
#27320 = CARTESIAN_POINT ( 'NONE',  ( -86.79746320437757845, -283.3808451009110172, -214.3816419668695801 ) ) ;
#27321 = CARTESIAN_POINT ( 'NONE',  ( -93.88237814915559909, -297.6140871058700554, -321.1458961067387463 ) ) ;
#27322 = CARTESIAN_POINT ( 'NONE',  ( 14.36425850722171305, -294.7935999725800116, -322.0508823860793655 ) ) ;
#27323 = EDGE_LOOP ( 'NONE', ( #46817, #53388, #8560, #65884 ) ) ;
#27324 = CARTESIAN_POINT ( 'NONE',  ( -103.2953156199358773, -288.8005705447496894, -302.7858628561513683 ) ) ;
#27325 = CARTESIAN_POINT ( 'NONE',  ( -31.27638830350270993, -274.7782450094238129, -193.6893597177242725 ) ) ;
#27326 = CARTESIAN_POINT ( 'NONE',  ( -63.30672211539041427, -273.7042447018218922, -202.1214005255021391 ) ) ;
#27327 = ORIENTED_EDGE ( 'NONE', *, *, #69069, .T. ) ;
#27328 = CARTESIAN_POINT ( 'NONE',  ( -0.1831253113849828362, -273.4547914905875245, -203.2586824619305332 ) ) ;
#27329 = DIRECTION ( 'NONE',  ( -1.000000000000000000, 0.000000000000000000, 0.000000000000000000 ) ) ;
#27330 = CARTESIAN_POINT ( 'NONE',  ( 197.4836817735085219, 42.27872732282707346, 11.66666666666666785 ) ) ;
#27331 = CARTESIAN_POINT ( 'NONE',  ( 199.0143093133015100, 17.19615242270663202, 9.000000000000001776 ) ) ;
#27332 = CARTESIAN_POINT ( 'NONE',  ( 24.39816595799696941, -283.1774308882137916, -309.9818599623097839 ) ) ;
#27333 = CARTESIAN_POINT ( 'NONE',  ( -92.35579478825694366, -281.0391018675192640, -217.8700442863209901 ) ) ;
#27334 = CARTESIAN_POINT ( 'NONE',  ( -109.8434773210250626, -283.7468500849336692, -260.0218359929064604 ) ) ;
#27335 = CARTESIAN_POINT ( 'NONE',  ( -30.16618188883983009, -282.0041768253495320, -196.4223111558342225 ) ) ;
#27336 = CARTESIAN_POINT ( 'NONE',  ( -11.02434954015732949, -275.1826137930383993, -339.1950108740455789 ) ) ;
#27337 = CARTESIAN_POINT ( 'NONE',  ( 208.0212563688061209, 27.56882951438707607, 14.33494424848942295 ) ) ;
#27338 = DIRECTION ( 'NONE',  ( 0.000000000000000000, 0.000000000000000000, 1.000000000000000000 ) ) ;
#27339 = CARTESIAN_POINT ( 'NONE',  ( -91.20852860431287468, -278.5968984351251265, -325.2309066167078981 ) ) ;
#27340 = EDGE_CURVE ( 'NONE', #86290, #16610, #41184, .T. ) ;
#27341 = ORIENTED_EDGE ( 'NONE', *, *, #86916, .T. ) ;
#27342 = ORIENTED_EDGE ( 'NONE', *, *, #87285, .F. ) ;
#27343 = CARTESIAN_POINT ( 'NONE',  ( -37.28952445085584344, -285.0313527085119745, -345.7290907686743822 ) ) ;
#27344 = CARTESIAN_POINT ( 'NONE',  ( -3.552610916742571234, -291.7073486354183842, -205.4696765001656615 ) ) ;
#27345 = EDGE_CURVE ( 'NONE', #72125, #79604, #45719, .T. ) ;
#27346 = CARTESIAN_POINT ( 'NONE',  ( -60.00515845156854766, -288.6869560250977997, -343.8436359249863017 ) ) ;
#27347 = CARTESIAN_POINT ( 'NONE',  ( -74.03885036147005394, -283.7973853105481794, -206.0712863698774697 ) ) ;
#27349 = CARTESIAN_POINT ( 'NONE',  ( -91.34730427840381140, -288.0730640359070094, -321.0459539607400075 ) ) ;
#27348 = CARTESIAN_POINT ( 'NONE',  ( -98.58748373413178001, -283.6886951472571923, -229.5649305666050566 ) ) ;
#27350 = CARTESIAN_POINT ( 'NONE',  ( -71.58058375418737285, -284.7202224335170513, -335.2828351021660183 ) ) ;
#27351 = CARTESIAN_POINT ( 'NONE',  ( 36.21573023247668033, -273.7399587408131083, -285.0002808901811591 ) ) ;
#27352 = CARTESIAN_POINT ( 'NONE',  ( 36.60546808372873784, -285.7195202817657105, -251.9693608252536876 ) ) ;
#27353 = CARTESIAN_POINT ( 'NONE',  ( -111.6245334400059050, -298.6863644333126899, -259.9209482428871638 ) ) ;
#27354 = CARTESIAN_POINT ( 'NONE',  ( -77.52046640878283768, -283.5141286249710220, -206.8339964871320831 ) ) ;
#27355 = CARTESIAN_POINT ( 'NONE',  ( 15.42060562452119399, -281.7617032878529812, -219.4994397253662441 ) ) ;
#27356 = CARTESIAN_POINT ( 'NONE',  ( 33.12643481780811072, -289.2135120760518703, -244.2025556733286749 ) ) ;
#27357 = CARTESIAN_POINT ( 'NONE',  ( 193.5407199155270064, 275.7877658745666167, 16.89624193776961647 ) ) ;
#27358 = CARTESIAN_POINT ( 'NONE',  ( 206.7809450508160865, 35.77530089738193908, 15.00000000000000000 ) ) ;
#27359 = CARTESIAN_POINT ( 'NONE',  ( -0.1466359448418213252, -296.4815763022608053, -336.1471449682514390 ) ) ;
#27360 = CARTESIAN_POINT ( 'NONE',  ( -94.60106717679414601, -277.2222716827536146, -221.9020741588640249 ) ) ;
#27361 = CARTESIAN_POINT ( 'NONE',  ( -112.1577026689060972, -289.9688221063344713, -252.8475636552739445 ) ) ;
#27362 = CARTESIAN_POINT ( 'NONE',  ( 8.711667836346627780, -292.8090281831858306, -328.0941692137078576 ) ) ;
#27363 = CARTESIAN_POINT ( 'NONE',  ( -16.76772230498805882, -279.0083639460441418, -199.8064943679413545 ) ) ;
#27364 = CARTESIAN_POINT ( 'NONE',  ( -111.0041586080609335, -270.7753642946829586, -259.2785438180432607 ) ) ;
#27365 = CARTESIAN_POINT ( 'NONE',  ( 4.772621072075070359, -293.9490609137965862, -210.0689550756791562 ) ) ;
#27366 = CARTESIAN_POINT ( 'NONE',  ( -69.85430415644619018, -297.9805209788416391, -337.9475929042657754 ) ) ;
#27367 = CARTESIAN_POINT ( 'NONE',  ( -91.13293395096499694, -295.7842898866273913, -216.2389329227558505 ) ) ;
#27368 = CARTESIAN_POINT ( 'NONE',  ( -50.87842608446878501, -290.8279796968201936, -342.9612582092462389 ) ) ;
#27369 = CARTESIAN_POINT ( 'NONE',  ( 14.75988629442987765, -291.0134833856989189, -214.9770199582285670 ) ) ;
#27370 = CARTESIAN_POINT ( 'NONE',  ( -107.1358418708726390, -292.2847520119598244, -247.0340372542501939 ) ) ;
#27371 = CARTESIAN_POINT ( 'NONE',  ( 196.7510731661265595, -143.7221692137691775, 21.50000000000000000 ) ) ;
#27372 = CARTESIAN_POINT ( 'NONE',  ( -108.8705926296952384, -291.5572875698862276, -254.9916916755754528 ) ) ;
#27373 = CARTESIAN_POINT ( 'NONE',  ( -74.94434090351494149, -282.8906705383787994, 54.50000000000000711 ) ) ;
#27374 = CARTESIAN_POINT ( 'NONE',  ( -108.4242666544780036, -291.3929707092885337, -298.9141818055691715 ) ) ;
#27376 = CARTESIAN_POINT ( 'NONE',  ( 23.34124622615589217, -292.9886269204886275, -229.7830448177489302 ) ) ;
#27375 = CARTESIAN_POINT ( 'NONE',  ( 37.97503265957070795, -279.6030249995276336, -272.7687230323354015 ) ) ;
#27377 = CARTESIAN_POINT ( 'NONE',  ( -41.00839511846569962, -280.0072384461698221, -193.4352749524908859 ) ) ;
#27378 = AXIS2_PLACEMENT_3D ( 'NONE', #23323, #2008, #67355 ) ;
#27379 = CARTESIAN_POINT ( 'NONE',  ( -31.64208975497111709, -282.6488075958485524, -347.1419453093952256 ) ) ;
#27380 = CARTESIAN_POINT ( 'NONE',  ( -69.57004763612914644, -287.4772168838541688, -337.8989743899766722 ) ) ;
#27381 = CARTESIAN_POINT ( 'NONE',  ( 28.89402431627868495, -279.2428427415923124, -236.7255172946338178 ) ) ;
#27382 = CARTESIAN_POINT ( 'NONE',  ( -15.95863829356263963, -284.3283997290398020, -198.4199873560102674 ) ) ;
#27383 = CARTESIAN_POINT ( 'NONE',  ( 25.71866934945004601, -279.4591717714094443, -227.3026520576797793 ) ) ;
#27384 = CARTESIAN_POINT ( 'NONE',  ( -26.65054086944309830, -285.1053071215373507, -194.3658049844564459 ) ) ;
#27385 = CARTESIAN_POINT ( 'NONE',  ( 165.2494399300530290, 8.542400036368780647, -9.000000000000001776 ) ) ;
#27386 = CARTESIAN_POINT ( 'NONE',  ( 11.44455111512501588, -294.3417896529086875, -214.9183819441529693 ) ) ;
#27387 = CARTESIAN_POINT ( 'NONE',  ( 25.64846991934734177, -276.4018962778529271, -227.0846712990225171 ) ) ;
#27388 = CARTESIAN_POINT ( 'NONE',  ( -109.3076459926786583, -278.0547752691741721, -282.8039674619773791 ) ) ;
#27389 = CARTESIAN_POINT ( 'NONE',  ( -107.7305083301197755, -290.3190013718808018, -301.7078813829190835 ) ) ;
#27390 = CARTESIAN_POINT ( 'NONE',  ( -83.03226933975948043, -281.7513958574232902, -330.6073059821854372 ) ) ;
#27391 = CARTESIAN_POINT ( 'NONE',  ( -108.3336134309491001, -289.8481472968634876, -252.3224674822463385 ) ) ;
#27392 = CARTESIAN_POINT ( 'NONE',  ( -91.27690388316308656, -293.8190723161891356, -322.4763215629811270 ) ) ;
#27393 = ORIENTED_EDGE ( 'NONE', *, *, #16696, .F. ) ;
#27394 = FACE_OUTER_BOUND ( 'NONE', #14380, .T. ) ;
#27395 = CARTESIAN_POINT ( 'NONE',  ( -30.79522088293225579, -291.6447872699930031, -197.5934599801285003 ) ) ;
#27396 = CARTESIAN_POINT ( 'NONE',  ( 207.7755975652984830, 28.53818587417392294, 11.99999999999999822 ) ) ;
#27397 = CARTESIAN_POINT ( 'NONE',  ( -102.0172624299487154, -270.4809262143062369, -239.1787733560258289 ) ) ;
#27398 = CARTESIAN_POINT ( 'NONE',  ( -113.5397675098091952, -295.7276931348159792, -261.0511910224050212 ) ) ;
#27399 = CARTESIAN_POINT ( 'NONE',  ( 38.40674090728612811, -279.6507178174103387, -267.1340045153355049 ) ) ;
#27400 = EDGE_CURVE ( 'NONE', #21372, #60748, #75370, .T. ) ;
#27401 = ADVANCED_FACE ( 'NONE', ( #82659 ), #52386, .F. ) ;
#27402 = CARTESIAN_POINT ( 'NONE',  ( -113.8342913009046100, -285.9077191078187639, -267.1519065369233203 ) ) ;
#27403 = CARTESIAN_POINT ( 'NONE',  ( 35.68042508330538709, -287.3584737447801558, -268.3145776192525318 ) ) ;
#27404 = CARTESIAN_POINT ( 'NONE',  ( 17.05590036306628221, -277.7788697772809883, -320.0952223965823578 ) ) ;
#27405 = CARTESIAN_POINT ( 'NONE',  ( -110.5017418172639907, -294.3803226888189783, -285.2388935552942257 ) ) ;
#27406 = CARTESIAN_POINT ( 'NONE',  ( -109.7754286480210624, -298.5109648063378813, -255.0905864607733236 ) ) ;
#27407 = CARTESIAN_POINT ( 'NONE',  ( -81.06816903332166646, -276.4562322859036385, -329.3113208726173866 ) ) ;
#27408 = ORIENTED_EDGE ( 'NONE', *, *, #45253, .T. ) ;
#27409 = CARTESIAN_POINT ( 'NONE',  ( 204.6539576904058606, 296.7472757692770529, 7.500000000000000000 ) ) ;
#27410 = CARTESIAN_POINT ( 'NONE',  ( -104.5865021315797350, -295.7317590908977536, -307.9384961836782963 ) ) ;
#27411 = CARTESIAN_POINT ( 'NONE',  ( 35.94357302915922503, -289.6412678093057025, -283.4218583100583260 ) ) ;
#27412 = CARTESIAN_POINT ( 'NONE',  ( 198.8852758280200419, 66.55360856414498016, -4.692040283682947788 ) ) ;
#27413 = CARTESIAN_POINT ( 'NONE',  ( 33.80220212180334016, -288.4249677313915754, -287.1670050828029161 ) ) ;
#27414 = VERTEX_POINT ( 'NONE', #1272 ) ;
#27415 = CARTESIAN_POINT ( 'NONE',  ( 3.706313439029678580, -279.6484947560007868, -205.4301429641734842 ) ) ;
#27416 = CARTESIAN_POINT ( 'NONE',  ( -112.7902900871879126, -297.3905032902615062, -255.4332481503423935 ) ) ;
#27417 = CARTESIAN_POINT ( 'NONE',  ( -63.93273379948281843, -289.8487573486725069, -199.3606468122460740 ) ) ;
#27418 = CARTESIAN_POINT ( 'NONE',  ( -96.49244601821297351, -296.2224108746394791, -319.6455300220125082 ) ) ;
#27419 = CARTESIAN_POINT ( 'NONE',  ( 34.50321368042285286, -293.7123695142064435, -257.2380349024562065 ) ) ;
#27420 = FACE_OUTER_BOUND ( 'NONE', #6484, .T. ) ;
#27421 =( LENGTH_UNIT ( ) NAMED_UNIT ( * ) SI_UNIT ( .MILLI., .METRE. ) );
#27422 = DIRECTION ( 'NONE',  ( -0.000000000000000000, 0.000000000000000000, -1.000000000000000000 ) ) ;
#27423 = CARTESIAN_POINT ( 'NONE',  ( 2.831726135935097144, -290.0439901617301643, -335.2984042817187742 ) ) ;
#27424 = CARTESIAN_POINT ( 'NONE',  ( -19.05039376806008633, -285.3376638359844719, -350.3538533559490702 ) ) ;
#27425 = ORIENTED_EDGE ( 'NONE', *, *, #46545, .T. ) ;
#27426 = CARTESIAN_POINT ( 'NONE',  ( 32.29655335312978792, -281.3203502777394647, -303.1028937768278979 ) ) ;
#27427 = CARTESIAN_POINT ( 'NONE',  ( -37.51993876966864860, -285.0545814136198715, -345.2069844629641580 ) ) ;
#27428 = CARTESIAN_POINT ( 'NONE',  ( 38.76950216745545674, -286.0345140429583921, -263.0319716620259669 ) ) ;
#27429 = CARTESIAN_POINT ( 'NONE',  ( -106.0223964171046873, -289.0112535863611356, -241.5168748522592637 ) ) ;
#27430 = CARTESIAN_POINT ( 'NONE',  ( 36.73266420422341838, -277.2094972349934210, -254.3846594581450802 ) ) ;
#27431 = EDGE_LOOP ( 'NONE', ( #62243, #68209, #41368, #61536, #67965, #48827, #55810, #22779, #11314, #41330, #42104, #91102, #5549, #4851, #7613 ) ) ;
#27433 = CARTESIAN_POINT ( 'NONE',  ( 4.988920407950307556, -279.9900585380363509, -210.7623660415267750 ) ) ;
#27432 = CARTESIAN_POINT ( 'NONE',  ( -78.63200210439875093, -277.6252152258310275, -330.6232601250132461 ) ) ;
#27434 = CARTESIAN_POINT ( 'NONE',  ( 39.07366994782440628, -276.7133764994251806, -276.8560179275592645 ) ) ;
#27435 = CARTESIAN_POINT ( 'NONE',  ( -68.49690627285440314, -278.4467592661184767, -200.3656544439373590 ) ) ;
#27436 = CARTESIAN_POINT ( 'NONE',  ( -64.69487635908569700, -181.8657373906415273, -359.8890228527233148 ) ) ;
#27437 = CARTESIAN_POINT ( 'NONE',  ( -85.66942062355305154, -274.3430498377096001, -210.7184181443548709 ) ) ;
#27438 = CARTESIAN_POINT ( 'NONE',  ( -62.66699936075727351, -299.1541419330542340, -198.2692633043302521 ) ) ;
#27439 = CARTESIAN_POINT ( 'NONE',  ( -106.6379572354042296, -292.6233781216987495, -303.7686719486574702 ) ) ;
#27440 = CARTESIAN_POINT ( 'NONE',  ( 82.65368334098262437, -299.1786464277133177, -192.8837611238190277 ) ) ;
#27441 = AXIS2_PLACEMENT_3D ( 'NONE', #44395, #2262, #44852 ) ;
#27442 = CARTESIAN_POINT ( 'NONE',  ( 35.43272459205206104, -288.7479241839253064, -279.1990577936966247 ) ) ;
#27443 = CARTESIAN_POINT ( 'NONE',  ( 38.34317685933614683, -289.2194144009057482, -263.0324034710992009 ) ) ;
#27444 = CARTESIAN_POINT ( 'NONE',  ( 35.09830811078096247, -286.7665630169072415, -260.1758885920074817 ) ) ;
#27445 = CARTESIAN_POINT ( 'NONE',  ( -112.2983557409630606, -284.2769706189415047, -253.0109974377302535 ) ) ;
#27446 = CARTESIAN_POINT ( 'NONE',  ( -72.49300536962913100, -277.9784877313607581, -205.4702391460896820 ) ) ;
#27447 = CARTESIAN_POINT ( 'NONE',  ( 16.86041374672074156, -288.6947358634152465, -219.6176547815807112 ) ) ;
#27448 = CARTESIAN_POINT ( 'NONE',  ( 3.100503244290429894, -279.0856411858003980, -208.6952022770793178 ) ) ;
#27449 = CARTESIAN_POINT ( 'NONE',  ( -85.41525797936425590, -279.0479800624798941, -326.0178727197855437 ) ) ;
#27450 = CARTESIAN_POINT ( 'NONE',  ( -11.22619375635359162, -277.1947582623361654, -338.5957775671961940 ) ) ;
#27451 = CARTESIAN_POINT ( 'NONE',  ( -70.48125557083621118, -288.2742195928282740, -339.4391138334882498 ) ) ;
#27452 = CARTESIAN_POINT ( 'NONE',  ( -85.99222072904312597, -284.5098016705559303, -329.8362023898341135 ) ) ;
#27453 = CARTESIAN_POINT ( 'NONE',  ( -110.1644125489615789, -284.7314306668059203, -295.1881085137200103 ) ) ;
#27454 = CARTESIAN_POINT ( 'NONE',  ( 34.48583090488907033, -281.8916569509727310, -283.4621278111322340 ) ) ;
#27455 = ORIENTED_EDGE ( 'NONE', *, *, #54344, .T. ) ;
#27456 = EDGE_LOOP ( 'NONE', ( #13127, #57449 ) ) ;
#27457 = CARTESIAN_POINT ( 'NONE',  ( 151.9709352735115147, -297.1570670221753971, -195.3611179825600175 ) ) ;
#27458 = CARTESIAN_POINT ( 'NONE',  ( -113.1338198747053241, -292.4373615970634432, -268.4105386301732210 ) ) ;
#27459 = CARTESIAN_POINT ( 'NONE',  ( -44.83198890635473077, -290.6441824661231976, -194.1692292640431106 ) ) ;
#27460 = CARTESIAN_POINT ( 'NONE',  ( -87.48570583729120642, -272.3906995855119249, -216.9157923600974698 ) ) ;
#27461 = CARTESIAN_POINT ( 'NONE',  ( 39.13477531981056501, -293.0075702591530558, -278.8918126578204237 ) ) ;
#27462 = CARTESIAN_POINT ( 'NONE',  ( -34.57114541367115379, -287.4967241094559540, -344.0524085595006909 ) ) ;
#27463 = CARTESIAN_POINT ( 'NONE',  ( -4.361680243343561081, -290.7327275512591882, -204.0877174320054337 ) ) ;
#27464 = CARTESIAN_POINT ( 'NONE',  ( -29.11345369632673297, -290.1506324523894591, -343.2955163495398665 ) ) ;
#27465 = DIRECTION ( 'NONE',  ( -1.000000000000000000, 0.000000000000000000, -0.000000000000000000 ) ) ;
#27466 = CARTESIAN_POINT ( 'NONE',  ( -104.7056410641375663, -292.1162448231181088, -303.4502878716615442 ) ) ;
#27467 = CARTESIAN_POINT ( 'NONE',  ( -110.8417835582008593, -288.7543947888402727, -254.5599007528447260 ) ) ;
#27468 = CARTESIAN_POINT ( 'NONE',  ( -85.66443643068748770, -293.3840823987449653, -212.9363270392000231 ) ) ;
#27469 = CARTESIAN_POINT ( 'NONE',  ( -68.88711278083134459, -286.5681490517861221, -204.2542014814545155 ) ) ;
#27470 = CARTESIAN_POINT ( 'NONE',  ( 20.77518091916995147, -294.8965061037041551, -222.6908277792020954 ) ) ;
#27471 = CARTESIAN_POINT ( 'NONE',  ( 199.9390245229519110, 68.58287003106127599, -4.389327654518210942 ) ) ;
#27472 = DIRECTION ( 'NONE',  ( 0.000000000000000000, 0.000000000000000000, 1.000000000000000000 ) ) ;
#27473 = CARTESIAN_POINT ( 'NONE',  ( -8.347270493903321764, -276.4096228299575841, -200.7519482697563262 ) ) ;
#27474 = EDGE_CURVE ( 'NONE', #45702, #59451, #26784, .T. ) ;
#27475 = CARTESIAN_POINT ( 'NONE',  ( -112.9783591683269748, -295.9189796037368296, -256.8239605997793547 ) ) ;
#27476 = CARTESIAN_POINT ( 'NONE',  ( 16.19506163846669367, -273.0642784632775601, -219.1812377889535526 ) ) ;
#27477 = CARTESIAN_POINT ( 'NONE',  ( -111.6068375098344916, -276.5568804823640221, -276.1673229430492142 ) ) ;
#27478 = CARTESIAN_POINT ( 'NONE',  ( -67.23319308046851006, -274.8563432785620080, -203.3128119753083354 ) ) ;
#27479 = CARTESIAN_POINT ( 'NONE',  ( -7.900697975683619312, -273.0050082660452517, -199.7937159872668360 ) ) ;
#27480 = CARTESIAN_POINT ( 'NONE',  ( -97.65599281484479377, -297.3942267175535790, -312.5222495544011281 ) ) ;
#27481 = DIRECTION ( 'NONE',  ( -0.9510565162951498674, 0.000000000000000000, 0.3090169943749591086 ) ) ;
#27482 = CARTESIAN_POINT ( 'NONE',  ( -101.3607911697761068, -297.8379242799479698, -234.9470288552004149 ) ) ;
#27483 = CARTESIAN_POINT ( 'NONE',  ( 159.4851178187871312, 0.000000000000000000, 10.00000000000000000 ) ) ;
#27485 = CARTESIAN_POINT ( 'NONE',  ( -110.3417001280813707, -272.3854989502048056, -270.3590007205843904 ) ) ;
#27484 = CARTESIAN_POINT ( 'NONE',  ( 13.16359611347443348, -284.7735701835686086, -214.3659444510310266 ) ) ;
#27486 = CARTESIAN_POINT ( 'NONE',  ( -85.15486556093594572, -289.3582838214090884, -330.7586053970208582 ) ) ;
#27487 = CARTESIAN_POINT ( 'NONE',  ( -97.78847990832565529, -299.1437673785420088, -225.3440886167354904 ) ) ;
#27488 = CARTESIAN_POINT ( 'NONE',  ( 34.08938311030586732, -291.8403679688487955, -292.6687125254013608 ) ) ;
#27489 = CARTESIAN_POINT ( 'NONE',  ( 36.83182285110126486, -280.4970021625206869, -250.2501067776279911 ) ) ;
#27490 = CARTESIAN_POINT ( 'NONE',  ( 10.59707575819633618, -285.9094976428776249, -330.5268031993606428 ) ) ;
#27491 = PLANE ( 'NONE',  #21225 ) ;
#27492 = CARTESIAN_POINT ( 'NONE',  ( 6.067174800044488947, -287.2435990869718125, -329.6089059913525716 ) ) ;
#27493 = CARTESIAN_POINT ( 'NONE',  ( 157.4851178187871312, 15.00000000000000000, 7.000000000000000888 ) ) ;
#27494 = CARTESIAN_POINT ( 'NONE',  ( -83.80469963662763178, -287.6899482727729946, -329.2354784656934044 ) ) ;
#27495 = CARTESIAN_POINT ( 'NONE',  ( -111.0350334602965603, -274.0720295093142909, -270.3804279068866663 ) ) ;
#27496 = CARTESIAN_POINT ( 'NONE',  ( 21.50522250096071986, -282.3171204041229885, -221.6205189710047705 ) ) ;
#27498 = CARTESIAN_POINT ( 'NONE',  ( 11.91668871776623639, -282.3443829044886684, -324.2370043169051996 ) ) ;
#27497 = CARTESIAN_POINT ( 'NONE',  ( -110.0286478122418146, -294.8288559109639095, -250.2935782761344115 ) ) ;
#27499 = CARTESIAN_POINT ( 'NONE',  ( -111.6226369167017367, -296.9750813353718399, -249.8824974785207473 ) ) ;
#27500 = CARTESIAN_POINT ( 'NONE',  ( -73.20103158731048154, -299.0875970637274577, -205.9808717845649255 ) ) ;
#27501 = CARTESIAN_POINT ( 'NONE',  ( 5.032736954301892496, -282.6251541127557516, -208.4789094859022498 ) ) ;
#27502 = CARTESIAN_POINT ( 'NONE',  ( -49.98278955158966852, -296.9456245938511074, -198.2250569196252741 ) ) ;
#27503 = EDGE_CURVE ( 'NONE', #32344, #93231, #3602, .T. ) ;
#27504 = CIRCLE ( 'NONE', #71382, 2.000000000000000000 ) ;
#27505 = EDGE_LOOP ( 'NONE', ( #83633, #29187, #57722, #52742 ) ) ;
#27506 = CARTESIAN_POINT ( 'NONE',  ( 143.6449502718966755, 0.000000000000000000, 21.50000000000000000 ) ) ;
#27508 = CARTESIAN_POINT ( 'NONE',  ( -92.87216662424697233, -285.8336180713416184, -320.2623451598472570 ) ) ;
#27507 = AXIS2_PLACEMENT_3D ( 'NONE', #45493, #51226, #38410 ) ;
#27509 = CARTESIAN_POINT ( 'NONE',  ( 143.6449502718966755, -26.00396092263537895, 22.08578643762690419 ) ) ;
#27510 = CARTESIAN_POINT ( 'NONE',  ( -106.6379572354042296, -288.4809262143061801, -236.9535640164627353 ) ) ;
#27511 = CARTESIAN_POINT ( 'NONE',  ( 36.33571411541639407, -275.0240808073210701, -292.2203004953053096 ) ) ;
#27512 = EDGE_CURVE ( 'NONE', #4350, #25794, #33404, .T. ) ;
#27513 = EDGE_CURVE ( 'NONE', #21234, #61209, #42707, .T. ) ;
#27514 = CARTESIAN_POINT ( 'NONE',  ( -30.80485956688695026, -291.9704018938274999, -197.6543801931254905 ) ) ;
#27515 = CIRCLE ( 'NONE', #45597, 0.4999999999999991673 ) ;
#27516 = CARTESIAN_POINT ( 'NONE',  ( 34.62162197104575512, -283.2797118954034090, -286.2352487337064986 ) ) ;
#27517 = CARTESIAN_POINT ( 'NONE',  ( 33.62370734642519920, -276.8851948664911333, -249.9215662272306417 ) ) ;
#27518 = CARTESIAN_POINT ( 'NONE',  ( -94.87899353602283270, -285.2921221856511238, -320.6409962755051879 ) ) ;
#27519 = B_SPLINE_CURVE_WITH_KNOTS ( 'NONE', 3,
 ( #40982, #33924, #62832, #75145, #10257, #32048, #60942, #36134, #1084, #70395, #15289, #65509, #66417, #79696, #43691, #26820, #87694, #55706, #56173, #51713, #80149, #8631, #22846, #57922, #13100, #36594, #629, #21939 ),
 .UNSPECIFIED., .F., .F.,
 ( 4, 2, 2, 2, 2, 2, 2, 2, 2, 2, 2, 2, 2, 4 ),
 ( 0.000000000000000000, 0.0007588366528438087811, 0.001517673305687617562, 0.002276509958531426452, 0.003035346611375235124, 0.004553019917062885863, 0.005311856569906778236, 0.006070693222750670609, 0.006829529875594562982, 0.007588366528438454488, 0.009106039834126240101, 0.01062371313981402485, 0.01138254979265798661, 0.01214138644550194837 ),
 .UNSPECIFIED. ) ;
#27520 = CARTESIAN_POINT ( 'NONE',  ( -4.664089697125836764, -281.4066399955497673, -336.0825321686388634 ) ) ;
#27521 = CARTESIAN_POINT ( 'NONE',  ( -110.1064407785872277, -280.3182582730640320, -288.5879567357413293 ) ) ;
#27522 = CARTESIAN_POINT ( 'NONE',  ( -18.55202796198441817, -274.4542557106599361, -195.6338162350585606 ) ) ;
#27523 = CARTESIAN_POINT ( 'NONE',  ( 35.73063161786891584, -275.0779566175285140, -245.9147612736157669 ) ) ;
#27524 = CARTESIAN_POINT ( 'NONE',  ( -23.22219826375168594, -296.7904972994708146, -343.5024141261557702 ) ) ;
#27525 = CARTESIAN_POINT ( 'NONE',  ( 196.1963538710215857, 305.7026273589066250, -40.00000000000000711 ) ) ;
#27526 = CARTESIAN_POINT ( 'NONE',  ( 152.4773011712318578, 19.90414083357004671, -8.234854308319460969 ) ) ;
#27527 = CARTESIAN_POINT ( 'NONE',  ( -104.1530215763134635, -295.1622821068463622, -234.5210099813571105 ) ) ;
#27528 = CARTESIAN_POINT ( 'NONE',  ( 31.31744144402193797, -275.3940920659171638, -295.4863031157839828 ) ) ;
#27529 = CARTESIAN_POINT ( 'NONE',  ( 39.01779417808786832, -295.0713897097376162, -270.2910974489604996 ) ) ;
#27530 = CARTESIAN_POINT ( 'NONE',  ( 1.580966553772762406, -295.7489465650217539, -336.3386500434745585 ) ) ;
#27531 = CARTESIAN_POINT ( 'NONE',  ( -85.01611820745596049, -293.3926104220229263, -212.6794199822438429 ) ) ;
#27532 = CARTESIAN_POINT ( 'NONE',  ( -95.03534499213677122, -275.8927509631027419, -318.0411640013697934 ) ) ;
#27533 = CARTESIAN_POINT ( 'NONE',  ( -110.7010874838116194, -280.3078465204497434, -283.0741390038166401 ) ) ;
#27534 = CARTESIAN_POINT ( 'NONE',  ( -91.47082283380068191, -293.9095507372211387, -321.5367718840875568 ) ) ;
#27535 = CARTESIAN_POINT ( 'NONE',  ( 36.66420507357636183, -283.6196196522857349, -286.6516883121927322 ) ) ;
#27536 = CARTESIAN_POINT ( 'NONE',  ( -38.61655091987873334, -284.9561557716685911, -197.0505558027613802 ) ) ;
#27537 = CARTESIAN_POINT ( 'NONE',  ( -111.2915329965731814, -274.0799573519071828, -284.0611421460235420 ) ) ;
#27538 = ORIENTED_EDGE ( 'NONE', *, *, #45025, .F. ) ;
#27539 = CARTESIAN_POINT ( 'NONE',  ( -109.8942584414632506, -284.1041937039935306, -279.0566610771871865 ) ) ;
#27540 = VERTEX_POINT ( 'NONE', #84990 ) ;
#27541 = CARTESIAN_POINT ( 'NONE',  ( 23.16754149100059479, -283.2640251823428343, -317.5005377996771472 ) ) ;
#27542 = CARTESIAN_POINT ( 'NONE',  ( -113.9436227052690072, -283.3520140231308915, -269.9684668169209658 ) ) ;
#27543 = EDGE_CURVE ( 'NONE', #26691, #49791, #33888, .T. ) ;
#27544 = CARTESIAN_POINT ( 'NONE',  ( -113.0650911497885005, -279.3353231721430348, -282.9622395735897840 ) ) ;
#27545 = CARTESIAN_POINT ( 'NONE',  ( -113.3863934105324063, -279.9848603097133264, -277.2875802944731731 ) ) ;
#27546 = CARTESIAN_POINT ( 'NONE',  ( 8.479139178526475362, -281.3123447839362257, -208.5392560358893945 ) ) ;
#27547 = CARTESIAN_POINT ( 'NONE',  ( 90.32002540683689062, -302.2645883696979467, -200.3030568020284647 ) ) ;
#27548 = CARTESIAN_POINT ( 'NONE',  ( -109.1987091961355105, -267.5305874205028545, -307.0464688485295142 ) ) ;
#27549 = VERTEX_POINT ( 'NONE', #18269 ) ;
#27550 = CARTESIAN_POINT ( 'NONE',  ( -13.50499136230118857, -276.3625292218551408, -199.4256561863484478 ) ) ;
#27551 = CARTESIAN_POINT ( 'NONE',  ( -71.60599505142221233, -195.9056560659656157, -360.2227879542884921 ) ) ;
#27552 = CARTESIAN_POINT ( 'NONE',  ( -96.90943078455200066, -277.1905090651634396, -225.3562214412502840 ) ) ;
#27553 = CARTESIAN_POINT ( 'NONE',  ( 27.17991173863390486, -294.7790864171419685, -230.1252792525458233 ) ) ;
#27554 = CARTESIAN_POINT ( 'NONE',  ( 35.80994277582180274, -292.9061046636203400, -270.7687586548724425 ) ) ;
#27555 = CARTESIAN_POINT ( 'NONE',  ( -112.8633468051969970, -290.2446218697569407, -255.5953112637739935 ) ) ;
#27556 = DIRECTION ( 'NONE',  ( 0.000000000000000000, 0.000000000000000000, 1.000000000000000000 ) ) ;
#27558 = CARTESIAN_POINT ( 'NONE',  ( -4.217421090718192822, -284.8962691664578983, -204.4124822453422325 ) ) ;
#27557 = CARTESIAN_POINT ( 'NONE',  ( -19.44305090082077925, -293.4011539718557060, -344.7004690562007454 ) ) ;
#27559 = CARTESIAN_POINT ( 'NONE',  ( -77.95032455262003168, -293.3604789860931419, -208.2176943468571437 ) ) ;
#27560 = CARTESIAN_POINT ( 'NONE',  ( -97.77091240416136486, -286.4464078370949096, -228.5111983569666734 ) ) ;
#27561 = ORIENTED_EDGE ( 'NONE', *, *, #81578, .T. ) ;
#27562 = CARTESIAN_POINT ( 'NONE',  ( -27.88998671274746854, -293.1104793945594906, -194.1269984574122134 ) ) ;
#27563 = CARTESIAN_POINT ( 'NONE',  ( -66.57844489734239346, -283.9380611388800162, -337.3314111948610048 ) ) ;
#27564 = CARTESIAN_POINT ( 'NONE',  ( 1.554527671027237989, -293.3391839350978785, -336.3542402111345382 ) ) ;
#27565 = CARTESIAN_POINT ( 'NONE',  ( 16.57994092810535491, -289.1121046293197310, -325.1764671271653810 ) ) ;
#27566 = CARTESIAN_POINT ( 'NONE',  ( -102.2459730535420874, -290.5013852880882723, -311.7745466030323769 ) ) ;
#27567 = CARTESIAN_POINT ( 'NONE',  ( 10.11687371408157432, -288.5432702663702003, -325.8958201078382899 ) ) ;
#27568 = VERTEX_POINT ( 'NONE', #34359 ) ;
#27569 = CARTESIAN_POINT ( 'NONE',  ( 205.2786681169002350, 32.98517505407394168, 15.00000000000000000 ) ) ;
#27570 = CARTESIAN_POINT ( 'NONE',  ( -109.6416740960722080, -298.7037897777284456, -247.5371003688834151 ) ) ;
#27571 = CARTESIAN_POINT ( 'NONE',  ( -37.23733949140996202, -296.7382676063367057, -193.8535291003551890 ) ) ;
#27572 = CARTESIAN_POINT ( 'NONE',  ( -3.028269771781935127, -279.5759642878047657, -205.6476126200663259 ) ) ;
#27573 = CARTESIAN_POINT ( 'NONE',  ( -71.36993810734335852, -273.1224594234291203, -201.3567273717213197 ) ) ;
#27574 = CARTESIAN_POINT ( 'NONE',  ( -39.73072626825614151, -293.5625392248066419, -344.0282676493075087 ) ) ;
#27575 = CARTESIAN_POINT ( 'NONE',  ( 24.62988793403597043, -276.7592097233517734, -229.8951287291834831 ) ) ;
#27576 = CARTESIAN_POINT ( 'NONE',  ( -81.79198737790059681, -271.5794588559407998, -210.8404500025061452 ) ) ;
#27577 = VECTOR ( 'NONE', #7314, 1000.000000000000000 ) ;
#27578 = CARTESIAN_POINT ( 'NONE',  ( -73.48464267762841473, -296.7482661672439690, -334.2424001322260665 ) ) ;
#27579 = CARTESIAN_POINT ( 'NONE',  ( -23.44682825410629690, -295.9501498990190385, -342.3932076799439983 ) ) ;
#27580 = CARTESIAN_POINT ( 'NONE',  ( 156.4851178187871312, 0.000000000000000000, -7.000000000000000888 ) ) ;
#27581 = CARTESIAN_POINT ( 'NONE',  ( -63.96736559493859886, -296.9938349776746804, -341.7579971404136359 ) ) ;
#27582 = TOROIDAL_SURFACE ( 'NONE', #38149, 16.36528803885689243, 1.000000000000000000 ) ;
#27583 = CARTESIAN_POINT ( 'NONE',  ( -100.0068637073478186, -295.1116386563899709, -228.8273835354135315 ) ) ;
#27584 = CARTESIAN_POINT ( 'NONE',  ( 12.96730746947797108, -293.4289607138384213, -217.3243720177621014 ) ) ;
#27585 = CARTESIAN_POINT ( 'NONE',  ( -29.86478826530026609, -274.9473554526223325, -193.8872361055482543 ) ) ;
#27586 = CARTESIAN_POINT ( 'NONE',  ( -75.26784763849518356, -290.1110113719590231, -207.2383149908752102 ) ) ;
#27587 = CARTESIAN_POINT ( 'NONE',  ( -51.97598062056112411, -275.8651589376317474, -196.7495040150124055 ) ) ;
#27588 = CARTESIAN_POINT ( 'NONE',  ( -85.77435706258641801, -273.8942172896033753, -210.5798111607869885 ) ) ;
#27590 = CARTESIAN_POINT ( 'NONE',  ( -95.61864146156943889, -296.2672931152511069, -314.3804144753287346 ) ) ;
#27589 = CIRCLE ( 'NONE', #7891, 24.00000000000000355 ) ;
#27591 = CIRCLE ( 'NONE', #71392, 0.5000000000000128786 ) ;
#27592 = CARTESIAN_POINT ( 'NONE',  ( -8.196931093351738085, -282.4117920468839884, -200.8561935027971970 ) ) ;
#27593 = CARTESIAN_POINT ( 'NONE',  ( 38.30968493627192828, -280.0890452723554063, -258.6079853689292918 ) ) ;
#27594 = CARTESIAN_POINT ( 'NONE',  ( -99.57216309763640538, -277.3003594425779283, -315.5574229866656992 ) ) ;
#27595 = CARTESIAN_POINT ( 'NONE',  ( 36.41230483756002911, -280.1942506987561501, -289.5128063912928837 ) ) ;
#27596 = CARTESIAN_POINT ( 'NONE',  ( -1.277964097544683986, -280.5748210313462323, -336.3259483538149652 ) ) ;
#27597 = CARTESIAN_POINT ( 'NONE',  ( 22.77257207110082149, -273.5389236089415590, -227.8934591347680225 ) ) ;
#27598 = CARTESIAN_POINT ( 'NONE',  ( -81.68449435463507768, -279.6555729793868750, -330.9119404235894990 ) ) ;
#27599 = DIRECTION ( 'NONE',  ( -0.000000000000000000, 1.000000000000000000, -0.000000000000000000 ) ) ;
#27600 = CARTESIAN_POINT ( 'NONE',  ( 153.3249703231417982, 19.65100358619422849, 12.05267380659650556 ) ) ;
#27601 = CARTESIAN_POINT ( 'NONE',  ( -94.79007543861693819, -295.4735565898628238, -220.5467333199635505 ) ) ;
#27602 = CARTESIAN_POINT ( 'NONE',  ( 10.10318621292782204, -290.7221492208485643, -211.7500544161656535 ) ) ;
#27603 = CARTESIAN_POINT ( 'NONE',  ( -19.38677432578216653, -292.2768278923069829, -195.4289250637597206 ) ) ;
#27604 = CARTESIAN_POINT ( 'NONE',  ( -34.33823053107608558, -279.0146256596172520, -345.4677594956069697 ) ) ;
#27605 = CARTESIAN_POINT ( 'NONE',  ( -36.69389282156906518, -272.0601337845139369, -195.3511557099496372 ) ) ;
#27606 = PLANE ( 'NONE',  #49939 ) ;
#27607 = CARTESIAN_POINT ( 'NONE',  ( -44.26250081192613806, -285.0590500688032876, -345.6558632286009924 ) ) ;
#27608 = CARTESIAN_POINT ( 'NONE',  ( 209.2522817606372882, 36.37164913089609541, 14.78224109794540198 ) ) ;
#27609 = CARTESIAN_POINT ( 'NONE',  ( -80.22184159682915094, -283.4717775772102186, -208.7656702330205860 ) ) ;
#27610 = DIRECTION ( 'NONE',  ( -0.000000000000000000, -1.000000000000000000, -0.000000000000000000 ) ) ;
#27611 = CARTESIAN_POINT ( 'NONE',  ( -47.86505605325606894, -293.9837412655173239, -343.0514383758520580 ) ) ;
#27612 = CARTESIAN_POINT ( 'NONE',  ( 36.50552166033610746, -285.5934042910004109, -262.7813216009982966 ) ) ;
#27613 = DIRECTION ( 'NONE',  ( 0.000000000000000000, 0.000000000000000000, -1.000000000000000000 ) ) ;
#27614 = CARTESIAN_POINT ( 'NONE',  ( -71.87372008138898138, -293.5084023882123461, -336.9528128238608815 ) ) ;
#27615 = CARTESIAN_POINT ( 'NONE',  ( -113.2165305978939358, -282.9297264235336797, -278.4677728390816469 ) ) ;
#27616 = CARTESIAN_POINT ( 'NONE',  ( -93.71433507312700328, -280.8219783564400700, -222.7122017083493688 ) ) ;
#27617 = CARTESIAN_POINT ( 'NONE',  ( -60.40506835693592791, -286.9647725944641365, -197.2572805548575730 ) ) ;
#27618 = CARTESIAN_POINT ( 'NONE',  ( 38.17831918871550556, -279.6795977643929518, -261.4908110275704303 ) ) ;
#27619 = CARTESIAN_POINT ( 'NONE',  ( 15.02949583536310918, -286.8168700710117491, -219.5058544068149615 ) ) ;
#27620 = CARTESIAN_POINT ( 'NONE',  ( -110.9814983762989442, -279.9735419037218094, -270.6584032288535013 ) ) ;
#27621 = CARTESIAN_POINT ( 'NONE',  ( -106.4132771030820663, -279.0330385724807343, -294.6335500764914741 ) ) ;
#27622 = EDGE_CURVE ( 'NONE', #200, #89141, #76036, .T. ) ;
#27623 = CARTESIAN_POINT ( 'NONE',  ( -37.99405631378817105, -288.0239039503819072, -195.0087375376406555 ) ) ;
#27624 = ORIENTED_EDGE ( 'NONE', *, *, #91412, .T. ) ;
#27625 = CARTESIAN_POINT ( 'NONE',  ( -73.27873688191642998, -297.4226936028829869, -202.2028651255565421 ) ) ;
#27626 = CARTESIAN_POINT ( 'NONE',  ( -109.7091805230882642, -292.7688189929253895, -252.0116696546971866 ) ) ;
#27627 = CYLINDRICAL_SURFACE ( 'NONE', #52977, 5.000000000000004441 ) ;
#27628 = CARTESIAN_POINT ( 'NONE',  ( -55.56934967048406548, -291.7662352645559167, -350.3683826091709648 ) ) ;
#27629 = ORIENTED_EDGE ( 'NONE', *, *, #87430, .F. ) ;
#27630 = CARTESIAN_POINT ( 'NONE',  ( -13.61642214219629388, -272.3592773142192982, -199.0369312755754265 ) ) ;
#27631 = EDGE_CURVE ( 'NONE', #59332, #86133, #61718, .T. ) ;
#27632 = CARTESIAN_POINT ( 'NONE',  ( -19.49463162005092087, -293.2263260178216910, -344.4959440713471963 ) ) ;
#27633 = CARTESIAN_POINT ( 'NONE',  ( -65.59072381180652656, -297.1801351323019276, -202.9817361014126789 ) ) ;
#27634 = CARTESIAN_POINT ( 'NONE',  ( -53.54228963306366040, -290.7839182215230949, -342.2516503924534277 ) ) ;
#27635 = CARTESIAN_POINT ( 'NONE',  ( -11.40880824863868526, -282.1546804486543465, -200.9855071766168919 ) ) ;
#27636 = CARTESIAN_POINT ( 'NONE',  ( -74.12759924740237238, -290.9563645807033367, -337.3492128304811217 ) ) ;
#27637 = CARTESIAN_POINT ( 'NONE',  ( -112.6892721554205394, -292.0343267173346362, -257.0930486787603400 ) ) ;
#27638 = CARTESIAN_POINT ( 'NONE',  ( -40.07153979562591672, -288.0179972238098003, -195.4108102660858606 ) ) ;
#27639 = CARTESIAN_POINT ( 'NONE',  ( -62.04963915970403576, -279.9063971833180062, -197.3767164906247444 ) ) ;
#27640 = CARTESIAN_POINT ( 'NONE',  ( -30.74155502696780928, -293.0491720647729039, -345.6323095663776144 ) ) ;
#27641 = CARTESIAN_POINT ( 'NONE',  ( 38.66750327269723186, -281.5404891994229502, -282.7561024184780081 ) ) ;
#27642 = CARTESIAN_POINT ( 'NONE',  ( 26.44888698417057782, -277.9258663280769497, -308.3298745400100529 ) ) ;
#27643 = CARTESIAN_POINT ( 'NONE',  ( -69.85430415644619018, -297.9805209788416391, -337.9475929042657754 ) ) ;
#27644 = CARTESIAN_POINT ( 'NONE',  ( 37.49803502612482475, -273.6243876975385660, -257.1341533668179977 ) ) ;
#27646 = VECTOR ( 'NONE', #73698, 1000.000000000000000 ) ;
#27645 = FACE_OUTER_BOUND ( 'NONE', #58084, .T. ) ;
#27647 = CARTESIAN_POINT ( 'NONE',  ( 13.38233414402698251, -280.2926585656831548, -217.7067638255011843 ) ) ;
#27648 = CIRCLE ( 'NONE', #14065, 0.5000000000000004441 ) ;
#27649 = CARTESIAN_POINT ( 'NONE',  ( -37.11266466071617742, -278.2543790046399863, -346.9766961103813401 ) ) ;
#27650 = CARTESIAN_POINT ( 'NONE',  ( -16.51685545203067207, -275.6419905724877708, -199.8270722053946997 ) ) ;
#27651 = CARTESIAN_POINT ( 'NONE',  ( -97.38883146410131531, -284.2531725154895526, -222.5368330158063088 ) ) ;
#27652 = CARTESIAN_POINT ( 'NONE',  ( -86.62019348327432056, -293.1167054582231231, -215.0688958986046373 ) ) ;
#27653 = CARTESIAN_POINT ( 'NONE',  ( -108.4277388919072109, -274.5052111951486609, -242.7710011707785327 ) ) ;
#27654 = CIRCLE ( 'NONE', #74538, 1.000000000000008882 ) ;
#27655 = CARTESIAN_POINT ( 'NONE',  ( -31.31571669936070279, -275.4418987109212935, -194.0787549732181390 ) ) ;
#27656 = FACE_BOUND ( 'NONE', #56348, .T. ) ;
#27657 = CARTESIAN_POINT ( 'NONE',  ( 32.51577207138818437, -275.6665440664735343, -291.5924990400104093 ) ) ;
#27658 = CARTESIAN_POINT ( 'NONE',  ( -102.8309847285540855, -299.0350594090631375, -234.1508704494058009 ) ) ;
#27659 = CARTESIAN_POINT ( 'NONE',  ( -74.73442363393843380, -281.5504951717720132, -335.2415685310998583 ) ) ;
#27660 = AXIS2_PLACEMENT_3D ( 'NONE', #36461, #78627, #86173 ) ;
#27661 = CARTESIAN_POINT ( 'NONE',  ( -97.44439548734553114, -290.8633287890763199, -222.2631938877581206 ) ) ;
#27662 = CARTESIAN_POINT ( 'NONE',  ( 36.32636387201440442, -273.7315544114858312, -282.7087091169038331 ) ) ;
#27663 = CARTESIAN_POINT ( 'NONE',  ( 18.07712842093451400, -289.8739412439222178, -322.6601988303125950 ) ) ;
#27664 = CARTESIAN_POINT ( 'NONE',  ( -88.13489411781456795, -290.2414784701313124, -217.4300511501999154 ) ) ;
#27665 = ORIENTED_EDGE ( 'NONE', *, *, #11779, .F. ) ;
#27666 = CARTESIAN_POINT ( 'NONE',  ( -113.2305918655839747, -289.0090099640698895, -279.7139975508565612 ) ) ;
#27667 = CARTESIAN_POINT ( 'NONE',  ( -109.8110189791233324, -290.1007034199903956, -279.3213251243636819 ) ) ;
#27668 = ORIENTED_EDGE ( 'NONE', *, *, #50647, .T. ) ;
#27669 = CARTESIAN_POINT ( 'NONE',  ( 4.997521423533825669, -287.6892176130587018, -206.3534999519835651 ) ) ;
#27670 = CARTESIAN_POINT ( 'NONE',  ( -100.8322833111559049, -279.3792902346340838, -234.2912783131542085 ) ) ;
#27671 = CARTESIAN_POINT ( 'NONE',  ( -44.77938748352222120, -294.0643969775455275, -346.7436845850107829 ) ) ;
#27672 = CARTESIAN_POINT ( 'NONE',  ( -111.7742044345890378, -284.9608910494137604, -289.7294870724063571 ) ) ;
#27673 = CARTESIAN_POINT ( 'NONE',  ( -85.50298577752880647, -285.7399204422563344, -210.3091833257372514 ) ) ;
#27674 = CARTESIAN_POINT ( 'NONE',  ( 24.15053851264908147, -282.4311609880903688, -309.8341772453737804 ) ) ;
#27675 = CARTESIAN_POINT ( 'NONE',  ( 84.52794612516449035, 83.35382402778485300, -302.3197191937509842 ) ) ;
#27676 = CARTESIAN_POINT ( 'NONE',  ( -96.29398733087926132, -239.0646663885169971, -340.8987983896206515 ) ) ;
#27677 = CARTESIAN_POINT ( 'NONE',  ( -56.32650456138331663, -169.0553163394745297, -360.7103527500878499 ) ) ;
#27678 = CARTESIAN_POINT ( 'NONE',  ( 24.11448446657037081, -275.2987689420457400, -310.1500906038724565 ) ) ;
#27679 = CARTESIAN_POINT ( 'NONE',  ( -0.3785840698713352492, -273.4763231492167392, -207.0380590452716945 ) ) ;
#27680 = CARTESIAN_POINT ( 'NONE',  ( 8.864193877305035940, -293.9448730891281230, -331.8797514379827476 ) ) ;
#27681 = CARTESIAN_POINT ( 'NONE',  ( -54.38370458779698424, -170.1712701406207486, -361.1722839838796517 ) ) ;
#27682 = CARTESIAN_POINT ( 'NONE',  ( 22.38394935977466105, -273.5921984346008458, -222.5266875958565720 ) ) ;
#27683 = CARTESIAN_POINT ( 'NONE',  ( -44.71495253834831374, -299.8184124375551391, -196.4417532559928077 ) ) ;
#27684 = CARTESIAN_POINT ( 'NONE',  ( -33.50595437956121714, -293.1812074276649014, -197.1398770807768983 ) ) ;
#27685 = ORIENTED_EDGE ( 'NONE', *, *, #38265, .T. ) ;
#27686 = CARTESIAN_POINT ( 'NONE',  ( -114.1027984822798089, -297.5027397814274650, -269.6168117708892282 ) ) ;
#27687 = CARTESIAN_POINT ( 'NONE',  ( 35.69179780106460242, -288.0892547718623860, -273.7564419364115906 ) ) ;
#27688 = VECTOR ( 'NONE', #1072, 1000.000000000000000 ) ;
#27689 = CARTESIAN_POINT ( 'NONE',  ( 36.12957975802836330, -294.0718971154751102, -247.8637880870911374 ) ) ;
#27690 = CARTESIAN_POINT ( 'NONE',  ( -92.64840805114447164, -296.3111780202609111, -323.8465829417602322 ) ) ;
#27691 = CARTESIAN_POINT ( 'NONE',  ( 12.90161958726231184, -292.9443056210603231, -217.4025603315702995 ) ) ;
#27692 = EDGE_LOOP ( 'NONE', ( #13955, #11214, #57944, #32676 ) ) ;
#27693 = CARTESIAN_POINT ( 'NONE',  ( 22.47755597598199984, -276.8442076921319881, -224.1776267369401410 ) ) ;
#27694 = ORIENTED_EDGE ( 'NONE', *, *, #92268, .F. ) ;
#27695 = CARTESIAN_POINT ( 'NONE',  ( -110.4892203164836957, -278.3620329675359244, -246.3390350988140085 ) ) ;
#27696 = CARTESIAN_POINT ( 'NONE',  ( -6.440566982790778106, -275.4095560453952203, -203.9643679174246529 ) ) ;
#27697 = CARTESIAN_POINT ( 'NONE',  ( -3.035364976444239637, -276.2592069854427450, -202.5450663414689529 ) ) ;
#27698 = CARTESIAN_POINT ( 'NONE',  ( -108.1989566239285665, -276.2395449046551903, -296.1587096935703585 ) ) ;
#27699 = CARTESIAN_POINT ( 'NONE',  ( -65.61979572447937414, -298.3237107666147381, -202.9501249783413641 ) ) ;
#27700 = CARTESIAN_POINT ( 'NONE',  ( -108.3999240650138773, -295.3781541007084002, -251.1787687992029134 ) ) ;
#27701 = DIRECTION ( 'NONE',  ( 0.000000000000000000, 1.000000000000000000, 0.000000000000000000 ) ) ;
#27702 = CARTESIAN_POINT ( 'NONE',  ( -113.2374326532378319, -278.8864908656411217, -282.9850907236757962 ) ) ;
#27703 = CARTESIAN_POINT ( 'NONE',  ( -35.11550923842111160, -277.1901022697819030, -343.3271654200470948 ) ) ;
#27704 = EDGE_CURVE ( 'NONE', #46837, #63636, #77924, .T. ) ;
#27705 = CARTESIAN_POINT ( 'NONE',  ( -37.96153848987580659, -284.7293711236492300, -193.8567777440656528 ) ) ;
#27706 = CARTESIAN_POINT ( 'NONE',  ( -59.62938112530403600, -299.7644559211680644, -198.5205078157930814 ) ) ;
#27707 = FACE_OUTER_BOUND ( 'NONE', #88, .T. ) ;
#27708 = AXIS2_PLACEMENT_3D ( 'NONE', #30260, #67653, #24080 ) ;
#27709 = CARTESIAN_POINT ( 'NONE',  ( 29.56860480009935799, -287.1481684185879999, -300.0775266694301422 ) ) ;
#27710 = CARTESIAN_POINT ( 'NONE',  ( 0.9430474256644593156, -278.8099815993402899, -206.9594410590462417 ) ) ;
#27712 = CARTESIAN_POINT ( 'NONE',  ( -68.40717075724357699, -281.5433517477497389, -338.0091093476349329 ) ) ;
#27711 = CARTESIAN_POINT ( 'NONE',  ( -89.88165379784589959, -277.8674667091413539, -218.7629258732470419 ) ) ;
#27713 = CARTESIAN_POINT ( 'NONE',  ( -77.95547014114582396, -287.5069994248777334, -207.2488651788966081 ) ) ;
#27714 = CARTESIAN_POINT ( 'NONE',  ( -7.331332943831510462, -277.8546272854011363, -337.3425211279961218 ) ) ;
#27715 = DIRECTION ( 'NONE',  ( 1.000000000000000000, 0.000000000000000000, -0.000000000000000000 ) ) ;
#27716 = VECTOR ( 'NONE', #8706, 1000.000000000000000 ) ;
#27717 = CARTESIAN_POINT ( 'NONE',  ( -51.15075254707824115, -275.4661958800792263, -345.0824943266380274 ) ) ;
#27718 = AXIS2_PLACEMENT_3D ( 'NONE', #32219, #1471, #84263 ) ;
#27719 = CARTESIAN_POINT ( 'NONE',  ( 35.70423805345799195, -276.2555875449469340, -274.3098780883924519 ) ) ;
#27720 = CARTESIAN_POINT ( 'NONE',  ( 28.17669662114862206, -284.0431787711817719, -307.3097380317208831 ) ) ;
#27721 = CARTESIAN_POINT ( 'NONE',  ( 175.2296996224750103, 275.0000000000000568, 0.000000000000000000 ) ) ;
#27722 = CARTESIAN_POINT ( 'NONE',  ( -3.679862741015699434, -290.5316854709591325, -338.0230535551716571 ) ) ;
#27723 = AXIS2_PLACEMENT_3D ( 'NONE', #83974, #40389, #47977 ) ;
#27724 = MANIFOLD_SOLID_BREP ( 'Boss-Extrude27', #58252 ) ;
#27725 = CARTESIAN_POINT ( 'NONE',  ( -91.42594102420888191, -293.8212159059965529, -322.3954285541440186 ) ) ;
#27726 = DIRECTION ( 'NONE',  ( 0.000000000000000000, 0.000000000000000000, 1.000000000000000000 ) ) ;
#27727 = CARTESIAN_POINT ( 'NONE',  ( -5.076536440178148091, -273.1708663601064586, -204.3153676671505821 ) ) ;
#27728 = CARTESIAN_POINT ( 'NONE',  ( 35.70275299060480023, -291.5190268903338620, -257.0474503475281836 ) ) ;
#27729 = CARTESIAN_POINT ( 'NONE',  ( 64.33209501061345748, 48.33985520751024723, -319.1928417150128325 ) ) ;
#27730 = DIRECTION ( 'NONE',  ( -0.2456588035076310295, 0.9693563597868428694, 0.000000000000000000 ) ) ;
#27731 = CARTESIAN_POINT ( 'NONE',  ( -38.92536795428206631, -287.5515671899481731, -346.6513516374243409 ) ) ;
#27732 = CARTESIAN_POINT ( 'NONE',  ( 37.97390402269154919, -285.6643135538512865, -260.2847205746248278 ) ) ;
#27733 = AXIS2_PLACEMENT_3D ( 'NONE', #33287, #40826, #83943 ) ;
#27734 = CARTESIAN_POINT ( 'NONE',  ( -110.1981253010328317, -286.1129925509735017, -260.0017633558638295 ) ) ;
#27735 = CARTESIAN_POINT ( 'NONE',  ( -52.13154334789275168, -286.6607744384797911, -198.7101426649522011 ) ) ;
#27736 = ADVANCED_FACE ( 'NONE', ( #69867 ), #56315, .T. ) ;
#27737 = CARTESIAN_POINT ( 'NONE',  ( -112.1769488774193064, -292.4136254876100338, -279.6275797635290132 ) ) ;
#27738 = CARTESIAN_POINT ( 'NONE',  ( 21.50385362800916766, -274.2795883042095397, -317.7789904473227693 ) ) ;
#27739 = CARTESIAN_POINT ( 'NONE',  ( 8.231962502020227390, -276.7812389605397811, -332.4656978067777118 ) ) ;
#27740 = CARTESIAN_POINT ( 'NONE',  ( -85.57467267313248271, -289.4712467822806161, -212.1305440981531092 ) ) ;
#27741 = CARTESIAN_POINT ( 'NONE',  ( -103.6057918900136201, -278.0400668303644238, -309.6839154718165332 ) ) ;
#27742 = CARTESIAN_POINT ( 'NONE',  ( -111.6909798513124485, -298.6248778251186877, -263.1656264632775333 ) ) ;
#27743 = FACE_OUTER_BOUND ( 'NONE', #77258, .T. ) ;
#27744 = DIRECTION ( 'NONE',  ( 0.000000000000000000, 0.5150380749100592626, 0.8571673007021092250 ) ) ;
#27745 = CARTESIAN_POINT ( 'NONE',  ( -80.93201050390715068, -282.3424669813427386, -329.5947774082359274 ) ) ;
#27746 = CARTESIAN_POINT ( 'NONE',  ( -71.57071146206192225, -277.5998769881154544, -203.6132336864991430 ) ) ;
#27747 = DIRECTION ( 'NONE',  ( -1.000000000000000000, 0.000000000000000000, 0.000000000000000000 ) ) ;
#27748 = CARTESIAN_POINT ( 'NONE',  ( 19.53216446816905716, -273.3351467189945083, -219.4103534795385144 ) ) ;
#27749 = CARTESIAN_POINT ( 'NONE',  ( -108.2730038300416595, -277.6671135310381828, -288.0944539993737408 ) ) ;
#27750 = CARTESIAN_POINT ( 'NONE',  ( 18.51045061406193426, -295.7506505319004759, -318.4557745035315861 ) ) ;
#27751 = AXIS2_PLACEMENT_3D ( 'NONE', #66303, #9914, #89429 ) ;
#27752 = CARTESIAN_POINT ( 'NONE',  ( 37.68514430102204926, -280.2721798262482480, -254.4090895892437345 ) ) ;
#27753 = CARTESIAN_POINT ( 'NONE',  ( -68.60693562699356107, -296.4146222192179039, -336.6009713808896322 ) ) ;
#27754 = CARTESIAN_POINT ( 'NONE',  ( -101.2073047603732903, -297.3087404217823746, -312.5815087232940073 ) ) ;
#27755 = CARTESIAN_POINT ( 'NONE',  ( -103.2223275882264062, -272.6446705769380401, -238.8677788116357306 ) ) ;
#27756 = CARTESIAN_POINT ( 'NONE',  ( -36.20056714911405038, -294.0665827818957609, -195.3569767363293010 ) ) ;
#27757 = CARTESIAN_POINT ( 'NONE',  ( -112.9986466442123572, -284.9013320331508794, -255.7649088036768603 ) ) ;
#27758 = CARTESIAN_POINT ( 'NONE',  ( 1.800476435031018951, -272.7094804265789776, -205.4905122053528714 ) ) ;
#27759 = CARTESIAN_POINT ( 'NONE',  ( 38.67463123557805460, -287.5429613925635408, -282.9537771995813955 ) ) ;
#27760 = CARTESIAN_POINT ( 'NONE',  ( -71.72116591213416825, -281.5754793454692617, -204.0903970262988310 ) ) ;
#27761 = ADVANCED_FACE ( 'NONE', ( #12582 ), #85046, .T. ) ;
#27762 = CARTESIAN_POINT ( 'NONE',  ( -77.16699619046305259, -284.5629841276941647, -208.8407701021576202 ) ) ;
#27763 = CARTESIAN_POINT ( 'NONE',  ( -64.74075229874868853, -287.4096252036816281, -340.2321406871787417 ) ) ;
#27764 = CARTESIAN_POINT ( 'NONE',  ( 69.94643833976951441, 44.42656045538938514, -317.4108715071801612 ) ) ;
#27765 = CARTESIAN_POINT ( 'NONE',  ( -9.464111096576960591, -285.9342049204319665, -202.8136920183264351 ) ) ;
#27766 = CARTESIAN_POINT ( 'NONE',  ( 17.66606512967681653, -283.2304255070220051, -323.9811409034066969 ) ) ;
#27767 = ADVANCED_FACE ( 'NONE', ( #32379 ), #49394, .F. ) ;
#27768 = CARTESIAN_POINT ( 'NONE',  ( -97.27233137253044504, -290.2554564205926795, -222.3909225182138130 ) ) ;
#27769 = CARTESIAN_POINT ( 'NONE',  ( -97.08252839257366418, -280.7918564639961119, -223.0591745013976777 ) ) ;
#27770 = CARTESIAN_POINT ( 'NONE',  ( -74.78131832722732497, -280.8796353169584563, -203.6410066050127909 ) ) ;
#27771 = CARTESIAN_POINT ( 'NONE',  ( 34.48506770012869538, -281.5583507417507008, -283.4663118048673596 ) ) ;
#27772 = CARTESIAN_POINT ( 'NONE',  ( -10.80579484633922327, -276.3981916850656830, -200.1568545849455063 ) ) ;
#27773 = CARTESIAN_POINT ( 'NONE',  ( -8.388037073456116488, -294.6835563454133649, -341.7666387349515276 ) ) ;
#27774 = CARTESIAN_POINT ( 'NONE',  ( -110.5568734288250425, -288.3838469392683237, -284.9656979898983309 ) ) ;
#27775 = CARTESIAN_POINT ( 'NONE',  ( -100.1545839252071488, -295.9915693547708884, -232.4633854209693311 ) ) ;
#27776 = EDGE_LOOP ( 'NONE', ( #3700, #12399, #30680 ) ) ;
#27777 = ORIENTED_EDGE ( 'NONE', *, *, #90893, .T. ) ;
#27778 = CARTESIAN_POINT ( 'NONE',  ( -23.77961776314300479, -284.7976793969160099, -343.5552715542814894 ) ) ;
#27779 = CARTESIAN_POINT ( 'NONE',  ( -108.3205719654971517, -295.9920168870833095, -287.5628310995685979 ) ) ;
#27780 = AXIS2_PLACEMENT_3D ( 'NONE', #88358, #59508, #88814 ) ;
#27781 = CARTESIAN_POINT ( 'NONE',  ( 10.91357574335173375, -293.7812204986319671, -210.6864219412660191 ) ) ;
#27782 = CARTESIAN_POINT ( 'NONE',  ( -70.25339703745979136, -284.1491536326142295, -335.6492517785920313 ) ) ;
#27783 = CARTESIAN_POINT ( 'NONE',  ( -46.83996842348226153, -272.9930901258628637, -194.1862985738517864 ) ) ;
#27784 = CARTESIAN_POINT ( 'NONE',  ( 0.6761292927307080980, -289.2108532868189172, -337.2640755107474320 ) ) ;
#27785 = CARTESIAN_POINT ( 'NONE',  ( -85.33846531074344455, -281.8469817804627837, -328.9837758017661713 ) ) ;
#27786 = CARTESIAN_POINT ( 'NONE',  ( -93.57444636036071017, -290.1676445437156531, -323.0081031047207034 ) ) ;
#27787 = CARTESIAN_POINT ( 'NONE',  ( 17.84429787934677236, -288.5673809809975410, -318.2551638927276940 ) ) ;
#27788 = CARTESIAN_POINT ( 'NONE',  ( 164.2231345125756263, 300.2961574867697436, -7.500000000000000000 ) ) ;
#27789 = AXIS2_PLACEMENT_3D ( 'NONE', #1707, #44788, #81699 ) ;
#27790 = FACE_OUTER_BOUND ( 'NONE', #88683, .T. ) ;
#27791 = CARTESIAN_POINT ( 'NONE',  ( 202.2091371056811795, 292.1033490241518393, -68.21892602122903781 ) ) ;
#27792 = CARTESIAN_POINT ( 'NONE',  ( 35.78497577281001440, -284.8380690714490129, -253.7030783399848985 ) ) ;
#27793 = EDGE_LOOP ( 'NONE', ( #35681, #16712 ) ) ;
#27794 = CARTESIAN_POINT ( 'NONE',  ( -43.76452800803483001, -278.8895441777788733, -197.2834616080425008 ) ) ;
#27795 = CARTESIAN_POINT ( 'NONE',  ( 39.60983844573426182, -275.1932189243736389, -268.3105076929415418 ) ) ;
#27796 = CARTESIAN_POINT ( 'NONE',  ( -35.03626274600039636, -279.0232862442031774, -345.1589347151418679 ) ) ;
#27797 = CARTESIAN_POINT ( 'NONE',  ( 186.3940997172195750, 260.5663691252829608, -151.7046075576564590 ) ) ;
#27798 = CARTESIAN_POINT ( 'NONE',  ( 32.64061832101208438, -279.7326540102445733, -239.6840679964911374 ) ) ;
#27800 = CIRCLE ( 'NONE', #5079, 9.550761578869391144 ) ;
#27799 = CARTESIAN_POINT ( 'NONE',  ( -98.90283554046479253, -281.9965521890634363, -312.6658560471549890 ) ) ;
#27801 = CARTESIAN_POINT ( 'NONE',  ( -96.60287615452892851, -297.6662759078676572, -317.9431062379033506 ) ) ;
#27802 = CARTESIAN_POINT ( 'NONE',  ( 35.70373570007519248, -294.0856817030418711, -273.4853544332152069 ) ) ;
#27803 = VERTEX_POINT ( 'NONE', #50307 ) ;
#27804 = CARTESIAN_POINT ( 'NONE',  ( -107.4671840212320149, -289.5269946965645431, -248.3264842510507435 ) ) ;
#27805 = CARTESIAN_POINT ( 'NONE',  ( 24.39307639438615283, -275.5931224610558843, -224.5121250317246506 ) ) ;
#27806 = CARTESIAN_POINT ( 'NONE',  ( -107.1965291664068474, -272.8348866151536072, -248.9911961818465045 ) ) ;
#27807 = VERTEX_POINT ( 'NONE', #57893 ) ;
#27808 = LINE ( 'NONE', #19748, #80984 ) ;
#27809 = CARTESIAN_POINT ( 'NONE',  ( 153.9133111279456045, 20.47222690886501795, -13.06183683676589524 ) ) ;
#27810 = AXIS2_PLACEMENT_3D ( 'NONE', #63497, #69165, #69630 ) ;
#27811 = AXIS2_PLACEMENT_3D ( 'NONE', #92152, #71340, #13122 ) ;
#27812 = DIRECTION ( 'NONE',  ( 0.000000000000000000, 0.000000000000000000, -1.000000000000000000 ) ) ;
#27813 = TOROIDAL_SURFACE ( 'NONE', #89741, 1.500000000000000888, 0.5000000000000000000 ) ;
#27814 = CARTESIAN_POINT ( 'NONE',  ( 5.090934676742263854, -281.7208644691550035, -210.5807066730290558 ) ) ;
#27815 = CARTESIAN_POINT ( 'NONE',  ( -96.91658063507647114, -280.9518433919937479, -223.1932514803793310 ) ) ;
#27816 = CARTESIAN_POINT ( 'NONE',  ( -108.8922226143005645, -283.8170366458926992, -254.6843170608131288 ) ) ;
#27817 = CARTESIAN_POINT ( 'NONE',  ( 27.52688981155101189, -282.9272361707023151, -234.2649752909618428 ) ) ;
#27818 = CARTESIAN_POINT ( 'NONE',  ( 29.77785774090250115, -274.4382455516015398, -300.7859877772241930 ) ) ;
#27819 = DIRECTION ( 'NONE',  ( 0.000000000000000000, 0.000000000000000000, 1.000000000000000000 ) ) ;
#27820 = DIRECTION ( 'NONE',  ( 1.000000000000000000, -0.000000000000000000, -0.000000000000000000 ) ) ;
#27821 = CARTESIAN_POINT ( 'NONE',  ( -28.60921274861700070, -277.7470460517150741, -346.7552815917981661 ) ) ;
#27822 = AXIS2_PLACEMENT_3D ( 'NONE', #5043, #54283, #83622 ) ;
#27823 = ORIENTED_EDGE ( 'NONE', *, *, #26635, .F. ) ;
#27824 = ORIENTED_EDGE ( 'NONE', *, *, #60993, .T. ) ;
#27825 = LINE ( 'NONE', #35844, #56523 ) ;
#27826 = CARTESIAN_POINT ( 'NONE',  ( -104.3105844749664044, -286.0757111728668178, -305.0230546044978723 ) ) ;
#27827 = EDGE_CURVE ( 'NONE', #29052, #11817, #72930, .T. ) ;
#27828 = CARTESIAN_POINT ( 'NONE',  ( 35.06901717529549245, -292.6117123840389809, -259.9069443353192241 ) ) ;
#27829 = CARTESIAN_POINT ( 'NONE',  ( 39.53832300489872864, -286.8798796672231219, -268.6953360801878148 ) ) ;
#27830 = CARTESIAN_POINT ( 'NONE',  ( -110.1864277931821334, -282.9633835506042487, -257.1895688095265768 ) ) ;
#27832 = CARTESIAN_POINT ( 'NONE',  ( 25.08112882513839637, -286.3343455412088474, -310.1274911929752420 ) ) ;
#27831 = CARTESIAN_POINT ( 'NONE',  ( -71.43521868467900049, -284.1672966304868169, -205.1460360545227672 ) ) ;
#27833 = CARTESIAN_POINT ( 'NONE',  ( -34.81759642637386776, -284.2248543295481795, -343.7272818156513381 ) ) ;
#27834 = CARTESIAN_POINT ( 'NONE',  ( 1.407088039515917544, -272.5697584191947271, -206.1463839728284029 ) ) ;
#27835 = CARTESIAN_POINT ( 'NONE',  ( -68.15835018713890747, -284.0540769866300366, -200.6563305972389344 ) ) ;
#27836 = CARTESIAN_POINT ( 'NONE',  ( -110.6448680717878261, -298.3486259242654342, -286.2244789886882472 ) ) ;
#27837 = CARTESIAN_POINT ( 'NONE',  ( -4.272386506592572353, -284.4868507060746197, -202.8454595614456082 ) ) ;
#27838 = CARTESIAN_POINT ( 'NONE',  ( -93.27764968013811142, -280.1632085063107525, -223.0705004749699469 ) ) ;
#27839 = CARTESIAN_POINT ( 'NONE',  ( 31.20372759903785820, -289.9559266745055197, -301.2083668266398604 ) ) ;
#27840 = CARTESIAN_POINT ( 'NONE',  ( 161.2244399300530233, -11.64849832608277325, 10.00000000000000000 ) ) ;
#27841 = DIRECTION ( 'NONE',  ( -1.000000000000000000, 0.000000000000000000, 0.000000000000000000 ) ) ;
#27842 = CARTESIAN_POINT ( 'NONE',  ( 7.967528631920097304, -294.5856262091520534, -209.8277574451288672 ) ) ;
#27843 = CARTESIAN_POINT ( 'NONE',  ( -68.90158566030386567, -275.4669149974804441, -338.4118106373981618 ) ) ;
#27844 = CARTESIAN_POINT ( 'NONE',  ( -100.5535876938750022, -289.1712039249697455, -314.0465399323989573 ) ) ;
#27845 = CARTESIAN_POINT ( 'NONE',  ( -3.993190426808736593, -293.0046814795990713, -336.2108003082978485 ) ) ;
#27846 = CARTESIAN_POINT ( 'NONE',  ( -102.5860235892323828, -277.6952922186414980, -236.4211052408278420 ) ) ;
#27847 = CARTESIAN_POINT ( 'NONE',  ( -71.00688282303227084, -295.7426845041317165, -204.1841361142431595 ) ) ;
#27848 = CARTESIAN_POINT ( 'NONE',  ( -68.02222776825142603, -292.9558717238584791, -203.5644417726997801 ) ) ;
#27849 = CARTESIAN_POINT ( 'NONE',  ( 10.64812456238589888, -284.9090924074130839, -330.4860931364851808 ) ) ;
#27850 = CARTESIAN_POINT ( 'NONE',  ( -110.1441692646284025, -294.7416971531197305, -293.2633282135773811 ) ) ;
#27851 = CARTESIAN_POINT ( 'NONE',  ( 21.00233050910374999, -289.7820505990085280, -315.5746672302768161 ) ) ;
#27852 = CARTESIAN_POINT ( 'NONE',  ( -8.869833837920655384, -290.6594074170397448, -199.9102354879851191 ) ) ;
#27853 = CARTESIAN_POINT ( 'NONE',  ( -93.90429155225014313, -292.6401192679890073, -223.2665189243566886 ) ) ;
#27854 = DIRECTION ( 'NONE',  ( 0.9393874931428881636, 0.000000000000000000, 0.3428573139466625785 ) ) ;
#27855 = CARTESIAN_POINT ( 'NONE',  ( -22.71832305514859129, -293.0469688396767651, -198.6759830561543652 ) ) ;
#27856 = ADVANCED_FACE ( 'NONE', ( #65025 ), #20971, .T. ) ;
#27857 = CARTESIAN_POINT ( 'NONE',  ( 121.3395553409046670, -299.5541904835127980, -198.1000099699160444 ) ) ;
#27858 = CARTESIAN_POINT ( 'NONE',  ( -111.2537441628948045, -292.0111517702345054, -250.1862362095788512 ) ) ;
#27860 = CARTESIAN_POINT ( 'NONE',  ( -33.50843596152530068, -292.1017104308021999, -197.4493385235594189 ) ) ;
#27859 = CARTESIAN_POINT ( 'NONE',  ( 35.40392965850670493, -279.3201327872214392, -250.6530238920276474 ) ) ;
#27861 = CARTESIAN_POINT ( 'NONE',  ( 21.97070697205877465, -280.8920786936284344, -221.2587925387763050 ) ) ;
#27862 = CARTESIAN_POINT ( 'NONE',  ( 6.909384276224850296, -282.1350184663884306, -333.4150734688782336 ) ) ;
#27863 = CARTESIAN_POINT ( 'NONE',  ( 34.18854243352146938, -285.2605713027791126, -247.7697927691642121 ) ) ;
#27864 = CARTESIAN_POINT ( 'NONE',  ( 35.43702946269367970, -279.8823841023202590, -285.0578981763972024 ) ) ;
#27865 = CARTESIAN_POINT ( 'NONE',  ( -82.06236911663238232, -283.4427157167420432, -210.0878805667496749 ) ) ;
#27866 = CARTESIAN_POINT ( 'NONE',  ( 19.62410622756333467, -279.3373208916834756, -219.5713490923693598 ) ) ;
#27867 = AXIS2_PLACEMENT_3D ( 'NONE', #59647, #31673, #81381 ) ;
#27868 = CARTESIAN_POINT ( 'NONE',  ( 29.86732314095164398, -285.9909378734185452, -233.3125708335854256 ) ) ;
#27869 = CARTESIAN_POINT ( 'NONE',  ( -11.44260362485885807, -275.2010569009327128, -201.8829939542681871 ) ) ;
#27870 = CARTESIAN_POINT ( 'NONE',  ( 195.1853111624926385, 40.37665348939848542, 15.05924827439051406 ) ) ;
#27871 = CARTESIAN_POINT ( 'NONE',  ( 36.50864150966231847, -295.1572839987191514, -270.7439568554125344 ) ) ;
#27872 = CARTESIAN_POINT ( 'NONE',  ( -2.839963049624011138, -275.9243922329022212, -202.1685529839888886 ) ) ;
#27873 = CARTESIAN_POINT ( 'NONE',  ( -45.91479224835151030, -276.8304283633519844, -342.9278917448578454 ) ) ;
#27874 = CARTESIAN_POINT ( 'NONE',  ( -92.81355847828376682, -291.4505834663241330, -216.8823302304002709 ) ) ;
#27875 = CARTESIAN_POINT ( 'NONE',  ( 24.73310678854785394, -280.2122656931841789, -313.4655595692692032 ) ) ;
#27876 = VECTOR ( 'NONE', #77752, 1000.000000000000114 ) ;
#27877 = CARTESIAN_POINT ( 'NONE',  ( -79.59264351942204030, -291.3319410763273822, -205.9245798495138615 ) ) ;
#27878 = EDGE_CURVE ( 'NONE', #33307, #86528, #29133, .T. ) ;
#27879 = CARTESIAN_POINT ( 'NONE',  ( -89.97712714218947383, -290.3443895934769898, -219.4403926232700712 ) ) ;
#27880 = CARTESIAN_POINT ( 'NONE',  ( -33.56179022501933673, -293.0044396263564295, -345.2785891142985406 ) ) ;
#27881 = ORIENTED_EDGE ( 'NONE', *, *, #63185, .F. ) ;
#27882 = CARTESIAN_POINT ( 'NONE',  ( 197.2116943569230045, 215.0000000000000568, -12.42446933126075592 ) ) ;
#27883 = AXIS2_PLACEMENT_3D ( 'NONE', #82418, #30844, #9975 ) ;
#27884 = CARTESIAN_POINT ( 'NONE',  ( 32.68986847843369503, -292.7823885402426640, -249.3644386981601997 ) ) ;
#27885 = CARTESIAN_POINT ( 'NONE',  ( 138.6539576904058606, 250.0000000000000568, 10.50000000000000000 ) ) ;
#27886 = CARTESIAN_POINT ( 'NONE',  ( -107.3417001280813565, -270.0523547857346784, -270.3292895737509980 ) ) ;
#27887 = CARTESIAN_POINT ( 'NONE',  ( -104.4032088572309078, -295.1238861540036282, -307.8271991359120534 ) ) ;
#27888 = CARTESIAN_POINT ( 'NONE',  ( -106.5523595750212564, -285.4469594962887982, -302.9676033856445656 ) ) ;
#27889 = CARTESIAN_POINT ( 'NONE',  ( 20.34195925106324054, -286.7553234639853486, -225.6219243692896441 ) ) ;
#27890 = CARTESIAN_POINT ( 'NONE',  ( 34.17742584323769961, -276.8400064867641390, -252.5925396873911950 ) ) ;
#27891 = CARTESIAN_POINT ( 'NONE',  ( -112.0192357161708401, -294.5940575145658613, -268.6710504015970287 ) ) ;
#27892 = CARTESIAN_POINT ( 'NONE',  ( -111.3977033364850229, -298.2974729872357784, -271.5007827338120592 ) ) ;
#27893 = AXIS2_PLACEMENT_3D ( 'NONE', #49296, #25631, #13329 ) ;
#27894 = CARTESIAN_POINT ( 'NONE',  ( 33.96868166395599786, -274.5757362630392322, -287.7910098152834735 ) ) ;
#27895 = ORIENTED_EDGE ( 'NONE', *, *, #1952, .F. ) ;
#27896 = CARTESIAN_POINT ( 'NONE',  ( 195.4781563537916043, 39.36132622696000283, 14.00000000000000000 ) ) ;
#27897 = CARTESIAN_POINT ( 'NONE',  ( -81.86293117527280572, -295.3068547626938880, -333.2243483208449675 ) ) ;
#27898 = CARTESIAN_POINT ( 'NONE',  ( 26.95187574008452813, -289.9784902834215359, -307.9817439055210002 ) ) ;
#27899 = CARTESIAN_POINT ( 'NONE',  ( -46.71249304810552871, -295.9331539542798737, -195.8971521768887385 ) ) ;
#27900 = ADVANCED_FACE ( 'NONE', ( #13878 ), #26067, .T. ) ;
#27901 = CARTESIAN_POINT ( 'NONE',  ( -66.36187284109030315, -290.0937235665642788, -337.5100811796905305 ) ) ;
#27902 = EDGE_LOOP ( 'NONE', ( #63936, #20529, #68374, #62739, #28716 ) ) ;
#27903 = CARTESIAN_POINT ( 'NONE',  ( 12.84741377223365610, -279.7916940393914729, -212.2760677698064455 ) ) ;
#27904 = CARTESIAN_POINT ( 'NONE',  ( -114.2361169130283685, -297.2129476498462282, -269.6118159258965647 ) ) ;
#27905 = CARTESIAN_POINT ( 'NONE',  ( -111.1091296955568168, -288.9114099761761736, -253.0789936976636341 ) ) ;
#27906 = CARTESIAN_POINT ( 'NONE',  ( -110.3243136509194926, -296.5770805311212825, -294.8413633830983258 ) ) ;
#27907 = CARTESIAN_POINT ( 'NONE',  ( 8.858937544581662493, -293.0391543083448482, -213.7483122041708441 ) ) ;
#27908 = CARTESIAN_POINT ( 'NONE',  ( 199.2174190867142727, 65.99980561011084035, -9.232127820537071372 ) ) ;
#27909 = CYLINDRICAL_SURFACE ( 'NONE', #5450, 4.999999999999986677 ) ;
#27910 = CYLINDRICAL_SURFACE ( 'NONE', #58242, 1.000000000000000888 ) ;
#27911 = CARTESIAN_POINT ( 'NONE',  ( 36.12221546286342999, -289.3337391289682614, -291.0430546115063635 ) ) ;
#27912 = CARTESIAN_POINT ( 'NONE',  ( -117.3452863284742733, -275.1604526064901393, -261.3791111993605227 ) ) ;
#27913 = VERTEX_POINT ( 'NONE', #70708 ) ;
#27914 = CARTESIAN_POINT ( 'NONE',  ( 33.08292177469775908, -280.5063885318763823, -239.4793204938449662 ) ) ;
#27915 = CARTESIAN_POINT ( 'NONE',  ( -83.91633429756087992, -285.6932732906661272, -329.0008965336969595 ) ) ;
#27916 = CARTESIAN_POINT ( 'NONE',  ( -12.87507038858997532, -284.9387818915158732, -197.9733405531459027 ) ) ;
#27917 = CARTESIAN_POINT ( 'NONE',  ( -76.64947980478116563, -287.6625334759774546, -333.5767224956252903 ) ) ;
#27918 = CARTESIAN_POINT ( 'NONE',  ( 33.55740889120653492, -277.0690759643125602, -243.6474170215644222 ) ) ;
#27920 = CARTESIAN_POINT ( 'NONE',  ( -41.04806842016684243, -279.3528599735148532, -197.3532040111178674 ) ) ;
#27919 = CARTESIAN_POINT ( 'NONE',  ( -106.2642072771267721, -278.2303353700393700, -294.5703570492445351 ) ) ;
#27921 = CARTESIAN_POINT ( 'NONE',  ( 38.18527739032933965, -276.4637415639192568, -256.9757010926957719 ) ) ;
#27922 = CARTESIAN_POINT ( 'NONE',  ( -110.1673777833031238, -277.6494193630538234, -246.4351457014333562 ) ) ;
#27923 = CARTESIAN_POINT ( 'NONE',  ( 137.0730373049989055, 179.9819603676357929, -239.3176569815323376 ) ) ;
#27924 = CARTESIAN_POINT ( 'NONE',  ( -81.12604869336394131, -274.4147922157858375, -207.2431406866963073 ) ) ;
#27925 = CARTESIAN_POINT ( 'NONE',  ( 52.70517975663122456, -300.5839879508616832, -193.9289803200042286 ) ) ;
#27926 = CARTESIAN_POINT ( 'NONE',  ( -85.28047601435908120, -286.1948066931273615, -330.5268031993605859 ) ) ;
#27927 = DIRECTION ( 'NONE',  ( 0.000000000000000000, 0.000000000000000000, 1.000000000000000000 ) ) ;
#27928 = CARTESIAN_POINT ( 'NONE',  ( 24.50648177546417728, -289.1737003427390960, -309.7188169580091426 ) ) ;
#27929 = CARTESIAN_POINT ( 'NONE',  ( -23.98633205694595105, -287.9804894034323297, -195.5038196974234381 ) ) ;
#27930 = CARTESIAN_POINT ( 'NONE',  ( 20.43292247756048141, -287.5308739620652432, -315.1696133570176244 ) ) ;
#27931 = CARTESIAN_POINT ( 'NONE',  ( -111.4339028052273619, -283.7997974221494815, -291.0944825380661882 ) ) ;
#27932 = CARTESIAN_POINT ( 'NONE',  ( -2.756337512046009408, -278.9171943879674700, -205.1525110326900290 ) ) ;
#27933 = CARTESIAN_POINT ( 'NONE',  ( 21.30210453034180418, -288.7820913678932584, -224.8444214997742279 ) ) ;
#27934 = CARTESIAN_POINT ( 'NONE',  ( 28.76454254570944258, -280.4705849856101167, -303.0448296655491163 ) ) ;
#27935 = CARTESIAN_POINT ( 'NONE',  ( -68.22954056533076539, -278.7817129990770013, -337.0621727666297716 ) ) ;
#27936 = B_SPLINE_CURVE_WITH_KNOTS ( 'NONE', 3,
 ( #33875, #91617, #55657, #40012, #84510, #4060 ),
 .UNSPECIFIED., .F., .F.,
 ( 4, 2, 4 ),
 ( 1.115630864829514821E-16, 0.0006602105328823850783, 0.001320421065764658484 ),
 .UNSPECIFIED. ) ;
#27937 = CARTESIAN_POINT ( 'NONE',  ( -6.508708559273599370, -274.9607239073000642, -204.1243074254262240 ) ) ;
#27938 = CARTESIAN_POINT ( 'NONE',  ( 27.10240031239158398, -286.8942965839950148, -311.8710490412135528 ) ) ;
#27939 = CARTESIAN_POINT ( 'NONE',  ( 21.49297940993257328, -283.0218273886974316, -319.7841824839669016 ) ) ;
#27940 = CARTESIAN_POINT ( 'NONE',  ( -86.05855980369636882, -284.1993662563010616, -329.9110506979000661 ) ) ;
#27941 = CARTESIAN_POINT ( 'NONE',  ( 21.81318416493202150, -282.3174695549828925, -313.1575103015319428 ) ) ;
#27942 = ORIENTED_EDGE ( 'NONE', *, *, #54431, .T. ) ;
#27943 = ORIENTED_EDGE ( 'NONE', *, *, #46281, .T. ) ;
#27944 = CARTESIAN_POINT ( 'NONE',  ( 156.5191989162425727, 214.5000000000000568, 16.58062614384861178 ) ) ;
#27945 = CARTESIAN_POINT ( 'NONE',  ( 29.28789883055610233, -289.8879691579193718, -306.5375349091719954 ) ) ;
#27946 = CARTESIAN_POINT ( 'NONE',  ( -88.30841731686322760, -290.0403525207105986, -213.3024463314751813 ) ) ;
#27947 = AXIS2_PLACEMENT_3D ( 'NONE', #43106, #87561, #87110 ) ;
#27948 = CARTESIAN_POINT ( 'NONE',  ( -43.48996544767952344, -273.0314699460711267, -197.3334855143597508 ) ) ;
#27949 = CARTESIAN_POINT ( 'NONE',  ( 26.42257728213035506, -293.4678031081490417, -313.3428549522618596 ) ) ;
#27950 = CARTESIAN_POINT ( 'NONE',  ( -94.65561665588371909, -288.3830240674366223, -316.6841438649119027 ) ) ;
#27951 = CARTESIAN_POINT ( 'NONE',  ( 34.08886541240971724, -292.0451003689444178, -289.7908993455463360 ) ) ;
#27952 = CARTESIAN_POINT ( 'NONE',  ( 29.79444020040299179, -289.1557536340848742, -300.1498634024007970 ) ) ;
#27953 = CARTESIAN_POINT ( 'NONE',  ( -69.85430415644619018, -291.9805209788416391, -337.9475929042657754 ) ) ;
#27954 = CARTESIAN_POINT ( 'NONE',  ( -73.44170209349182699, -291.5311599022000451, -336.1161045002704100 ) ) ;
#27955 = CARTESIAN_POINT ( 'NONE',  ( -91.47367761872342840, -289.2840923547162788, -218.1358030738686580 ) ) ;
#27956 = CARTESIAN_POINT ( 'NONE',  ( 24.09585832701573338, -294.9673657744388038, -227.2567852158995265 ) ) ;
#27957 = CARTESIAN_POINT ( 'NONE',  ( -25.11429705045469518, -287.1530173869681448, -198.1023217635853371 ) ) ;
#27958 = CARTESIAN_POINT ( 'NONE',  ( -11.80074132295477440, -294.3839197307498239, -199.6120958487989014 ) ) ;
#27959 = DIRECTION ( 'NONE',  ( 0.000000000000000000, 0.000000000000000000, 1.000000000000000000 ) ) ;
#27960 = DIRECTION ( 'NONE',  ( -0.000000000000000000, 1.000000000000000000, 0.000000000000000000 ) ) ;
#27961 = CARTESIAN_POINT ( 'NONE',  ( -109.4702845331659518, -274.8139039863303310, -248.3680098610322204 ) ) ;
#27962 = VECTOR ( 'NONE', #78002, 1000.000000000000000 ) ;
#27963 = CARTESIAN_POINT ( 'NONE',  ( -92.22183984943048074, -281.8365326743239621, -321.4803014006045601 ) ) ;
#27964 = CARTESIAN_POINT ( 'NONE',  ( -113.4940128995877302, -295.6160217112962982, -280.9973586397013605 ) ) ;
#27965 = CARTESIAN_POINT ( 'NONE',  ( -29.86552482766319372, -272.3879355550705554, -196.7263380488801943 ) ) ;
#27966 = CARTESIAN_POINT ( 'NONE',  ( -54.30538834567294515, -275.3514247613899784, -342.8956506329570288 ) ) ;
#27967 = CARTESIAN_POINT ( 'NONE',  ( -72.10929422892263574, -274.7869768633194099, -205.6643640865797806 ) ) ;
#27968 = CARTESIAN_POINT ( 'NONE',  ( -110.9734164504221781, -297.9626579442078764, -271.4901245234829048 ) ) ;
#27969 = DIRECTION ( 'NONE',  ( -0.000000000000000000, 1.000000000000000000, -0.000000000000000000 ) ) ;
#27970 = CARTESIAN_POINT ( 'NONE',  ( -110.5455347005672166, -297.3403183804243213, -271.4757568934718392 ) ) ;
#27971 = CARTESIAN_POINT ( 'NONE',  ( 201.2104617360081704, 15.00000000000000000, -10.00000000000000000 ) ) ;
#27973 = CARTESIAN_POINT ( 'NONE',  ( -110.1886153916286588, -272.4573627217373541, -264.9113385027636127 ) ) ;
#27972 = CARTESIAN_POINT ( 'NONE',  ( 36.21379865595796588, -285.7822219247698285, -286.7905047154431486 ) ) ;
#27974 = CARTESIAN_POINT ( 'NONE',  ( -65.87736105605257819, -285.6890032763001273, -198.8297203755435305 ) ) ;
#27975 = CARTESIAN_POINT ( 'NONE',  ( 7.535050267258309731, -286.3123054090664255, -207.7509064954122096 ) ) ;
#27976 = CARTESIAN_POINT ( 'NONE',  ( -84.21346412910577328, -299.3910101241331745, -211.3573508217638448 ) ) ;
#27977 = CARTESIAN_POINT ( 'NONE',  ( -66.79765748930917368, -293.4388402721720013, -339.1533777548776811 ) ) ;
#27978 = CARTESIAN_POINT ( 'NONE',  ( -67.29007497460159470, -278.8664542544996721, -199.5991672970455966 ) ) ;
#27979 = CARTESIAN_POINT ( 'NONE',  ( 21.27581636871891391, -291.6952119285919025, -317.1477375740089997 ) ) ;
#27980 = DIRECTION ( 'NONE',  ( 0.000000000000000000, 0.000000000000000000, 1.000000000000000000 ) ) ;
#27981 = CARTESIAN_POINT ( 'NONE',  ( -21.05608060528523851, -287.6334131177407016, -341.9286322635841202 ) ) ;
#27982 = CARTESIAN_POINT ( 'NONE',  ( 200.1411370654279551, 66.37844756382011724, -9.866896536115095984 ) ) ;
#27983 = CARTESIAN_POINT ( 'NONE',  ( -28.97461484905128515, -286.9459128861973909, -344.8929402574292453 ) ) ;
#27984 = CARTESIAN_POINT ( 'NONE',  ( -91.64643365806763597, -274.7806438306192831, -220.5257315113691732 ) ) ;
#27985 = CARTESIAN_POINT ( 'NONE',  ( -19.90843096779035903, -281.6971225055159493, -195.9112900974531613 ) ) ;
#27987 = CARTESIAN_POINT ( 'NONE',  ( 18.49435572935509953, -282.2203537072990116, -317.4053548136532754 ) ) ;
#27986 = CARTESIAN_POINT ( 'NONE',  ( -87.52917990643007329, -293.7681210646803152, -326.6416414990556518 ) ) ;
#27988 = CARTESIAN_POINT ( 'NONE',  ( -103.8508741773613338, -297.2248935143250037, -231.4548793782386156 ) ) ;
#27989 = CARTESIAN_POINT ( 'NONE',  ( -86.57776161076688481, -298.8731386555825793, -215.5293935837487140 ) ) ;
#27990 = CARTESIAN_POINT ( 'NONE',  ( -2.098379140744467186, -282.5189682755772083, -204.1575759557293281 ) ) ;
#27991 = CARTESIAN_POINT ( 'NONE',  ( -94.96597827460345798, -294.9756243184080517, -315.5590274144084901 ) ) ;
#27992 = ORIENTED_EDGE ( 'NONE', *, *, #72204, .F. ) ;
#27993 = DIRECTION ( 'NONE',  ( 0.000000000000000000, 0.000000000000000000, 1.000000000000000000 ) ) ;
#27994 = CARTESIAN_POINT ( 'NONE',  ( -62.05604516651806080, -285.3548235517718012, -340.8502527955778305 ) ) ;
#27995 = DIRECTION ( 'NONE',  ( 0.000000000000000000, 0.000000000000000000, 1.000000000000000000 ) ) ;
#27996 = CARTESIAN_POINT ( 'NONE',  ( -110.4542110544635705, -288.2666405000204577, -253.6410175316879361 ) ) ;
#27997 = CARTESIAN_POINT ( 'NONE',  ( 38.56968178120676782, -274.5991142934987010, -258.3757766717307618 ) ) ;
#27998 = CARTESIAN_POINT ( 'NONE',  ( 12.90469444076323668, -292.6109992374461513, -217.4054777038944621 ) ) ;
#27999 = CARTESIAN_POINT ( 'NONE',  ( 36.04086593327440369, -282.9769203603686947, -263.0636187760797498 ) ) ;
#28000 = CARTESIAN_POINT ( 'NONE',  ( 34.90031361873190718, -276.9546506386490137, -255.2153453687832609 ) ) ;
#28001 = CARTESIAN_POINT ( 'NONE',  ( -37.29624056562353474, -284.4768226468576700, -346.7848434621091656 ) ) ;
#28002 = CARTESIAN_POINT ( 'NONE',  ( 35.91712305628837498, -280.2879916519581229, -265.8583044698336835 ) ) ;
#28003 = CARTESIAN_POINT ( 'NONE',  ( -112.1616053369291279, -280.4765637453513136, -276.2608981042075698 ) ) ;
#28004 = CARTESIAN_POINT ( 'NONE',  ( -36.89686204664280211, -298.0575775464870958, -193.3611179820811401 ) ) ;
#28005 = CARTESIAN_POINT ( 'NONE',  ( 1.045191405193388823, -276.3882277681180426, -337.1707270143655819 ) ) ;
#28006 = CARTESIAN_POINT ( 'NONE',  ( 34.51298934953057795, -295.7248008620028941, -289.8574664704102588 ) ) ;
#28007 = TOROIDAL_SURFACE ( 'NONE', #11350, 1.000000000000000000, 0.5000000000000000000 ) ;
#28008 = DIRECTION ( 'NONE',  ( 0.000000000000000000, 0.000000000000000000, 1.000000000000000000 ) ) ;
#28009 = EDGE_CURVE ( 'NONE', #33307, #47563, #39636, .T. ) ;
#28010 = CARTESIAN_POINT ( 'NONE',  ( -112.5458065890736492, -294.8086773902774098, -261.1606913031427553 ) ) ;
#28011 = CARTESIAN_POINT ( 'NONE',  ( 31.17820085880634551, -274.7219550178333520, -245.0034443843609893 ) ) ;
#28012 = AXIS2_PLACEMENT_3D ( 'NONE', #22751, #33128, #60625 ) ;
#28013 = CARTESIAN_POINT ( 'NONE',  ( 33.81202857369787296, -295.4246590639627925, -297.9265790378584029 ) ) ;
#28014 = CARTESIAN_POINT ( 'NONE',  ( 31.82082319512121416, -294.3314994450817608, -237.3053287517543595 ) ) ;
#28015 = CARTESIAN_POINT ( 'NONE',  ( -81.46852711905823696, -291.6536940049837767, -330.8644088861172463 ) ) ;
#28016 = CARTESIAN_POINT ( 'NONE',  ( -54.39588776401409831, -275.2714312198598350, -343.2787136585802727 ) ) ;
#28017 = CARTESIAN_POINT ( 'NONE',  ( -64.84282839875992011, -279.3341592742543185, -339.5895602522381296 ) ) ;
#28018 = CARTESIAN_POINT ( 'NONE',  ( -42.51371024838580581, -293.1977432530407555, -344.6212318387199502 ) ) ;
#28019 = CARTESIAN_POINT ( 'NONE',  ( 12.88003433711540424, -284.2207523445686093, -327.1591206434434298 ) ) ;
#28020 = CIRCLE ( 'NONE', #64349, 0.5000000000000001110 ) ;
#28021 = CARTESIAN_POINT ( 'NONE',  ( -99.86580070651493202, -283.9988228077532995, -231.9895940736992657 ) ) ;
#28022 = CARTESIAN_POINT ( 'NONE',  ( 140.7777284831114173, 178.7908050832685660, -240.4635850708682199 ) ) ;
#28023 = ORIENTED_EDGE ( 'NONE', *, *, #80614, .T. ) ;
#28024 = CARTESIAN_POINT ( 'NONE',  ( -104.1343511845896046, -283.8218535153925473, -299.8709341718724772 ) ) ;
#28025 = ORIENTED_EDGE ( 'NONE', *, *, #6914, .T. ) ;
#28026 = CARTESIAN_POINT ( 'NONE',  ( 29.01222710156249107, -282.1297269839663500, -231.9079146012832950 ) ) ;
#28027 = CARTESIAN_POINT ( 'NONE',  ( -113.9582448744078391, -283.3161530564225927, -272.8210911669781922 ) ) ;
#28028 = CARTESIAN_POINT ( 'NONE',  ( -95.73465106590919049, -280.1677410188584645, -220.5103765501183659 ) ) ;
#28029 =( NAMED_UNIT ( * ) PLANE_ANGLE_UNIT ( ) SI_UNIT ( $, .RADIAN. ) );
#28030 = CARTESIAN_POINT ( 'NONE',  ( -113.0756255427715757, -279.9492366175376787, -280.1102947509685350 ) ) ;
#28031 = CARTESIAN_POINT ( 'NONE',  ( -37.30987171927208124, -297.5519495502701375, -340.3611179825599606 ) ) ;
#28032 = CARTESIAN_POINT ( 'NONE',  ( 198.4579507164851009, 284.8021970988023099, -111.8421920981697468 ) ) ;
#28033 = ORIENTED_EDGE ( 'NONE', *, *, #53026, .T. ) ;
#28034 = CARTESIAN_POINT ( 'NONE',  ( -110.9373293241335432, -274.7303055138964396, -256.5293980630806345 ) ) ;
#28035 = CARTESIAN_POINT ( 'NONE',  ( 175.2296996224750103, 160.0000000000000568, 24.00000000000001066 ) ) ;
#28036 = CARTESIAN_POINT ( 'NONE',  ( -94.32997554917086802, -277.2425367033696944, -222.1316811135891953 ) ) ;
#28037 = CARTESIAN_POINT ( 'NONE',  ( -94.90809356893018389, -292.9911176452388304, -220.7419850043174847 ) ) ;
#28038 = CARTESIAN_POINT ( 'NONE',  ( 30.92654188914169922, -292.5521051785483451, -244.2203490601783358 ) ) ;
#28039 = CARTESIAN_POINT ( 'NONE',  ( -46.02505861133587928, -288.6669869282663967, -346.8610871995458069 ) ) ;
#28040 = CARTESIAN_POINT ( 'NONE',  ( -5.802570524182335987, -229.5268262511776527, 25.50000000000000000 ) ) ;
#28042 = CARTESIAN_POINT ( 'NONE',  ( 5.203008780962274038, -285.0377962690827758, -209.9960987087968078 ) ) ;
#28041 = CARTESIAN_POINT ( 'NONE',  ( 12.99392934457449478, -292.9403333033848185, -327.9197831423583125 ) ) ;
#28043 = CARTESIAN_POINT ( 'NONE',  ( -80.26387722345732811, -293.3247882169677041, -209.7295227356470377 ) ) ;
#28044 = CARTESIAN_POINT ( 'NONE',  ( 31.82436773254024942, -283.1977697238015139, -295.3571764910120123 ) ) ;
#28045 = ORIENTED_EDGE ( 'NONE', *, *, #84612, .F. ) ;
#28046 = CARTESIAN_POINT ( 'NONE',  ( -111.4089442134200141, -291.7473706602705761, -250.1403505333659041 ) ) ;
#28047 = CARTESIAN_POINT ( 'NONE',  ( 9.311019555255182212, -281.2054999386868417, -214.0678468630394775 ) ) ;
#28048 = CARTESIAN_POINT ( 'NONE',  ( 22.85009222728621481, -292.9842291068742384, -317.7631340231550325 ) ) ;
#28049 = CARTESIAN_POINT ( 'NONE',  ( -40.32223792881935509, -289.8915235689477754, -347.1548679513696811 ) ) ;
#28050 = CARTESIAN_POINT ( 'NONE',  ( -75.62761341090129008, -290.0412110251078275, -337.0972831956987079 ) ) ;
#28051 = CARTESIAN_POINT ( 'NONE',  ( 30.48597157529096080, -288.0815754236534190, -297.4864780855438084 ) ) ;
#28052 = EDGE_LOOP ( 'NONE', ( #5054, #55514, #80394, #81443 ) ) ;
#28053 = CARTESIAN_POINT ( 'NONE',  ( 194.8650209881936064, 26.44696541833617687, 13.81479162729918997 ) ) ;
#28054 = CARTESIAN_POINT ( 'NONE',  ( -1.272993729137065877, -296.4394104881654357, -337.0042431845305373 ) ) ;
#28055 = CARTESIAN_POINT ( 'NONE',  ( -112.1149302435014476, -295.4415447471848779, -254.1055185902897904 ) ) ;
#28056 = CARTESIAN_POINT ( 'NONE',  ( -89.26106157956098741, -276.8634653042522586, -322.0837801763900075 ) ) ;
#28057 = CARTESIAN_POINT ( 'NONE',  ( -95.03617356095902835, -272.7495893077818323, -219.4604830293382633 ) ) ;
#28058 = CARTESIAN_POINT ( 'NONE',  ( -86.97105768655656277, -294.2380822046523008, -324.8371183800423410 ) ) ;
#28059 = CARTESIAN_POINT ( 'NONE',  ( 23.87807793721375305, -276.7414679868615508, -228.7437702527872716 ) ) ;
#28060 = CARTESIAN_POINT ( 'NONE',  ( -47.38841827234107740, -296.1627301703168769, -196.9809126923687757 ) ) ;
#28061 = CARTESIAN_POINT ( 'NONE',  ( 19.14848069100017369, -295.4182486591070074, -317.2225090953092490 ) ) ;
#28062 = CARTESIAN_POINT ( 'NONE',  ( -92.41384093303166480, -296.9439873335218749, -318.7479486428186988 ) ) ;
#28063 = DIRECTION ( 'NONE',  ( -0.000000000000000000, -1.000000000000000000, -0.000000000000000000 ) ) ;
#28064 = CARTESIAN_POINT ( 'NONE',  ( -14.00744866198116156, -296.3544873044916130, -342.9004391991400666 ) ) ;
#28065 = CARTESIAN_POINT ( 'NONE',  ( -107.7299518214646241, -294.2085732513149310, -296.8808627079519624 ) ) ;
#28066 = CARTESIAN_POINT ( 'NONE',  ( -37.26203148652085417, -298.7045363509798790, -193.4622787378366411 ) ) ;
#28067 = CARTESIAN_POINT ( 'NONE',  ( 24.72565874737504643, -286.6691604813794356, -309.8961389004255693 ) ) ;
#28068 = CARTESIAN_POINT ( 'NONE',  ( -106.2264664317372791, -274.9418047100177773, -240.5664689719322098 ) ) ;
#28069 = CARTESIAN_POINT ( 'NONE',  ( -63.54203524777665990, -274.2119788028431344, -198.0211612311889269 ) ) ;
#28070 = EDGE_CURVE ( 'NONE', #44324, #46709, #51752, .T. ) ;
#28071 = CARTESIAN_POINT ( 'NONE',  ( -92.76322366191756430, -297.5622419110973738, -222.7967240744494006 ) ) ;
#28072 = EDGE_CURVE ( 'NONE', #75355, #76874, #63907, .T. ) ;
#28073 = CARTESIAN_POINT ( 'NONE',  ( -69.28850980877456323, -281.6138905431190551, -202.0988976426890531 ) ) ;
#28074 = CARTESIAN_POINT ( 'NONE',  ( -19.85257429741055901, -278.9571171680595398, -195.8256322199339934 ) ) ;
#28075 = CARTESIAN_POINT ( 'NONE',  ( 2.034808907305420078, -281.8880808434401501, -336.4126381976352036 ) ) ;
#28076 = CARTESIAN_POINT ( 'NONE',  ( 38.82435768319805902, -274.7681843432404207, -259.7760141078702532 ) ) ;
#28077 = CARTESIAN_POINT ( 'NONE',  ( 32.44849175900301219, -279.5578260653259690, -239.7707677089753702 ) ) ;
#28078 = CARTESIAN_POINT ( 'NONE',  ( 11.81297834089748733, -278.7329559869243099, -213.4942030997031850 ) ) ;
#28079 = CARTESIAN_POINT ( 'NONE',  ( -0.2335894197411676199, -273.1307780190336416, -206.7982915321937014 ) ) ;
#28080 = CARTESIAN_POINT ( 'NONE',  ( 36.25921273462058281, -277.7382913887556128, -284.8457121460251074 ) ) ;
#28081 = CARTESIAN_POINT ( 'NONE',  ( 223.4306832106270804, -135.2391364535880882, -21.50000000000000000 ) ) ;
#28082 = CARTESIAN_POINT ( 'NONE',  ( -110.6385569029122848, -295.0485713668923040, -250.1283228783588015 ) ) ;
#28083 = CARTESIAN_POINT ( 'NONE',  ( -7.811030919525538074, -290.4572835550393961, -201.0192816191308793 ) ) ;
#28084 = CARTESIAN_POINT ( 'NONE',  ( -16.62661434677074368, -292.3126276128176073, -196.1999069550090553 ) ) ;
#28085 = PRODUCT_DEFINITION_FORMATION_WITH_SPECIFIED_SOURCE ( 'ANY', '', #64119, .NOT_KNOWN. ) ;
#28086 = CARTESIAN_POINT ( 'NONE',  ( -26.02034839420548451, -278.9084648971136176, -344.6703059690834721 ) ) ;
#28087 = CARTESIAN_POINT ( 'NONE',  ( -24.22220845655590793, -272.2193692862254011, -196.4644972783399908 ) ) ;
#28088 = FACE_OUTER_BOUND ( 'NONE', #56696, .T. ) ;
#28089 = CARTESIAN_POINT ( 'NONE',  ( 10.59821394562014163, -284.3163988261264876, -328.8332841813749496 ) ) ;
#28090 = SURFACE_SIDE_STYLE ('',( #91981 ) ) ;
#28091 = CARTESIAN_POINT ( 'NONE',  ( -57.85746960201582567, -283.7871510016461798, -198.1684539808781835 ) ) ;
#28092 = CARTESIAN_POINT ( 'NONE',  ( 197.4027394742815602, 40.84896208771628068, 12.00000000000000000 ) ) ;
#28093 = CARTESIAN_POINT ( 'NONE',  ( 27.50171581107858998, -292.8142785873861840, -304.8566253971574724 ) ) ;
#28094 = CARTESIAN_POINT ( 'NONE',  ( -11.57134551548542767, -284.5309734624110547, -200.7424832421526446 ) ) ;
#28095 = CARTESIAN_POINT ( 'NONE',  ( 157.4787282879766508, 15.38390992556615622, -9.006389530800271714 ) ) ;
#28096 = CARTESIAN_POINT ( 'NONE',  ( -9.778035230499003916, -292.6919539700308519, -340.1124264062586349 ) ) ;
#28097 = CARTESIAN_POINT ( 'NONE',  ( -99.23754676277074793, -282.4339519434785188, -315.0769286375563070 ) ) ;
#28098 = CARTESIAN_POINT ( 'NONE',  ( -100.1592769896655142, -280.6817413980896845, -231.5286852455453186 ) ) ;
#28099 = CARTESIAN_POINT ( 'NONE',  ( -78.32305721756537764, -286.7188482332049375, -205.6422097011765686 ) ) ;
#28100 = CARTESIAN_POINT ( 'NONE',  ( 38.40341063769719199, -279.7152870788160044, -264.3070113555457397 ) ) ;
#28101 = CARTESIAN_POINT ( 'NONE',  ( 15.97446700786748686, -286.8346201214483813, -220.4789939989699121 ) ) ;
#28102 = CARTESIAN_POINT ( 'NONE',  ( -45.95922735717458352, -278.5886984747362476, -343.4950714331884569 ) ) ;
#28103 = CARTESIAN_POINT ( 'NONE',  ( -83.09980543342778958, -278.4997163134779044, -327.5121914353359784 ) ) ;
#28104 = CARTESIAN_POINT ( 'NONE',  ( -70.36858769287958637, -287.5988760299284763, -202.6290612783738538 ) ) ;
#28105 = ORIENTED_EDGE ( 'NONE', *, *, #30387, .T. ) ;
#28106 = CARTESIAN_POINT ( 'NONE',  ( -33.33235367113654490, -297.9343723149041807, -193.3612275890083652 ) ) ;
#28107 = CARTESIAN_POINT ( 'NONE',  ( 37.19341873245248564, -289.4687431499712602, -265.4540040888338694 ) ) ;
#28108 = CARTESIAN_POINT ( 'NONE',  ( 197.5379522065468052, 276.0000000000000568, -11.97918851819043873 ) ) ;
#28109 = CARTESIAN_POINT ( 'NONE',  ( -55.56934967048406548, -285.7662352645559736, -350.3683826091709648 ) ) ;
#28110 = ORIENTED_EDGE ( 'NONE', *, *, #46184, .T. ) ;
#28111 = CARTESIAN_POINT ( 'NONE',  ( -34.15480953538573061, -272.0919910463347264, -195.2620357165949088 ) ) ;
#28112 = CARTESIAN_POINT ( 'NONE',  ( 36.31795925728029317, -292.1988635904641001, -289.8725248096885707 ) ) ;
#28113 = CARTESIAN_POINT ( 'NONE',  ( -52.64186249299973497, -297.3585942447999173, -198.8676508325147552 ) ) ;
#28114 = CARTESIAN_POINT ( 'NONE',  ( -19.66814652079286319, -287.8036951470864437, -198.8184506195497647 ) ) ;
#28115 = CARTESIAN_POINT ( 'NONE',  ( -22.00602838502867087, -282.0113298568033997, -197.9014226922296587 ) ) ;
#28116 = CARTESIAN_POINT ( 'NONE',  ( -17.85693358336884984, -290.2309328392287853, -344.2458265767364765 ) ) ;
#28117 = CARTESIAN_POINT ( 'NONE',  ( -89.14518610396103782, -291.0781396373813550, -326.6611811480674419 ) ) ;
#28118 = CARTESIAN_POINT ( 'NONE',  ( -95.82909910700773537, -285.9062825093197375, -317.3307111817943564 ) ) ;
#28119 = CARTESIAN_POINT ( 'NONE',  ( -75.33435227619870034, -277.7109374176577035, -337.3354293807615818 ) ) ;
#28120 = CARTESIAN_POINT ( 'NONE',  ( -39.09932026000416272, -293.1538992842187099, -345.9006769748923489 ) ) ;
#28121 = CARTESIAN_POINT ( 'NONE',  ( -4.942056552631748367, -280.3004092114634318, -200.5093957366760549 ) ) ;
#28122 = CARTESIAN_POINT ( 'NONE',  ( -106.5766844540482623, -274.7661600914407245, -243.4352046824957654 ) ) ;
#28123 = CARTESIAN_POINT ( 'NONE',  ( 35.77081079830085031, -283.8376638359844719, -253.6410175316879361 ) ) ;
#28124 = CARTESIAN_POINT ( 'NONE',  ( 38.36892465339373359, -273.8740213224252784, -276.8322312763607442 ) ) ;
#28125 = DIRECTION ( 'NONE',  ( 0.000000000000000000, 1.000000000000000000, -1.224646799147353207E-16 ) ) ;
#28126 = CARTESIAN_POINT ( 'NONE',  ( 20.22558858948192650, -281.6934121598234810, -315.3499578384507913 ) ) ;
#28127 = CARTESIAN_POINT ( 'NONE',  ( -103.2562580389043205, -279.2449484700624112, -309.4943211881104048 ) ) ;
#28128 = CARTESIAN_POINT ( 'NONE',  ( -65.81734592743688950, -299.0974448382855826, -202.5045596089376261 ) ) ;
#28129 = CARTESIAN_POINT ( 'NONE',  ( -75.97789731365388377, -284.6084101304830369, -203.9669286006616460 ) ) ;
#28130 = CARTESIAN_POINT ( 'NONE',  ( -95.73641430247434414, -291.6800915229406996, -315.8571982698352372 ) ) ;
#28131 = CARTESIAN_POINT ( 'NONE',  ( -112.2852903574929542, -274.3299928845239606, -256.2986304240960749 ) ) ;
#28132 = CARTESIAN_POINT ( 'NONE',  ( -38.36770459288386093, -275.3547103246697816, -193.8611468089742971 ) ) ;
#28133 = DIRECTION ( 'NONE',  ( -0.000000000000000000, -1.000000000000000000, -0.000000000000000000 ) ) ;
#28134 = CARTESIAN_POINT ( 'NONE',  ( -48.03033188651542673, -297.1884613269500051, -344.4797458317314636 ) ) ;
#28135 = CARTESIAN_POINT ( 'NONE',  ( -45.87315631982862385, -281.1602700852100725, -344.7588222751869012 ) ) ;
#28136 = CARTESIAN_POINT ( 'NONE',  ( -95.64212420531865178, -290.8980335871908096, -220.0736377485097535 ) ) ;
#28137 = CARTESIAN_POINT ( 'NONE',  ( 12.66675576639619649, -272.7732058343387394, -214.8748835000687052 ) ) ;
#28138 = CARTESIAN_POINT ( 'NONE',  ( -10.29715296642566535, -287.9992811074804990, -199.0656487114469257 ) ) ;
#28139 = CARTESIAN_POINT ( 'NONE',  ( -79.69814407969313663, -290.3851741328182925, -210.4644847016560902 ) ) ;
#28140 = ORIENTED_EDGE ( 'NONE', *, *, #41040, .F. ) ;
#28141 = CARTESIAN_POINT ( 'NONE',  ( -103.2990538180395248, -288.6197473780759992, -309.0434482503382583 ) ) ;
#28142 = CARTESIAN_POINT ( 'NONE',  ( -81.73853767321745067, -291.0954685806805173, -212.3229330168005333 ) ) ;
#28143 = EDGE_LOOP ( 'NONE', ( #74531, #83062, #34521, #32904 ) ) ;
#28144 = CARTESIAN_POINT ( 'NONE',  ( 34.55962938336060120, -288.2931712937298130, -243.6835745483854794 ) ) ;
#28145 = CARTESIAN_POINT ( 'NONE',  ( 5.412601320327937948, -276.7890038939988244, -329.6194828118274245 ) ) ;
#28146 = CARTESIAN_POINT ( 'NONE',  ( 0.3764463079797041867, -293.4822351244868059, -337.1507359201993381 ) ) ;
#28147 = CARTESIAN_POINT ( 'NONE',  ( -21.73855640299023406, -283.5086081065511507, -345.6595554973395110 ) ) ;
#28148 = CARTESIAN_POINT ( 'NONE',  ( -46.50719114211967309, -286.2721241826269534, -193.9298543141706546 ) ) ;
#28149 = CARTESIAN_POINT ( 'NONE',  ( 26.87565952756503762, -282.3595616613027914, -305.1205513143564190 ) ) ;
#28150 = CARTESIAN_POINT ( 'NONE',  ( 25.26796030052132025, -22.82892349226261075, -345.1428209926129966 ) ) ;
#28151 = CARTESIAN_POINT ( 'NONE',  ( -57.31220355042948000, -168.7168211105807529, -363.3665416233598648 ) ) ;
#28152 = CARTESIAN_POINT ( 'NONE',  ( 83.65573564170013299, 82.10386166810425834, -298.8792467998813436 ) ) ;
#28153 = CARTESIAN_POINT ( 'NONE',  ( -40.77230168148079770, -273.2052034312633282, -197.2303059850570151 ) ) ;
#28154 = CARTESIAN_POINT ( 'NONE',  ( 34.13822505986901490, -274.2580367448811671, -254.0308445503238772 ) ) ;
#28155 = CARTESIAN_POINT ( 'NONE',  ( -90.67393958100727502, -295.2912265906286393, -325.8889516326451030 ) ) ;
#28156 = CARTESIAN_POINT ( 'NONE',  ( -81.85735553743283788, -219.3983098388335691, -349.3051352687708686 ) ) ;
#28157 = CARTESIAN_POINT ( 'NONE',  ( -18.65411271695536044, -272.9726401196645043, -196.1170019598329475 ) ) ;
#28158 = CARTESIAN_POINT ( 'NONE',  ( -109.7922860182429048, -298.2026840404762424, -286.5406757052586499 ) ) ;
#28159 = CARTESIAN_POINT ( 'NONE',  ( -39.95886001895915030, -290.4007690617337971, -343.8575672787906683 ) ) ;
#28160 = CARTESIAN_POINT ( 'NONE',  ( -108.4115248816573001, -291.8687437960538773, -252.3293109300332446 ) ) ;
#28161 = EDGE_LOOP ( 'NONE', ( #63326, #82721, #89690, #20690, #59841, #66887 ) ) ;
#28162 = CARTESIAN_POINT ( 'NONE',  ( -51.76818457096969439, -298.8132971490065870, -194.9100150582193010 ) ) ;
#28163 = CIRCLE ( 'NONE', #62975, 4.025000000000000355 ) ;
#28164 = CARTESIAN_POINT ( 'NONE',  ( -0.9553561296519736956, -289.0478212563090779, -333.7756677901251123 ) ) ;
#28165 = CARTESIAN_POINT ( 'NONE',  ( 23.90646584971814192, -294.9744124262732043, -316.7596199564286508 ) ) ;
#28166 = CARTESIAN_POINT ( 'NONE',  ( -0.7299311085422596213, -295.0715627795631235, -338.0450784592586047 ) ) ;
#28167 = CARTESIAN_POINT ( 'NONE',  ( 29.49090886667639921, -294.1139096438990350, -299.7278062438883239 ) ) ;
#28168 = ORIENTED_EDGE ( 'NONE', *, *, #33819, .T. ) ;
#28169 = CARTESIAN_POINT ( 'NONE',  ( 15.95714609906237058, -278.2245376995158495, -323.9930235821350379 ) ) ;
#28170 = ORIENTED_EDGE ( 'NONE', *, *, #17248, .F. ) ;
#28171 = CARTESIAN_POINT ( 'NONE',  ( -79.87153957028512252, -279.0016068032708176, -206.1821622566758379 ) ) ;
#28172 = CARTESIAN_POINT ( 'NONE',  ( 35.61146836546884487, -276.4016974978463850, -263.3864527957813380 ) ) ;
#28173 = CARTESIAN_POINT ( 'NONE',  ( -43.97691090012794035, -275.7296400576510678, -194.6120907048616289 ) ) ;
#28174 = CARTESIAN_POINT ( 'NONE',  ( 29.08106880941043215, -274.0435382624835938, -306.0580591023386887 ) ) ;
#28175 = CARTESIAN_POINT ( 'NONE',  ( -107.9362574306327929, -297.4545039448234434, -251.3312609251844947 ) ) ;
#28176 = CARTESIAN_POINT ( 'NONE',  ( -101.9935680215305212, -294.6509622677120319, -305.5109528833190211 ) ) ;
#28177 = CARTESIAN_POINT ( 'NONE',  ( 144.2857639756989272, -299.5541904835127980, -202.0153591320744226 ) ) ;
#28178 = CARTESIAN_POINT ( 'NONE',  ( -114.3163711564752134, -279.0647664114617896, -268.7418033755333795 ) ) ;
#28179 = EDGE_CURVE ( 'NONE', #12173, #69141, #78735, .T. ) ;
#28180 = CARTESIAN_POINT ( 'NONE',  ( -6.274698393131096452, -276.7989492697439005, -336.4342645810056638 ) ) ;
#28181 = CARTESIAN_POINT ( 'NONE',  ( 28.28420850146423859, -285.7196752927730472, -230.9328562144431771 ) ) ;
#28182 = CARTESIAN_POINT ( 'NONE',  ( -112.3417001280813992, -274.5519907608264134, -270.3865269787834222 ) ) ;
#28183 = DIRECTION ( 'NONE',  ( 0.000000000000000000, 0.000000000000000000, 1.000000000000000000 ) ) ;
#28184 = CARTESIAN_POINT ( 'NONE',  ( 32.43066532167586757, -286.4577060278090244, -248.3096427053020818 ) ) ;
#28185 = CARTESIAN_POINT ( 'NONE',  ( -24.68131805288838265, -278.4557568257499156, -197.4386335419287093 ) ) ;
#28186 = CARTESIAN_POINT ( 'NONE',  ( -107.7859579568138173, -277.4064100955260983, -249.0777569567908358 ) ) ;
#28187 = CARTESIAN_POINT ( 'NONE',  ( -89.23430503325336360, -285.7820398157825821, -324.5815481743356372 ) ) ;
#28188 = CARTESIAN_POINT ( 'NONE',  ( -43.22369394126268816, -278.3331605554121211, -343.5221229904959728 ) ) ;
#28189 = CARTESIAN_POINT ( 'NONE',  ( 196.1963538710215857, 305.7026273589066250, 13.99999999999999112 ) ) ;
#28190 = CARTESIAN_POINT ( 'NONE',  ( -8.293032212393173452, -274.9168698057608822, -340.5902317083035200 ) ) ;
#28191 = CARTESIAN_POINT ( 'NONE',  ( -43.49896903086576572, -274.6238782417506741, -197.4681732426494136 ) ) ;
#28192 = CARTESIAN_POINT ( 'NONE',  ( 35.77123290750189000, -283.7765328698089320, -287.8668151835400977 ) ) ;
#28193 = LINE ( 'NONE', #35279, #47398 ) ;
#28194 = CARTESIAN_POINT ( 'NONE',  ( 37.91545077661244534, -289.5584402653669827, -277.1194782840451012 ) ) ;
#28195 = B_SPLINE_CURVE_WITH_KNOTS ( 'NONE', 3,
 ( #22932, #80235, #52732, #81615, #43772, #79774 ),
 .UNSPECIFIED., .F., .F.,
 ( 4, 2, 4 ),
 ( 0.000000000000000000, 0.0009572278725339521555, 0.001914455745067904311 ),
 .UNSPECIFIED. ) ;
#28196 = CARTESIAN_POINT ( 'NONE',  ( -48.22273983581821710, -289.9136607298749482, -196.1027513855873394 ) ) ;
#28197 = CARTESIAN_POINT ( 'NONE',  ( 175.2296996224750103, 214.5000000000000568, 0.000000000000000000 ) ) ;
#28198 = CARTESIAN_POINT ( 'NONE',  ( 21.08370160627710987, -273.6139865770130655, -225.7565898271020046 ) ) ;
#28199 = CARTESIAN_POINT ( 'NONE',  ( 36.85665640478975291, -291.6613916260426436, -268.0224505403757576 ) ) ;
#28200 = CARTESIAN_POINT ( 'NONE',  ( 28.92138380700103895, -24.05900251067409457, -347.7894294321414463 ) ) ;
#28201 = CARTESIAN_POINT ( 'NONE',  ( 199.7700033442230279, 63.22432295887224285, -10.15684170342041703 ) ) ;
#28202 = CARTESIAN_POINT ( 'NONE',  ( -91.12372321394828134, -288.2790271934700286, -324.5668051599027990 ) ) ;
#28203 = CARTESIAN_POINT ( 'NONE',  ( -70.55692872783261294, -285.0977153088188061, -336.2781237141655879 ) ) ;
#28204 = CARTESIAN_POINT ( 'NONE',  ( 36.51413064112026774, -286.0191328881043660, -288.2847123187141278 ) ) ;
#28205 = CARTESIAN_POINT ( 'NONE',  ( -64.25409643154559092, -284.8356200401500473, -338.8527075587416562 ) ) ;
#28206 = CARTESIAN_POINT ( 'NONE',  ( -69.06996289883772988, -284.2832992851155609, -336.2985353886234634 ) ) ;
#28207 = CARTESIAN_POINT ( 'NONE',  ( -37.81064810741841598, -294.0261927356572187, -195.0073729177867108 ) ) ;
#28208 = CARTESIAN_POINT ( 'NONE',  ( 28.70103266055255276, -273.1458537488143179, -233.5428177046572387 ) ) ;
#28209 = CARTESIAN_POINT ( 'NONE',  ( -1.315148466027089347, -274.8500468257770990, -202.3329483252103103 ) ) ;
#28210 = CARTESIAN_POINT ( 'NONE',  ( -111.4603495875456218, -288.4439694074263230, -285.1148957839625950 ) ) ;
#28211 = CARTESIAN_POINT ( 'NONE',  ( -77.81490168422480735, -277.5794856372182835, -335.9281926935486808 ) ) ;
#28212 = CARTESIAN_POINT ( 'NONE',  ( 28.62316312046310429, -295.9987339488381508, -305.4070589946056202 ) ) ;
#28213 = CARTESIAN_POINT ( 'NONE',  ( 170.2331121529641678, 214.9642003054772488, -24.76688354601320441 ) ) ;
#28214 = CARTESIAN_POINT ( 'NONE',  ( -4.771743288812468897, -297.1233781216987495, -337.9199732462171255 ) ) ;
#28215 = CARTESIAN_POINT ( 'NONE',  ( -94.68021586434736037, -282.5914848497494063, -316.3543759677571643 ) ) ;
#28216 = CARTESIAN_POINT ( 'NONE',  ( -9.577188976701833667, -278.4147702638450141, -200.6895127905459901 ) ) ;
#28217 = CARTESIAN_POINT ( 'NONE',  ( 186.6539576904058890, 293.9636489450775230, 11.60392986742922439 ) ) ;
#28218 = CARTESIAN_POINT ( 'NONE',  ( -102.1201425696595919, -271.5644569664745518, -230.0317100195215971 ) ) ;
#28219 = CARTESIAN_POINT ( 'NONE',  ( -76.41730650169333217, -276.9381154945092476, -332.2024458730276137 ) ) ;
#28220 = CARTESIAN_POINT ( 'NONE',  ( 29.35789448925144995, -294.6515473460921157, -238.9059162442042634 ) ) ;
#28221 = CARTESIAN_POINT ( 'NONE',  ( 16.90442126109993737, -293.7899599567780342, -221.0854665434989670 ) ) ;
#28222 = CARTESIAN_POINT ( 'NONE',  ( -53.17075368909969058, -296.5660545582534837, -345.2667576224077948 ) ) ;
#28223 = CARTESIAN_POINT ( 'NONE',  ( -109.1425161710217679, -296.2107265850891622, -283.6077357180204785 ) ) ;
#28224 = CARTESIAN_POINT ( 'NONE',  ( -28.92403570801938528, -290.9455890375159584, -344.8872447663294452 ) ) ;
#28225 = CARTESIAN_POINT ( 'NONE',  ( -113.4877514638859992, -284.8662507383784259, -258.5736007833649523 ) ) ;
#28226 = CARTESIAN_POINT ( 'NONE',  ( 11.01583020941407121, -272.8523817500299060, -211.9675058205340008 ) ) ;
#28227 = CARTESIAN_POINT ( 'NONE',  ( 27.13891865678215254, -286.8325718297650724, -228.2748992687869247 ) ) ;
#28228 = CARTESIAN_POINT ( 'NONE',  ( -60.26213215570052739, -281.7335712239016061, -199.2678796310722475 ) ) ;
#28229 = CARTESIAN_POINT ( 'NONE',  ( -96.75872625015618667, -284.2079516786839690, -227.5258824215704578 ) ) ;
#28230 = CARTESIAN_POINT ( 'NONE',  ( -73.48640904561523257, -287.5314850700121383, -336.0915394860306264 ) ) ;
#28231 = CARTESIAN_POINT ( 'NONE',  ( 126.6218730542261568, 145.9178657400643431, -262.1768218896158373 ) ) ;
#28232 = CARTESIAN_POINT ( 'NONE',  ( 20.39313511829428904, -286.4297090199575564, -225.5874958269120043 ) ) ;
#28233 = CARTESIAN_POINT ( 'NONE',  ( -27.39068880348714785, -283.8700397890278282, -346.5313159530292069 ) ) ;
#28234 = CARTESIAN_POINT ( 'NONE',  ( -104.3985991894187464, -290.0968076811613514, -232.9954586059634494 ) ) ;
#28235 = AXIS2_PLACEMENT_3D ( 'NONE', #73765, #88877, #72831 ) ;
#28236 = CARTESIAN_POINT ( 'NONE',  ( -97.95254533299885225, -280.7745758153931206, -224.1579778351505468 ) ) ;
#28237 = CARTESIAN_POINT ( 'NONE',  ( -73.54714586137188803, -280.8972150909823426, -202.9484576090193855 ) ) ;
#28238 = CARTESIAN_POINT ( 'NONE',  ( 18.83746333747442137, -280.7241845885035900, -223.7273239982240511 ) ) ;
#28239 = CARTESIAN_POINT ( 'NONE',  ( 22.25570254758597244, -276.9287847461008596, -224.8081276612231534 ) ) ;
#28240 = CARTESIAN_POINT ( 'NONE',  ( -65.60349775875658906, -295.4116592975155413, -342.0012486326589851 ) ) ;
#28241 = CARTESIAN_POINT ( 'NONE',  ( 17.19584324582809032, -286.2898704726347887, -321.4024250702861423 ) ) ;
#28242 = CARTESIAN_POINT ( 'NONE',  ( 10.59948876026856013, -294.3015937381687195, -211.0641761292658316 ) ) ;
#28243 = CARTESIAN_POINT ( 'NONE',  ( -97.12689406063604736, -296.0624191245326529, -227.9352218751724308 ) ) ;
#28244 = EDGE_LOOP ( 'NONE', ( #63106, #24772, #62377, #26872, #39608 ) ) ;
#28245 = CARTESIAN_POINT ( 'NONE',  ( -33.39591625071374636, -284.9222791111476454, -344.7092933470706271 ) ) ;
#28246 = CARTESIAN_POINT ( 'NONE',  ( -109.3844692818184114, -296.0617587240714670, -282.2744256454533343 ) ) ;
#28247 = CARTESIAN_POINT ( 'NONE',  ( 6.308962904953159700, -293.7095395394031812, -207.3046978034235792 ) ) ;
#28248 = CARTESIAN_POINT ( 'NONE',  ( 7.863494910495058221, -283.0675139387952299, -327.8747319127886612 ) ) ;
#28249 = CARTESIAN_POINT ( 'NONE',  ( -58.04659286304920585, -272.8498895435625400, -196.3861271410816585 ) ) ;
#28250 = CARTESIAN_POINT ( 'NONE',  ( -75.60575182150422791, -290.2002513685679901, -337.0632553892853593 ) ) ;
#28251 = CARTESIAN_POINT ( 'NONE',  ( -13.82813477853880180, -280.8897849415487258, -342.3848482620905997 ) ) ;
#28252 = CARTESIAN_POINT ( 'NONE',  ( -111.9004935473823252, -290.6451154730147550, -289.5640506319537053 ) ) ;
#28253 = CARTESIAN_POINT ( 'NONE',  ( -26.46755010455341051, -289.2433848408505810, -342.6191097243445256 ) ) ;
#28254 = CARTESIAN_POINT ( 'NONE',  ( 175.2296996224750103, 20.99999999999998934, -24.00000000000000355 ) ) ;
#28255 = CARTESIAN_POINT ( 'NONE',  ( 153.5370352062773520, 129.8649369643340492, -11.69957875851211249 ) ) ;
#28256 = CARTESIAN_POINT ( 'NONE',  ( 193.2925842856977283, 275.7319325034035273, -124.0216442356983322 ) ) ;
#28257 = CARTESIAN_POINT ( 'NONE',  ( -106.6379572354042296, -270.4809262143061233, -236.9535640164627353 ) ) ;
#28258 = CARTESIAN_POINT ( 'NONE',  ( -109.6532155393864798, -277.6029532917806364, -281.4807612333127622 ) ) ;
#28259 = ORIENTED_EDGE ( 'NONE', *, *, #2228, .T. ) ;
#28260 = CARTESIAN_POINT ( 'NONE',  ( -68.64285039021375212, -278.5510994786062611, -204.0703639745659927 ) ) ;
#28261 = CARTESIAN_POINT ( 'NONE',  ( 38.70738402024316116, -275.0685898997495542, -258.3479583630651746 ) ) ;
#28262 = CARTESIAN_POINT ( 'NONE',  ( 190.8835322504810676, 268.3746148070026152, -138.2713062114818285 ) ) ;
#28263 = CARTESIAN_POINT ( 'NONE',  ( -45.19462286533578776, -278.5294077734797042, -194.3023633270605615 ) ) ;
#28264 = CARTESIAN_POINT ( 'NONE',  ( -104.5033528016349464, -282.1396040418259190, -303.0553471374125252 ) ) ;
#28265 = CARTESIAN_POINT ( 'NONE',  ( -111.8988365848795041, -298.4990520223184376, -255.6241553476149591 ) ) ;
#28266 = CARTESIAN_POINT ( 'NONE',  ( 34.00854564896192045, -293.8365349737172210, -254.5828940317004196 ) ) ;
#28267 = ORIENTED_EDGE ( 'NONE', *, *, #940, .T. ) ;
#28268 = CARTESIAN_POINT ( 'NONE',  ( -110.8606930591889324, -289.2622454714943956, -268.4322173840665187 ) ) ;
#28269 = CARTESIAN_POINT ( 'NONE',  ( -27.01842774447975870, -274.8313914881420601, -194.1057720772648736 ) ) ;
#28270 = CARTESIAN_POINT ( 'NONE',  ( -47.27484840216956741, -298.0892411032280620, -197.9888690110764458 ) ) ;
#28271 = ORIENTED_EDGE ( 'NONE', *, *, #26870, .T. ) ;
#28272 = CARTESIAN_POINT ( 'NONE',  ( 222.4201966301864672, -44.14345022962302068, -22.50000000000000000 ) ) ;
#28273 = EDGE_CURVE ( 'NONE', #36049, #77270, #1953, .T. ) ;
#28274 = CARTESIAN_POINT ( 'NONE',  ( 154.2759627658477939, 20.32662787347680222, 12.20915505293938530 ) ) ;
#28275 = CARTESIAN_POINT ( 'NONE',  ( 2.862065401724003699, -281.6850157889714978, -208.9986366600172403 ) ) ;
#28276 = CARTESIAN_POINT ( 'NONE',  ( 10.17168953740782378, -282.4568323180754419, -210.9940145562682687 ) ) ;
#28277 = CARTESIAN_POINT ( 'NONE',  ( -106.7514822109890105, -283.9220947784536975, -246.8423828427566775 ) ) ;
#28278 = CARTESIAN_POINT ( 'NONE',  ( -1.388249863805268713, -282.3947712243137858, -205.4133320649779364 ) ) ;
#28279 = CARTESIAN_POINT ( 'NONE',  ( -3.566783299242565430, -275.0777469910586888, -335.8589251771521731 ) ) ;
#28280 = DIRECTION ( 'NONE',  ( -1.000000000000000000, -0.000000000000000000, -0.000000000000000000 ) ) ;
#28281 = CARTESIAN_POINT ( 'NONE',  ( -37.11715091922809506, -277.8522009983414023, -347.2123456663356933 ) ) ;
#28282 = DIRECTION ( 'NONE',  ( -0.000000000000000000, -1.000000000000000000, -0.000000000000000000 ) ) ;
#28283 = ORIENTED_EDGE ( 'NONE', *, *, #20809, .F. ) ;
#28284 = CARTESIAN_POINT ( 'NONE',  ( 208.0212563688061209, 27.56882951438707607, 12.00000000000000000 ) ) ;
#28285 = CARTESIAN_POINT ( 'NONE',  ( -107.7567829909006178, -286.1832625031181578, -297.3414952590535449 ) ) ;
#28286 = CARTESIAN_POINT ( 'NONE',  ( 24.99079450515892020, -292.2213257825347910, -231.9600675560892000 ) ) ;
#28287 = EDGE_CURVE ( 'NONE', #40097, #42461, #29008, .T. ) ;
#28288 = CARTESIAN_POINT ( 'NONE',  ( -14.98981534668951454, -288.1187496797799668, -343.9946843718208243 ) ) ;
#28289 = CARTESIAN_POINT ( 'NONE',  ( -35.89144408075565451, -284.3104467680829543, -196.3619911400743945 ) ) ;
#28291 = CARTESIAN_POINT ( 'NONE',  ( -12.97512089154715653, -286.9709733649725649, -340.2484832851479837 ) ) ;
#28290 = CARTESIAN_POINT ( 'NONE',  ( -62.74941192218881980, -284.2897048478316151, -201.2428744651817851 ) ) ;
#28292 = CARTESIAN_POINT ( 'NONE',  ( 14.21446335635532954, -283.5134547372127258, -322.6734096486179055 ) ) ;
#28293 = CARTESIAN_POINT ( 'NONE',  ( -8.437187426262960699, -272.4302129329582272, -201.0995521608556089 ) ) ;
#28294 = CARTESIAN_POINT ( 'NONE',  ( -84.99657131749313521, -283.8068220410114009, -210.9014369767490393 ) ) ;
#28295 = CARTESIAN_POINT ( 'NONE',  ( -41.80051706656752941, -297.1083613085517641, -345.2794979898001770 ) ) ;
#28296 = CARTESIAN_POINT ( 'NONE',  ( -111.9957770044708383, -282.6642618403684537, -261.5977150279383636 ) ) ;
#28297 = CARTESIAN_POINT ( 'NONE',  ( -99.67427751751634446, -280.0229711684557969, -231.8188253953773597 ) ) ;
#28298 = CARTESIAN_POINT ( 'NONE',  ( 4.146041451738739170, -288.6095584392433011, -207.6190294715171660 ) ) ;
#28299 = CARTESIAN_POINT ( 'NONE',  ( 196.2373416849518151, 25.97420206995995073, 13.14673451885373368 ) ) ;
#28300 = CARTESIAN_POINT ( 'NONE',  ( 199.4392256788250677, 65.82574266882504332, 7.741079165001067963 ) ) ;
#28301 = CARTESIAN_POINT ( 'NONE',  ( 37.79147270589700724, -295.3640016885484556, -261.8631178182608323 ) ) ;
#28302 = CARTESIAN_POINT ( 'NONE',  ( -111.9530736642375501, -276.6562656018784310, -262.2398140564039295 ) ) ;
#28303 = CARTESIAN_POINT ( 'NONE',  ( -114.2070411641225576, -289.7745416608204323, -268.3487175639312454 ) ) ;
#28304 = CARTESIAN_POINT ( 'NONE',  ( -5.211432686409379400, -293.0219433526013972, -336.8136683314594393 ) ) ;
#28305 = CARTESIAN_POINT ( 'NONE',  ( 2.988507873670241732, -279.2905561233907861, -208.8613125284154250 ) ) ;
#28307 = EDGE_CURVE ( 'NONE', #15166, #10282, #43215, .T. ) ;
#28306 = CARTESIAN_POINT ( 'NONE',  ( -111.7807899796114839, -270.6682393416608079, -267.5591356020806870 ) ) ;
#28308 = CARTESIAN_POINT ( 'NONE',  ( -92.05139610758976687, -292.5650613949779881, -221.2699691272126472 ) ) ;
#28309 = CARTESIAN_POINT ( 'NONE',  ( -37.37352853689063892, -276.5519495502701943, -195.3611179825600175 ) ) ;
#28310 = CARTESIAN_POINT ( 'NONE',  ( -22.25374103378196011, -293.3421642802720726, -345.1612599696929919 ) ) ;
#28311 = CARTESIAN_POINT ( 'NONE',  ( 24.18762060913717704, -289.7118520561572836, -311.1344624296644383 ) ) ;
#28312 = CARTESIAN_POINT ( 'NONE',  ( -22.37120057738430390, -290.4810262123950224, -195.8101340056990978 ) ) ;
#28313 = CARTESIAN_POINT ( 'NONE',  ( -48.12957299507327491, -290.6172278044049335, -343.2067586893828093 ) ) ;
#28314 = DIRECTION ( 'NONE',  ( -1.224646799147353207E-16, 1.000000000000000000, 0.000000000000000000 ) ) ;
#28315 = CARTESIAN_POINT ( 'NONE',  ( -10.65569201325464910, -289.4979349682825500, -338.5363695234173633 ) ) ;
#28316 = DIRECTION ( 'NONE',  ( -1.000000000000000000, 0.000000000000000000, 0.000000000000000000 ) ) ;
#28317 = CARTESIAN_POINT ( 'NONE',  ( -98.70181860357061510, -291.1436925374194402, -316.2406777845557144 ) ) ;
#28319 = CARTESIAN_POINT ( 'NONE',  ( -109.7895141777525367, -290.4339308599354581, -279.3229391939135553 ) ) ;
#28318 = CARTESIAN_POINT ( 'NONE',  ( 23.28379039339642986, -278.9645514771179364, -225.6067136813653065 ) ) ;
#28320 = CARTESIAN_POINT ( 'NONE',  ( -41.01163423075385595, -280.3404657819189083, -193.4566010151165472 ) ) ;
#28321 = CARTESIAN_POINT ( 'NONE',  ( 38.84973329861187352, -281.3562580944006299, -281.3433656533117642 ) ) ;
#28322 = CARTESIAN_POINT ( 'NONE',  ( 34.21430011340099497, -285.8438185006478989, -293.0001849796011015 ) ) ;
#28323 = CARTESIAN_POINT ( 'NONE',  ( 202.6689663790774887, 287.6799160531548409, -4.951217617476999955 ) ) ;
#28324 = CARTESIAN_POINT ( 'NONE',  ( 29.24876831152463197, -280.1303457736433984, -303.2889034600283935 ) ) ;
#28325 = CARTESIAN_POINT ( 'NONE',  ( -63.81672455304082803, -283.7068214046984167, -200.1755758578940174 ) ) ;
#28326 = DIRECTION ( 'NONE',  ( 0.000000000000000000, 0.000000000000000000, -1.000000000000000000 ) ) ;
#28327 = CARTESIAN_POINT ( 'NONE',  ( -113.3898918052547202, -276.9451060890970098, -277.2490561028980096 ) ) ;
#28328 = CARTESIAN_POINT ( 'NONE',  ( -7.450868010730220092, -285.3551958583295800, -199.6786931537127145 ) ) ;
#28329 = CARTESIAN_POINT ( 'NONE',  ( -14.02363297095190653, -275.1653942578785177, -201.0151053300785406 ) ) ;
#28330 = LINE ( 'NONE', #52297, #484 ) ;
#28331 = CARTESIAN_POINT ( 'NONE',  ( -41.65979929593486020, -293.5971313076430533, -196.6371591474400589 ) ) ;
#28332 = CARTESIAN_POINT ( 'NONE',  ( -35.55589187825142972, -275.4993826257528440, -193.9581857035290113 ) ) ;
#28333 = CARTESIAN_POINT ( 'NONE',  ( -76.37070613831363630, -277.2561962624366174, -332.1362596562551630 ) ) ;
#28334 = CARTESIAN_POINT ( 'NONE',  ( -110.4315724295534693, -291.0256432409331637, -245.9688349423528848 ) ) ;
#28335 = CARTESIAN_POINT ( 'NONE',  ( 31.86402919032397563, -279.2378518939059973, -240.0315742205260676 ) ) ;
#28336 = CARTESIAN_POINT ( 'NONE',  ( -7.188246166747680910, -292.2702027453557321, -199.4964663984306128 ) ) ;
#28337 = CARTESIAN_POINT ( 'NONE',  ( -60.32146125780350587, -290.8056370598891363, -200.7713084256891705 ) ) ;
#28338 = CARTESIAN_POINT ( 'NONE',  ( -22.51840680678187567, -292.8622030125993092, -343.8816635520170735 ) ) ;
#28339 = VERTEX_POINT ( 'NONE', #72116 ) ;
#28340 = CARTESIAN_POINT ( 'NONE',  ( 152.6996702291354211, 19.85642976176308139, 8.932053473883454942 ) ) ;
#28341 = CARTESIAN_POINT ( 'NONE',  ( 22.64203867691799132, -292.4786581677000186, -228.6264896721686171 ) ) ;
#28342 = DIRECTION ( 'NONE',  ( -0.000000000000000000, -1.000000000000000000, -0.000000000000000000 ) ) ;
#28343 = CARTESIAN_POINT ( 'NONE',  ( -6.998514795304330072, -280.1237833571632336, -333.4427485647536855 ) ) ;
#28344 = CARTESIAN_POINT ( 'NONE',  ( -97.23142217410500621, -294.9653202116670059, -318.4031849749455318 ) ) ;
#28345 = CARTESIAN_POINT ( 'NONE',  ( -106.2423027022131095, -286.2967567186024098, -237.1044609596501687 ) ) ;
#28346 = CARTESIAN_POINT ( 'NONE',  ( 29.96259376634963800, -287.0045857113311172, -241.9612783996791165 ) ) ;
#28347 = CARTESIAN_POINT ( 'NONE',  ( 10.12527082571453718, -277.9037474629217854, -326.7312733756273815 ) ) ;
#28348 = CARTESIAN_POINT ( 'NONE',  ( 36.93462677629541702, -291.4702222292804663, -262.4521460158393893 ) ) ;
#28349 = CARTESIAN_POINT ( 'NONE',  ( -63.91212782299929529, -297.1634670437745740, -339.4949773434000804 ) ) ;
#28350 = CARTESIAN_POINT ( 'NONE',  ( -29.68719177125014852, -275.7481403152637540, -343.4091425660722621 ) ) ;
#28351 = ORIENTED_EDGE ( 'NONE', *, *, #60229, .F. ) ;
#28352 = CARTESIAN_POINT ( 'NONE',  ( 194.2870706637141325, 39.36132622696000283, 14.58823529411764675 ) ) ;
#28353 = CARTESIAN_POINT ( 'NONE',  ( -68.22159410805548418, -295.1134861140318435, -340.8747793495459177 ) ) ;
#28354 = CARTESIAN_POINT ( 'NONE',  ( -31.73904115706336526, -290.9011888229114220, -344.6416052184358136 ) ) ;
#28355 = CARTESIAN_POINT ( 'NONE',  ( -77.68490200995596240, -295.5107798038987426, -207.0751259330633332 ) ) ;
#28356 = CARTESIAN_POINT ( 'NONE',  ( -26.45152270995227894, -289.5614656518309857, -342.6984529841714675 ) ) ;
#28357 = EDGE_LOOP ( 'NONE', ( #14821, #80378, #88183, #27209, #86593, #61328 ) ) ;
#28358 = CARTESIAN_POINT ( 'NONE',  ( 19.96105889002106437, -279.9160973750380208, -219.2608830957678947 ) ) ;
#28359 = CARTESIAN_POINT ( 'NONE',  ( 11.14048502495207593, -295.0526103053552447, -330.1188594882695497 ) ) ;
#28360 = CARTESIAN_POINT ( 'NONE',  ( -67.58297230049872439, -287.5842880753826307, -339.8288870556209531 ) ) ;
#28361 = CARTESIAN_POINT ( 'NONE',  ( -92.67885520298236202, -296.1521376562493515, -323.8732059600917523 ) ) ;
#28362 = CARTESIAN_POINT ( 'NONE',  ( 19.71294465489122771, -294.5291887324432878, -315.9535769871431512 ) ) ;
#28363 = CARTESIAN_POINT ( 'NONE',  ( 197.1861737955271963, 69.99861189218830759, -10.13991136371132207 ) ) ;
#28364 = DIRECTION ( 'NONE',  ( 0.000000000000000000, 0.000000000000000000, -1.000000000000000000 ) ) ;
#28365 = CARTESIAN_POINT ( 'NONE',  ( 165.2494399300530290, -11.64849832608277325, 9.974999999999996092 ) ) ;
#28366 = CARTESIAN_POINT ( 'NONE',  ( 38.66220832902902060, -288.9794338081946421, -263.0046742499005177 ) ) ;
#28367 = CARTESIAN_POINT ( 'NONE',  ( -55.63300648810263738, -282.3376638359844151, -190.3683826091709363 ) ) ;
#28368 = CARTESIAN_POINT ( 'NONE',  ( -69.91164440902817034, -278.9830115240158079, -200.6867775767822479 ) ) ;
#28369 = CARTESIAN_POINT ( 'NONE',  ( -51.33638705727141627, -285.2315219397586361, -343.9270957213098541 ) ) ;
#28370 = CARTESIAN_POINT ( 'NONE',  ( 29.62398548833278156, -285.6453926094040412, -233.4517842346842258 ) ) ;
#28371 = B_SPLINE_CURVE_WITH_KNOTS ( 'NONE', 3,
 ( #9671, #17258, #86518, #28788, #9191, #44722 ),
 .UNSPECIFIED., .F., .F.,
 ( 4, 2, 4 ),
 ( 0.0009696774721519553974, 0.002350549526938858821, 0.003731421581725762136 ),
 .UNSPECIFIED. ) ;
#28372 = CARTESIAN_POINT ( 'NONE',  ( 37.06829794255180843, -285.6771417894561296, -273.8512573091762192 ) ) ;
#28373 = CARTESIAN_POINT ( 'NONE',  ( 36.97547293525119727, -277.5999108600984187, -285.1009711396022794 ) ) ;
#28374 = ORIENTED_EDGE ( 'NONE', *, *, #51069, .F. ) ;
#28376 = CARTESIAN_POINT ( 'NONE',  ( -110.2597366796839395, -277.9689982681035190, -265.1791672499649621 ) ) ;
#28375 = CARTESIAN_POINT ( 'NONE',  ( -107.2271173388270284, -278.8314523100888778, -249.2654202865838613 ) ) ;
#28377 = CARTESIAN_POINT ( 'NONE',  ( -35.54486669291351575, -275.1538376283556318, -193.6782033881368363 ) ) ;
#28378 = CARTESIAN_POINT ( 'NONE',  ( -77.27236899099928280, -278.3246323492271586, -204.9273191779148533 ) ) ;
#28379 = CARTESIAN_POINT ( 'NONE',  ( -109.8935430929009840, -264.1146777768358334, -305.7921915240701196 ) ) ;
#28380 = CARTESIAN_POINT ( 'NONE',  ( -112.8391045486285975, -273.6712229691746643, -256.1860008254682270 ) ) ;
#28381 = CARTESIAN_POINT ( 'NONE',  ( -3.751190591230367133, -299.8901968535543574, -193.9423814121325620 ) ) ;
#28382 = EDGE_CURVE ( 'NONE', #4576, #6353, #79670, .T. ) ;
#28383 = CARTESIAN_POINT ( 'NONE',  ( -106.6662871844225293, -293.4805209788415823, -237.0123917617630980 ) ) ;
#28384 = VERTEX_POINT ( 'NONE', #49387 ) ;
#28385 = DIRECTION ( 'NONE',  ( 0.000000000000000000, 0.000000000000000000, 1.000000000000000000 ) ) ;
#28386 = CARTESIAN_POINT ( 'NONE',  ( -83.85456148404830401, -286.4759049093451608, -213.6314077734191130 ) ) ;
#28387 = CARTESIAN_POINT ( 'NONE',  ( -109.0287915748000245, -286.6343918355893834, -245.1632027404195640 ) ) ;
#28388 = CARTESIAN_POINT ( 'NONE',  ( 14.14930715884026569, -287.6537511809348757, -322.2510865376845572 ) ) ;
#28389 = CARTESIAN_POINT ( 'NONE',  ( -103.9840160314192730, -284.5612455575871422, -231.8061457548824080 ) ) ;
#28390 = CARTESIAN_POINT ( 'NONE',  ( -66.36576111139123668, -278.0655631838487238, -202.4942231890591131 ) ) ;
#28391 = CARTESIAN_POINT ( 'NONE',  ( -11.61577298641283562, -288.2512052509643468, -200.7260538792021123 ) ) ;
#28392 = CARTESIAN_POINT ( 'NONE',  ( 30.97005544243717523, -280.3987505263974072, -298.0054989999449049 ) ) ;
#28393 = CARTESIAN_POINT ( 'NONE',  ( -103.5681841008370583, -279.4377183200045351, -302.3425322013466143 ) ) ;
#28394 = CARTESIAN_POINT ( 'NONE',  ( 34.43278222750208784, -275.8645433489803622, -256.7078354323108442 ) ) ;
#28395 = CARTESIAN_POINT ( 'NONE',  ( -23.39935020333249227, -287.6727716158931116, -345.7383852058756020 ) ) ;
#28396 = CARTESIAN_POINT ( 'NONE',  ( 25.80347286089903491, -282.9348127611646078, -314.1660620642208528 ) ) ;
#28397 = CARTESIAN_POINT ( 'NONE',  ( -81.52108806444685740, -284.1276142721295059, -333.4156786522270863 ) ) ;
#28398 = CARTESIAN_POINT ( 'NONE',  ( -8.001393944992623020, -280.6142058573529994, -203.5032505283305682 ) ) ;
#28399 = EDGE_LOOP ( 'NONE', ( #66064, #54902, #53377, #41976 ) ) ;
#28400 = ORIENTED_EDGE ( 'NONE', *, *, #64378, .T. ) ;
#28401 = CARTESIAN_POINT ( 'NONE',  ( 156.5854952678944301, 214.6009552038394759, 16.65543863426000470 ) ) ;
#28402 = CARTESIAN_POINT ( 'NONE',  ( -2.349792472082426809, -290.4545249669257032, -337.5613551967477974 ) ) ;
#28403 = CARTESIAN_POINT ( 'NONE',  ( -100.2844703387150531, -288.6589451961174859, -313.8525648565666870 ) ) ;
#28404 = CARTESIAN_POINT ( 'NONE',  ( -65.89386147549961947, -272.7279132680730527, -202.9209034889935594 ) ) ;
#28405 = EDGE_CURVE ( 'NONE', #66586, #13010, #78279, .T. ) ;
#28406 = CARTESIAN_POINT ( 'NONE',  ( 28.01490804648733146, -293.4324977709014775, -310.9806000076931127 ) ) ;
#28407 = CARTESIAN_POINT ( 'NONE',  ( -56.26210232422564417, -287.7800955951983610, -341.6372508704704956 ) ) ;
#28408 = CARTESIAN_POINT ( 'NONE',  ( 35.48422810754055945, -291.6192854011053441, -257.0860523830502302 ) ) ;
#28409 = CARTESIAN_POINT ( 'NONE',  ( 23.85670293687120846, -288.1969690799986665, -229.7489374369895074 ) ) ;
#28410 = CARTESIAN_POINT ( 'NONE',  ( -106.6662871844225293, -287.4805209788416391, -237.0123917617630980 ) ) ;
#28411 = CARTESIAN_POINT ( 'NONE',  ( -15.50945203929048866, -290.7698964510578321, -342.1674554648361095 ) ) ;
#28412 = CARTESIAN_POINT ( 'NONE',  ( -40.52857529660360569, -290.0120326590459285, -195.2491665500594706 ) ) ;
#28413 = CARTESIAN_POINT ( 'NONE',  ( -109.7767041371149332, -292.8028757421384398, -250.8657049353424497 ) ) ;
#28414 = CARTESIAN_POINT ( 'NONE',  ( -96.10339076390474133, -284.8822623916798875, -314.0700662918847001 ) ) ;
#28415 = CARTESIAN_POINT ( 'NONE',  ( -9.221295223462485424, -294.4191020264000258, -200.6526446415019791 ) ) ;
#28416 = DIRECTION ( 'NONE',  ( 0.000000000000000000, -1.000000000000000000, 0.000000000000000000 ) ) ;
#28417 = DIRECTION ( 'NONE',  ( 0.000000000000000000, 0.000000000000000000, 1.000000000000000000 ) ) ;
#28418 = CARTESIAN_POINT ( 'NONE',  ( -52.24552229563639827, -275.8422797947567915, -196.4411800919441760 ) ) ;
#28419 = CARTESIAN_POINT ( 'NONE',  ( 17.71965796332989740, -281.4351889464814462, -318.5363042554145636 ) ) ;
#28420 = CARTESIAN_POINT ( 'NONE',  ( -86.18299073586358361, -281.7294940876061560, -327.2779782051489406 ) ) ;
#28421 = CARTESIAN_POINT ( 'NONE',  ( -70.74693375525615124, -294.6786811575623801, -339.5727745412522154 ) ) ;
#28422 = CARTESIAN_POINT ( 'NONE',  ( -57.11101232590282706, -272.0336020947864313, -198.9834266358783452 ) ) ;
#28423 = CARTESIAN_POINT ( 'NONE',  ( -69.90294619096133033, -275.5641426381071710, -337.3160951345850549 ) ) ;
#28424 = CARTESIAN_POINT ( 'NONE',  ( -108.0729060057444428, -297.6052626141399742, -290.3195746836731814 ) ) ;
#28425 = CARTESIAN_POINT ( 'NONE',  ( -53.25928572453645415, -296.6854281607849089, -342.2606168857566331 ) ) ;
#28426 = CARTESIAN_POINT ( 'NONE',  ( 73.43068321062709458, -134.2391364535880598, -4.999999999999990230 ) ) ;
#28427 = CARTESIAN_POINT ( 'NONE',  ( -10.42109369833701038, -295.4944946105301824, -338.3896610843711983 ) ) ;
#28429 = CARTESIAN_POINT ( 'NONE',  ( -75.21064462323710131, -297.5325194028824285, -207.8930324880744251 ) ) ;
#28428 = CARTESIAN_POINT ( 'NONE',  ( -2.950580946930152937, -284.5243794501732850, -203.2970123157070361 ) ) ;
#28430 = CARTESIAN_POINT ( 'NONE',  ( -73.61301432528566124, -285.5847271407538983, -202.3801102728685350 ) ) ;
#28431 = CARTESIAN_POINT ( 'NONE',  ( 39.06903997543155072, -287.3410128355357074, -280.1247140277017706 ) ) ;
#28432 = CARTESIAN_POINT ( 'NONE',  ( -39.04483975007040186, -297.0533146916417877, -345.6970730218347398 ) ) ;
#28433 = CARTESIAN_POINT ( 'NONE',  ( -9.010354017486729816, -290.4232240499913473, -201.0429720676251009 ) ) ;
#28434 = CARTESIAN_POINT ( 'NONE',  ( -74.92002003295255008, -278.7619707004824932, -203.3385196015004794 ) ) ;
#28435 = CARTESIAN_POINT ( 'NONE',  ( 10.64812456238590599, -284.1952119285918457, -210.2361428286349394 ) ) ;
#28436 = CARTESIAN_POINT ( 'NONE',  ( 153.8801639287781313, 129.5385997557426947, 11.85807839311486411 ) ) ;
#28437 = CARTESIAN_POINT ( 'NONE',  ( -19.70566616733899323, -285.0789360147833804, -199.1143579876925003 ) ) ;
#28438 = CARTESIAN_POINT ( 'NONE',  ( 199.1087447750284980, 64.61450673763175701, -10.46317447812566215 ) ) ;
#28439 = CARTESIAN_POINT ( 'NONE',  ( 9.201713644166414241, -286.4127103764753315, -329.1719271935503457 ) ) ;
#28440 = CARTESIAN_POINT ( 'NONE',  ( -75.64307371856145323, -299.1323897829857970, -207.2190165580626910 ) ) ;
#28441 = CARTESIAN_POINT ( 'NONE',  ( 10.44029577962546185, -282.1220172704596507, -210.6654071994988726 ) ) ;
#28443 = CARTESIAN_POINT ( 'NONE',  ( 33.45558131864618190, -281.3166696193655412, -252.5130019504298104 ) ) ;
#28442 = CARTESIAN_POINT ( 'NONE',  ( -109.6445023313047216, -294.2996289942353201, -291.6366537529475522 ) ) ;
#28444 = CARTESIAN_POINT ( 'NONE',  ( -92.69552985178474103, -295.9855633861066053, -323.8863787425185023 ) ) ;
#28445 = CARTESIAN_POINT ( 'NONE',  ( -55.48289355846002024, -299.3347238296130399, -198.8827869876849377 ) ) ;
#28446 = CARTESIAN_POINT ( 'NONE',  ( 21.87882984116004437, -284.9918841294445429, -223.4124239601724469 ) ) ;
#28447 = CARTESIAN_POINT ( 'NONE',  ( -31.26196546129850873, -282.1289783527839177, -195.5566186812525586 ) ) ;
#28448 = CARTESIAN_POINT ( 'NONE',  ( -84.21627007210248905, -296.4480018408657429, -214.0260687512058837 ) ) ;
#28449 = ORIENTED_EDGE ( 'NONE', *, *, #9944, .T. ) ;
#28450 = CYLINDRICAL_SURFACE ( 'NONE', #74062, 2.397123461337413719 ) ;
#28451 = CARTESIAN_POINT ( 'NONE',  ( 4.328879329303341628, -284.4675369076890661, -332.3543386368593247 ) ) ;
#28452 = CARTESIAN_POINT ( 'NONE',  ( 151.4851178187871312, 21.00000000000000000, 3.492110388858666870 ) ) ;
#28453 = CARTESIAN_POINT ( 'NONE',  ( -37.37352853689063181, -292.5523547857347353, -345.3611179825600175 ) ) ;
#28454 = CARTESIAN_POINT ( 'NONE',  ( 37.13125224652835499, -274.5120875601161856, -251.4418636189326719 ) ) ;
#28455 = CARTESIAN_POINT ( 'NONE',  ( -1.254829195941062903, -292.3784751178791907, -206.8900608952109224 ) ) ;
#28456 = CARTESIAN_POINT ( 'NONE',  ( 21.57577524728873897, -283.6882023982014402, -314.6475266157881947 ) ) ;
#28457 = CARTESIAN_POINT ( 'NONE',  ( 27.32783823085941677, -276.6705761294236368, -234.6977897020352941 ) ) ;
#28458 = CARTESIAN_POINT ( 'NONE',  ( -33.08287447289618655, -284.5995056645817840, -346.4550129270340335 ) ) ;
#28459 = CARTESIAN_POINT ( 'NONE',  ( 30.39380530294350891, -279.9699497601903317, -242.0939672980213970 ) ) ;
#28460 = CARTESIAN_POINT ( 'NONE',  ( -112.3932127978049209, -280.5483375756771807, -270.6710630290847917 ) ) ;
#28461 = CARTESIAN_POINT ( 'NONE',  ( -48.96998934205065979, -297.9080622941874594, -194.1905487919816835 ) ) ;
#28462 = CARTESIAN_POINT ( 'NONE',  ( 32.55395254745287303, -274.9707405430401082, -237.9293751423893752 ) ) ;
#28463 = CARTESIAN_POINT ( 'NONE',  ( 17.78850000220721483, -294.7687040044921787, -220.2657980348386104 ) ) ;
#28464 = PLANE ( 'NONE',  #35453 ) ;
#28465 = EDGE_CURVE ( 'NONE', #71834, #82501, #31333, .T. ) ;
#28466 = DIRECTION ( 'NONE',  ( 0.000000000000000000, 0.000000000000000000, 1.000000000000000000 ) ) ;
#28467 = CARTESIAN_POINT ( 'NONE',  ( -25.13061993587638909, -293.0377698050264144, -345.1886075569556169 ) ) ;
#28468 = TOROIDAL_SURFACE ( 'NONE', #26904, 25.50000000000000355, 0.5000000000000000000 ) ;
#28469 = CARTESIAN_POINT ( 'NONE',  ( -90.23683606011185532, -272.7861916843015706, -219.9434803805021375 ) ) ;
#28470 = CARTESIAN_POINT ( 'NONE',  ( -8.630782098019755821, -296.2034329184634771, -341.1163975170875347 ) ) ;
#28471 = CARTESIAN_POINT ( 'NONE',  ( 21.89240877794877704, -294.1015500400542351, -221.7881927840422236 ) ) ;
#28472 = CARTESIAN_POINT ( 'NONE',  ( -31.70854943656532043, -290.9811823333152461, -345.0340290010827289 ) ) ;
#28473 = CARTESIAN_POINT ( 'NONE',  ( -110.5637862384032530, -276.3532372914447137, -285.8063287626636111 ) ) ;
#28474 = CARTESIAN_POINT ( 'NONE',  ( -69.85879053232243052, -279.4038289387650593, -337.3375516678631811 ) ) ;
#28475 = CARTESIAN_POINT ( 'NONE',  ( 27.02579904642238517, -292.1350876887759682, -307.7528182094750377 ) ) ;
#28476 = CARTESIAN_POINT ( 'NONE',  ( 24.11939543188977453, -284.0097929729437283, -314.6870908671187976 ) ) ;
#28477 = CARTESIAN_POINT ( 'NONE',  ( -60.06143061898620772, -284.6709599091000769, -200.6614772407775149 ) ) ;
#28478 = ORIENTED_EDGE ( 'NONE', *, *, #62997, .T. ) ;
#28479 = CARTESIAN_POINT ( 'NONE',  ( -69.02217679628078884, -283.1473695424714947, -336.1657673458254294 ) ) ;
#28480 = CARTESIAN_POINT ( 'NONE',  ( 19.88881048564466170, -281.9366943835040615, -219.2908015978099741 ) ) ;
#28481 = CARTESIAN_POINT ( 'NONE',  ( -75.89354559437660441, -284.3446289529159117, -204.1051473292179423 ) ) ;
#28482 = CARTESIAN_POINT ( 'NONE',  ( -99.24525265291504184, -280.0983648947290021, -224.9432197278113676 ) ) ;
#28483 =( NAMED_UNIT ( * ) PLANE_ANGLE_UNIT ( ) SI_UNIT ( $, .RADIAN. ) );
#28484 = CARTESIAN_POINT ( 'NONE',  ( -42.73764658997463783, -278.6391963444464182, -346.4767636455488287 ) ) ;
#28485 = CARTESIAN_POINT ( 'NONE',  ( -107.3417001280813565, -270.0523547857346784, -270.3292895737509980 ) ) ;
#28486 = EDGE_LOOP ( 'NONE', ( #2363, #28727, #22403, #71357 ) ) ;
#28487 = ORIENTED_EDGE ( 'NONE', *, *, #9225, .T. ) ;
#28488 = CARTESIAN_POINT ( 'NONE',  ( 98.92740146068138074, -301.7582495827366529, -195.3146565631489864 ) ) ;
#28489 = CARTESIAN_POINT ( 'NONE',  ( -52.12907782588145267, -277.8821703048455447, -197.1427941626550933 ) ) ;
#28490 = CARTESIAN_POINT ( 'NONE',  ( -109.8085733308718375, -292.0192256045564250, -293.3916848779560382 ) ) ;
#28491 = CARTESIAN_POINT ( 'NONE',  ( 33.21290587866195665, -293.1536491949343599, -289.5382562690976442 ) ) ;
#28492 = CARTESIAN_POINT ( 'NONE',  ( -37.50775581640981926, -288.5617982835651105, -347.3124618552888023 ) ) ;
#28493 = DIRECTION ( 'NONE',  ( 0.000000000000000000, 0.000000000000000000, 1.000000000000000000 ) ) ;
#28495 = CARTESIAN_POINT ( 'NONE',  ( 13.70748821460256650, -285.1814993094901638, -216.9949957669825551 ) ) ;
#28494 = CARTESIAN_POINT ( 'NONE',  ( 35.80033258094827886, -292.4085891141127149, -292.6501493059306540 ) ) ;
#28496 = CARTESIAN_POINT ( 'NONE',  ( -52.64719312274739593, -293.7145564622181837, -197.6680753076331882 ) ) ;
#28497 = CARTESIAN_POINT ( 'NONE',  ( -30.44732214321059516, -284.6206489963906279, -196.9397109779411608 ) ) ;
#28498 = CARTESIAN_POINT ( 'NONE',  ( 33.43888422345286671, -283.1270411310507598, -290.1437456567363142 ) ) ;
#28499 = CARTESIAN_POINT ( 'NONE',  ( -16.70143513112662959, -293.2537280737448668, -196.4233084857097822 ) ) ;
#28500 = CARTESIAN_POINT ( 'NONE',  ( 32.79190502860596723, -281.7738542076801878, -249.8851352351114485 ) ) ;
#28501 = CARTESIAN_POINT ( 'NONE',  ( -36.29534569271209676, -293.8342745126162754, -346.9699366343728570 ) ) ;
#28502 = CARTESIAN_POINT ( 'NONE',  ( -43.15984973873052866, -289.9266858464213215, -346.9790529299918376 ) ) ;
#28503 = CARTESIAN_POINT ( 'NONE',  ( -26.14731371219676603, -289.4056175643074198, -346.4808435198353891 ) ) ;
#28504 = CARTESIAN_POINT ( 'NONE',  ( -89.66433739983241935, -285.4556235800654349, -219.3833542634595517 ) ) ;
#28505 = EDGE_LOOP ( 'NONE', ( #70059, #71493, #11478, #3377 ) ) ;
#28506 = CYLINDRICAL_SURFACE ( 'NONE', #24657, 4.999999999999990230 ) ;
#28507 = CARTESIAN_POINT ( 'NONE',  ( -41.84802413041015967, -296.9686393303921932, -346.0433434733269564 ) ) ;
#28508 = CARTESIAN_POINT ( 'NONE',  ( -50.39993521719393499, -293.9002168524291392, -345.7989399140182059 ) ) ;
#28509 = CARTESIAN_POINT ( 'NONE',  ( -110.5157259006389268, -277.5715116476278013, -273.3561805335664872 ) ) ;
#28510 = CARTESIAN_POINT ( 'NONE',  ( -60.84635035476559040, -273.2628992908906298, -197.0453243812449102 ) ) ;
#28511 = CARTESIAN_POINT ( 'NONE',  ( 12.81270761395191826, -292.8172340018795126, -324.4240326373146672 ) ) ;
#28512 = CARTESIAN_POINT ( 'NONE',  ( 18.21044641385283569, -278.0012426477495069, -319.2876373444584601 ) ) ;
#28513 = CARTESIAN_POINT ( 'NONE',  ( -111.5769001271280843, -270.6920356235430631, -270.3374848783465154 ) ) ;
#28514 = CARTESIAN_POINT ( 'NONE',  ( 18.28334148698370143, -295.4356552216946739, -318.2654117656361450 ) ) ;
#28515 = CARTESIAN_POINT ( 'NONE',  ( -84.66721260088756651, -296.8016400516380600, -326.4145592287690079 ) ) ;
#28516 = CARTESIAN_POINT ( 'NONE',  ( -43.35418436979174572, -267.5839012688533671, -434.2375725762524326 ) ) ;
#28517 = CARTESIAN_POINT ( 'NONE',  ( -87.40385372127317964, -293.7478560322562657, -326.5006183914676967 ) ) ;
#28518 = CARTESIAN_POINT ( 'NONE',  ( -60.12581276806698583, -298.4159258269825159, -196.8604699823577562 ) ) ;
#28519 = CARTESIAN_POINT ( 'NONE',  ( -56.23423490102257460, -287.8749300005506484, -341.5368630525657068 ) ) ;
#28520 = CARTESIAN_POINT ( 'NONE',  ( -96.19763085118555068, -275.1907627763315531, -223.8747751254295508 ) ) ;
#28521 = CARTESIAN_POINT ( 'NONE',  ( -109.9349923283016324, -291.6255911271211403, -260.3086581466929488 ) ) ;
#28522 = CARTESIAN_POINT ( 'NONE',  ( -34.11205789542941602, -274.5840959186526788, -193.4904713453673253 ) ) ;
#28523 = CARTESIAN_POINT ( 'NONE',  ( -108.6115791286629815, -296.6757965447201855, -286.2574016400802179 ) ) ;
#28524 = CARTESIAN_POINT ( 'NONE',  ( -102.0132352982649309, -281.0485310563680628, -231.5814530067391956 ) ) ;
#28525 = CARTESIAN_POINT ( 'NONE',  ( 37.20083460002793885, -280.0195157330298912, -253.0782653648941505 ) ) ;
#28526 = EDGE_LOOP ( 'NONE', ( #79054, #15330 ) ) ;
#28527 = ADVANCED_FACE ( 'NONE', ( #52163, #87210 ), #45985, .F. ) ;
#28528 = CARTESIAN_POINT ( 'NONE',  ( -69.15187290582098001, -282.8082658700704428, -340.3856966308424603 ) ) ;
#28529 = CARTESIAN_POINT ( 'NONE',  ( 26.85004453705635896, -274.3432348589163894, -228.0204436447908449 ) ) ;
#28530 = CARTESIAN_POINT ( 'NONE',  ( -25.49961332998155328, -278.6005328050862317, -195.0869165981462459 ) ) ;
#28531 = CARTESIAN_POINT ( 'NONE',  ( 18.77732092554002463, -278.8573599125859914, -220.3349179597435636 ) ) ;
#28532 = EDGE_CURVE ( 'NONE', #52326, #15079, #9531, .T. ) ;
#28533 = CARTESIAN_POINT ( 'NONE',  ( -95.06368389007577946, -271.7658846459888764, -224.7152253996716524 ) ) ;
#28534 = CARTESIAN_POINT ( 'NONE',  ( 11.83664892150792447, -276.7349936858275896, -213.6674257877280638 ) ) ;
#28535 = VECTOR ( 'NONE', #38336, 1000.000000000000000 ) ;
#28536 = DIRECTION ( 'NONE',  ( 0.3428573139466625785, 0.000000000000000000, -0.9393874931428880526 ) ) ;
#28537 = CARTESIAN_POINT ( 'NONE',  ( 32.93814406427365782, -291.2186798921856052, -243.0294737510616301 ) ) ;
#28538 = CARTESIAN_POINT ( 'NONE',  ( -107.2604300942438584, -290.9661963431117329, -237.9792970038828344 ) ) ;
#28539 = CARTESIAN_POINT ( 'NONE',  ( 28.93879108266040134, -278.0229503649280787, -305.9242239625236834 ) ) ;
#28540 = CARTESIAN_POINT ( 'NONE',  ( -90.64620244883043654, -271.2964016184525349, -217.6009940230856898 ) ) ;
#28541 = CARTESIAN_POINT ( 'NONE',  ( -65.80801644476309775, -284.8863002828427398, -198.9759378816672779 ) ) ;
#28542 = DIRECTION ( 'NONE',  ( 0.000000000000000000, 0.000000000000000000, 1.000000000000000000 ) ) ;
#28543 = CARTESIAN_POINT ( 'NONE',  ( -110.4605518797364567, -282.7670474610935685, -253.6123716280919211 ) ) ;
#28544 = CARTESIAN_POINT ( 'NONE',  ( 195.7510731661265595, -142.7221692137691775, -21.50000000000000000 ) ) ;
#28545 = CARTESIAN_POINT ( 'NONE',  ( 34.60876271578055707, -292.1568240332521782, -255.8607247996800709 ) ) ;
#28546 = CARTESIAN_POINT ( 'NONE',  ( 28.76876495960400248, -285.2392658908804606, -236.4797965107975983 ) ) ;
#28547 = DIRECTION ( 'NONE',  ( 1.000000000000000000, 0.000000000000000000, 0.000000000000000000 ) ) ;
#28548 = DIRECTION ( 'NONE',  ( -0.8195702660916324156, 0.000000000000000000, -0.5729786897769331144 ) ) ;
#28549 = CARTESIAN_POINT ( 'NONE',  ( 0.2222790942726419194, -292.5521961339405266, -335.3353120175667073 ) ) ;
#28550 = CARTESIAN_POINT ( 'NONE',  ( -71.44638962548887662, -281.9742861700697745, -338.6222189808248686 ) ) ;
#28551 = CARTESIAN_POINT ( 'NONE',  ( -71.32802330024252058, -281.1957769393596891, -204.8383234104281314 ) ) ;
#28552 = CARTESIAN_POINT ( 'NONE',  ( -112.7433490751408840, -285.5836919336028927, -284.1649993788072379 ) ) ;
#28553 = CARTESIAN_POINT ( 'NONE',  ( -4.080656119599637144, -278.7245511021169477, -202.0263889879495878 ) ) ;
#28554 = CARTESIAN_POINT ( 'NONE',  ( 32.31361609759608911, -287.8436563150969505, -292.3728220202745547 ) ) ;
#28555 = CARTESIAN_POINT ( 'NONE',  ( -93.16183596830248348, -279.3001362223347428, -318.3140882050001323 ) ) ;
#28556 = CARTESIAN_POINT ( 'NONE',  ( -76.43347931896123271, -278.3921269405136627, -332.2627079808701183 ) ) ;
#28557 = CARTESIAN_POINT ( 'NONE',  ( -108.4340450161021181, -286.8541073822441376, -245.3754160728247484 ) ) ;
#28558 = ORIENTED_EDGE ( 'NONE', *, *, #79777, .F. ) ;
#28559 = CARTESIAN_POINT ( 'NONE',  ( -78.20066584281454425, -297.3520132355545798, -205.0959287526150945 ) ) ;
#28560 = CARTESIAN_POINT ( 'NONE',  ( -26.20514170116859987, -290.8897307150051006, -344.2226944491937957 ) ) ;
#28561 = LINE ( 'NONE', #86762, #27688 ) ;
#28562 = CARTESIAN_POINT ( 'NONE',  ( -55.63300648810263738, -288.3376638359845288, -190.3683826091709363 ) ) ;
#28563 = ORIENTED_EDGE ( 'NONE', *, *, #18204, .F. ) ;
#28564 = CARTESIAN_POINT ( 'NONE',  ( -43.85782345427671203, -271.9699448503430972, -195.4253793298688890 ) ) ;
#28565 = CARTESIAN_POINT ( 'NONE',  ( 31.49845563045568397, -292.3765361795876174, -303.1562621562962931 ) ) ;
#28566 = CARTESIAN_POINT ( 'NONE',  ( -40.01830389208569017, -287.5380362941845078, -196.7164063859355565 ) ) ;
#28567 = PRODUCT ( 'Heavy-Duty Plastic Foot Pedal', 'Heavy-Duty Plastic Foot Pedal', '', ( #46386 ) ) ;
#28568 = CARTESIAN_POINT ( 'NONE',  ( 36.35922337219032130, -283.2169009494947431, -263.0289747195490691 ) ) ;
#28569 = CARTESIAN_POINT ( 'NONE',  ( -23.40148035319239739, -290.3026962991718278, -345.5432208753875329 ) ) ;
#28570 = CARTESIAN_POINT ( 'NONE',  ( -15.07963746813612360, -290.0850202617360765, -343.6128194289748876 ) ) ;
#28571 = CARTESIAN_POINT ( 'NONE',  ( -40.28811120983795746, -285.0893599131707674, -345.3032243909405565 ) ) ;
#28572 = CARTESIAN_POINT ( 'NONE',  ( -62.40398497116377996, -277.5359233304245095, -343.2245811122954251 ) ) ;
#28573 = ORIENTED_EDGE ( 'NONE', *, *, #84617, .F. ) ;
#28574 = CARTESIAN_POINT ( 'NONE',  ( 32.08363315579531871, -292.0206311653488456, -300.3165891057225849 ) ) ;
#28575 = CARTESIAN_POINT ( 'NONE',  ( 37.54787317587523177, -281.6100430444549829, -288.3213134733172183 ) ) ;
#28576 = CARTESIAN_POINT ( 'NONE',  ( -38.11866273645279790, -275.9027303578936312, -196.1299802249641857 ) ) ;
#28577 = CARTESIAN_POINT ( 'NONE',  ( -37.30987171927208124, -285.5519495502701943, -345.3611179825600175 ) ) ;
#28578 = CARTESIAN_POINT ( 'NONE',  ( 38.31072428392599249, -273.6949852128341831, -262.7050263693009811 ) ) ;
#28579 = LINE ( 'NONE', #86312, #68192 ) ;
#28580 = CARTESIAN_POINT ( 'NONE',  ( -35.65509781019719071, -279.5814970969258866, -197.3066360357894666 ) ) ;
#28581 = CARTESIAN_POINT ( 'NONE',  ( 37.79590505368462061, -276.9446766378411553, -285.2724897271040163 ) ) ;
#28582 = CARTESIAN_POINT ( 'NONE',  ( -41.92301125775718873, -299.4185651724802142, -196.9146306187143125 ) ) ;
#28583 = CARTESIAN_POINT ( 'NONE',  ( -83.75051943416367806, -282.7301404120939310, -331.5756036024696982 ) ) ;
#28584 = CARTESIAN_POINT ( 'NONE',  ( -107.9753013925963501, -292.6018137217848789, -248.2080133815861984 ) ) ;
#28585 = CARTESIAN_POINT ( 'NONE',  ( -21.54077395617752799, -275.8516179978487912, -195.8173647531914412 ) ) ;
#28586 = ADVANCED_FACE ( 'NONE', ( #67325 ), #22358, .T. ) ;
#28587 = CARTESIAN_POINT ( 'NONE',  ( 98.29621670120258159, -300.9199634798632133, -193.7310287357714742 ) ) ;
#28588 = EDGE_CURVE ( 'NONE', #37463, #68679, #29198, .T. ) ;
#28589 = CARTESIAN_POINT ( 'NONE',  ( -35.58260892391334806, -297.0302193835679532, -345.1865871620890971 ) ) ;
#28590 = CARTESIAN_POINT ( 'NONE',  ( -26.50176542822750037, -280.9138818148171595, -344.4577733266178825 ) ) ;
#28591 = CARTESIAN_POINT ( 'NONE',  ( -111.9026155549361476, -289.9786608994671724, -289.5558101779715230 ) ) ;
#28592 = CARTESIAN_POINT ( 'NONE',  ( 33.65498902118835645, -273.8713452967687658, -293.4114310478694847 ) ) ;
#28593 = CARTESIAN_POINT ( 'NONE',  ( 29.42071459036348102, -288.6703062843075145, -233.5199520612079596 ) ) ;
#28594 = CARTESIAN_POINT ( 'NONE',  ( -101.9219384145607989, -289.0001049265405300, -305.1619944745023645 ) ) ;
#28595 = ORIENTED_EDGE ( 'NONE', *, *, #6798, .F. ) ;
#28596 = CARTESIAN_POINT ( 'NONE',  ( -96.84277371914417643, -288.4790977218034982, -318.3216007486200851 ) ) ;
#28597 = CARTESIAN_POINT ( 'NONE',  ( -95.78779648069846075, -289.6043659490258051, -314.1557378135203180 ) ) ;
#28598 = ORIENTED_EDGE ( 'NONE', *, *, #61048, .F. ) ;
#28599 = CARTESIAN_POINT ( 'NONE',  ( -54.90721545993856978, -286.9110891317310461, -195.7089567278675020 ) ) ;
#28600 = CARTESIAN_POINT ( 'NONE',  ( -66.80730314165892025, -277.7825002068363460, -337.1732854813812423 ) ) ;
#28601 = CARTESIAN_POINT ( 'NONE',  ( 29.29922972513464785, -292.9685751236604005, -308.4220048040718893 ) ) ;
#28602 = CARTESIAN_POINT ( 'NONE',  ( -109.2047295540654943, -284.8549974712008748, -297.8776432634088565 ) ) ;
#28603 = CARTESIAN_POINT ( 'NONE',  ( -67.18478086484179812, -286.0047023192887536, -199.4024340622470390 ) ) ;
#28605 = CARTESIAN_POINT ( 'NONE',  ( -35.66656833962258588, -280.4069919106366342, -197.3467840251825862 ) ) ;
#28604 = AXIS2_PLACEMENT_3D ( 'NONE', #45152, #37590, #9170 ) ;
#28606 = CARTESIAN_POINT ( 'NONE',  ( 199.9431822037543895, 289.4637811216681484, -97.53612682803708367 ) ) ;
#28607 = CARTESIAN_POINT ( 'NONE',  ( 172.7456591032144217, 243.4255081464518469, -179.1439596359693951 ) ) ;
#28608 = CARTESIAN_POINT ( 'NONE',  ( 199.8454374018455155, 291.1247744847867693, -82.44697178725743925 ) ) ;
#28609 = CARTESIAN_POINT ( 'NONE',  ( -105.5631175224678060, -272.1033404182197160, -243.7934079629947348 ) ) ;
#28610 = CARTESIAN_POINT ( 'NONE',  ( 11.76373686284951248, -273.6732817008837060, -215.8603904072934085 ) ) ;
#28611 = CARTESIAN_POINT ( 'NONE',  ( -93.64871248334942777, -295.3443503549772799, -322.8118811401897688 ) ) ;
#28612 = CARTESIAN_POINT ( 'NONE',  ( 197.3573331818941199, 281.6218204230049764, -110.3645358861669621 ) ) ;
#28613 = CARTESIAN_POINT ( 'NONE',  ( -89.81238187975995402, -272.0152907662348412, -214.6100140034042738 ) ) ;
#28614 = CARTESIAN_POINT ( 'NONE',  ( -82.71754104506084104, -299.2852353268698948, -211.5430932386634311 ) ) ;
#28615 = CARTESIAN_POINT ( 'NONE',  ( -26.38493765066929697, -290.2251195794141267, -343.0843292747882742 ) ) ;
#28616 = CARTESIAN_POINT ( 'NONE',  ( -47.04894798124955457, -293.0056245913336852, -197.6975410527181225 ) ) ;
#28617 = VERTEX_POINT ( 'NONE', #23753 ) ;
#28618 = CARTESIAN_POINT ( 'NONE',  ( -112.6601639414535896, -297.6802952042838797, -255.4627805770078908 ) ) ;
#28619 = CARTESIAN_POINT ( 'NONE',  ( -62.59001911922237582, -286.2070151452742834, -201.7468910568526894 ) ) ;
#28620 = CARTESIAN_POINT ( 'NONE',  ( 27.97406667447834749, -294.8865092217719734, -310.9334298753838652 ) ) ;
#28621 = CARTESIAN_POINT ( 'NONE',  ( 1.743578206831889688, -295.0363330136170248, -336.6322875867046491 ) ) ;
#28622 = CARTESIAN_POINT ( 'NONE',  ( 20.18158153086591611, -293.0850774663261404, -225.3956698767600528 ) ) ;
#28623 = ORIENTED_EDGE ( 'NONE', *, *, #44041, .F. ) ;
#28624 = CARTESIAN_POINT ( 'NONE',  ( -66.99350518999349902, -275.5866846015036344, -200.8623075148435646 ) ) ;
#28625 = ORIENTED_EDGE ( 'NONE', *, *, #5917, .F. ) ;
#28626 = CARTESIAN_POINT ( 'NONE',  ( -69.93060055712770406, -279.1420517671097059, -200.6510414866850738 ) ) ;
#28627 = PRODUCT_DEFINITION_CONTEXT ( 'detailed design', #62598, 'design' ) ;
#28628 = CARTESIAN_POINT ( 'NONE',  ( 35.16323437238900596, -273.7724060376565376, -256.5961301584999319 ) ) ;
#28629 = CARTESIAN_POINT ( 'NONE',  ( -35.14814744777818589, -299.2852899822167956, -196.9635804436839521 ) ) ;
#28630 = CARTESIAN_POINT ( 'NONE',  ( 11.69520675621157579, -275.6938797878317473, -215.8980822190610809 ) ) ;
#28631 = CARTESIAN_POINT ( 'NONE',  ( -57.86969819946626359, -275.5508479452520874, -197.1451213531220787 ) ) ;
#28632 = CARTESIAN_POINT ( 'NONE',  ( 36.03911415418804154, -273.3526174624257123, -253.1683092593688968 ) ) ;
#28633 = CARTESIAN_POINT ( 'NONE',  ( -108.0660898847512925, -296.9591701710171492, -288.9025687809136684 ) ) ;
#28634 = CARTESIAN_POINT ( 'NONE',  ( 30.02221297379228560, -292.5222135302249740, -299.9833752756852050 ) ) ;
#28635 = DIRECTION ( 'NONE',  ( -1.000000000000000000, 0.000000000000000000, 0.000000000000000000 ) ) ;
#28636 = CARTESIAN_POINT ( 'NONE',  ( -114.1702220533711341, -278.9930361417931977, -274.4727018439157291 ) ) ;
#28637 = CARTESIAN_POINT ( 'NONE',  ( 20.02377983392060656, -276.3558815742215984, -315.5276970628954700 ) ) ;
#28638 = CARTESIAN_POINT ( 'NONE',  ( -54.83547755593648532, -284.5166291460943739, -195.8811473681408017 ) ) ;
#28639 = CARTESIAN_POINT ( 'NONE',  ( -15.50192490817703472, -300.3250948112315655, -195.1870173997247377 ) ) ;
#28640 = CARTESIAN_POINT ( 'NONE',  ( 221.8344101925596306, 0.000000000000000000, -7.000000000000000888 ) ) ;
#28641 = CARTESIAN_POINT ( 'NONE',  ( 27.16803260128937580, -287.2200307440771212, -304.9811733557868934 ) ) ;
#28642 = CARTESIAN_POINT ( 'NONE',  ( -102.7629399610539451, -276.3270049458675430, -304.9737658125844177 ) ) ;
#28643 = CARTESIAN_POINT ( 'NONE',  ( -96.07111906590684214, -277.7450392750235437, -225.9980127734212090 ) ) ;
#28644 = CARTESIAN_POINT ( 'NONE',  ( -112.3926082005458085, -286.5555504912839524, -270.1093041087452775 ) ) ;
#28645 = CARTESIAN_POINT ( 'NONE',  ( -56.69014825028757798, -278.5121529209635582, -341.2148023865774462 ) ) ;
#28646 = DIRECTION ( 'NONE',  ( -1.000000000000000000, 0.000000000000000000, 0.000000000000000000 ) ) ;
#28647 = CARTESIAN_POINT ( 'NONE',  ( 37.39372394057577509, -274.1399261341155125, -285.2290972235209097 ) ) ;
#28648 = CARTESIAN_POINT ( 'NONE',  ( 30.26593218869695789, -275.8298379601324655, -242.4235477907718632 ) ) ;
#28649 = CARTESIAN_POINT ( 'NONE',  ( 25.21069362367574840, -284.1142764797457971, -312.0411667167350060 ) ) ;
#28650 = LINE ( 'NONE', #6405, #88236 ) ;
#28651 = CARTESIAN_POINT ( 'NONE',  ( 36.31039383494378825, -289.2566057811712881, -253.4312189103996502 ) ) ;
#28652 = CARTESIAN_POINT ( 'NONE',  ( 17.42841982436524972, -292.2700949125618308, -321.6728848860828407 ) ) ;
#28653 = ADVANCED_FACE ( 'NONE', ( #8606, #45499 ), #16189, .T. ) ;
#28654 = DIRECTION ( 'NONE',  ( -1.000000000000000000, 0.000000000000000000, 0.000000000000000000 ) ) ;
#28655 = CARTESIAN_POINT ( 'NONE',  ( -19.13335423497906262, -272.9761024779716081, -199.1065105522791896 ) ) ;
#28656 = CARTESIAN_POINT ( 'NONE',  ( 2.930151069906376193, -290.7381477128460574, -207.9380173828699299 ) ) ;
#28657 = CARTESIAN_POINT ( 'NONE',  ( -28.16072294498304274, -126.4832272301380556, -368.1402060870429409 ) ) ;
#28658 = DIRECTION ( 'NONE',  ( 0.9693563597868429804, 0.2456588035076310572, 7.238107246010827522E-15 ) ) ;
#28659 = CARTESIAN_POINT ( 'NONE',  ( -36.11755601511399050, -287.5169839217354593, -346.6709599171697960 ) ) ;
#28660 = CARTESIAN_POINT ( 'NONE',  ( -87.45731342431548683, -285.3651013704769639, -324.6054151949148263 ) ) ;
#28661 = CARTESIAN_POINT ( 'NONE',  ( -111.3674071488271409, -283.0093818693535468, -253.2097705752599097 ) ) ;
#28662 = CARTESIAN_POINT ( 'NONE',  ( -8.244693324677454527, -284.0887481021479175, -337.9535666237158011 ) ) ;
#28663 = CARTESIAN_POINT ( 'NONE',  ( -108.5249953298580436, -285.5780629189009687, -253.4091958844059036 ) ) ;
#28664 = CARTESIAN_POINT ( 'NONE',  ( -98.70659666386923448, -293.1239175678067568, -226.6260487877287346 ) ) ;
#28665 = AXIS2_PLACEMENT_3D ( 'NONE', #81508, #9541, #16655 ) ;
#28666 = CARTESIAN_POINT ( 'NONE',  ( -92.15698610461994633, -273.6279996527131289, -216.3145758656163196 ) ) ;
#28667 = CARTESIAN_POINT ( 'NONE',  ( -110.1608738582254290, -288.3745377523694060, -290.5274795062143198 ) ) ;
#28668 = CARTESIAN_POINT ( 'NONE',  ( -3.994849273332384598, -276.6244627062955033, -339.7801377912581415 ) ) ;
#28670 = CARTESIAN_POINT ( 'NONE',  ( 37.26449636698217205, -295.5010816555038105, -267.9606504731878545 ) ) ;
#28669 = CIRCLE ( 'NONE', #22631, 6.286090667950827715 ) ;
#28671 = CARTESIAN_POINT ( 'NONE',  ( 175.2296996224750103, 250.0000000000000568, 0.000000000000000000 ) ) ;
#28672 = CARTESIAN_POINT ( 'NONE',  ( -54.42813229853333468, -297.7662352645559167, -345.3683826091709648 ) ) ;
#28673 = CARTESIAN_POINT ( 'NONE',  ( -90.00462221785272732, -283.9740084339952659, -219.0254483009370858 ) ) ;
#28674 = CARTESIAN_POINT ( 'NONE',  ( -89.64468680142144308, -277.3149834520348804, -216.5356183031331057 ) ) ;
#28675 = CARTESIAN_POINT ( 'NONE',  ( -55.15283607664092358, -272.3069708041207946, -196.1622555444353964 ) ) ;
#28676 = EDGE_CURVE ( 'NONE', #40166, #73999, #45041, .T. ) ;
#28677 = CARTESIAN_POINT ( 'NONE',  ( 35.45476189744334050, -274.9886787818614948, -277.0370287497797221 ) ) ;
#28678 = CARTESIAN_POINT ( 'NONE',  ( 15.35791437019653038, -294.3332629596289962, -218.7763194314568409 ) ) ;
#28679 = CARTESIAN_POINT ( 'NONE',  ( 26.00216572862364117, -294.9960329119103903, -307.1165679997777715 ) ) ;
#28680 = CARTESIAN_POINT ( 'NONE',  ( -74.35301600703208180, -296.8484562379771319, -337.3790920864740883 ) ) ;
#28681 = CARTESIAN_POINT ( 'NONE',  ( -106.7061191744315352, -296.6893236095895077, -247.4505508893097954 ) ) ;
#28682 = CARTESIAN_POINT ( 'NONE',  ( -74.51469973401995617, -291.5467401008506840, -335.5155315235590479 ) ) ;
#28683 = CARTESIAN_POINT ( 'NONE',  ( -66.57428434567681563, -283.5912626331861475, -341.6105198614217215 ) ) ;
#28684 = CARTESIAN_POINT ( 'NONE',  ( -21.58812544718778170, -272.3916306235416869, -196.2522091890145930 ) ) ;
#28685 = CARTESIAN_POINT ( 'NONE',  ( 22.09152783232254436, -286.7277218172623066, -221.4051028389808664 ) ) ;
#28686 = CARTESIAN_POINT ( 'NONE',  ( -10.64269782588093172, -278.6820632574600722, -340.0677179490696744 ) ) ;
#28687 = CARTESIAN_POINT ( 'NONE',  ( -97.54254689361944486, -284.1903460932551297, -228.6344419062922668 ) ) ;
#28688 = CARTESIAN_POINT ( 'NONE',  ( -45.82551048213237976, -287.1594166383063111, -344.9314914214473902 ) ) ;
#28689 = CARTESIAN_POINT ( 'NONE',  ( 133.9787772367566561, 181.9811788097603937, -239.6702418147338562 ) ) ;
#28690 = CARTESIAN_POINT ( 'NONE',  ( -46.72656677273066350, -285.4375796011000830, -197.8540185774890574 ) ) ;
#28691 = CARTESIAN_POINT ( 'NONE',  ( 36.21412361271706715, -282.4870526845435279, -248.9237189662935350 ) ) ;
#28692 = CARTESIAN_POINT ( 'NONE',  ( -37.51313324917455105, -288.1129661712404300, -347.1386650677256966 ) ) ;
#28693 = CARTESIAN_POINT ( 'NONE',  ( -64.47670133170277040, -281.3040613688663143, -199.1006054706350028 ) ) ;
#28694 = ADVANCED_FACE ( 'NONE', ( #38416 ), #89059, .T. ) ;
#28695 = CARTESIAN_POINT ( 'NONE',  ( -101.6731843001405338, -279.3193833865271358, -311.8673988259027965 ) ) ;
#28696 = CARTESIAN_POINT ( 'NONE',  ( -99.46661477659858974, -278.9152176534990417, -231.9306962631322051 ) ) ;
#28697 = CARTESIAN_POINT ( 'NONE',  ( -88.47805353815522267, -275.3113733633115316, -215.9127545520194644 ) ) ;
#28698 = CARTESIAN_POINT ( 'NONE',  ( 39.71162069869933475, -293.5515123490475276, -270.3099585778629148 ) ) ;
#28699 = CARTESIAN_POINT ( 'NONE',  ( 24.08952345884162227, -286.1500996849189846, -312.7870759143351620 ) ) ;
#28700 = CARTESIAN_POINT ( 'NONE',  ( -37.81076760605006370, -293.6464904254155499, -194.1625589780649079 ) ) ;
#28701 = CARTESIAN_POINT ( 'NONE',  ( -109.5781130771610918, -295.6366126532654448, -257.8660502213547261 ) ) ;
#28702 = CARTESIAN_POINT ( 'NONE',  ( 35.90670947416063541, -283.6448476284422782, -283.6985933199347301 ) ) ;
#28703 = CARTESIAN_POINT ( 'NONE',  ( -108.4966853032510130, -296.4351901858185556, -253.9582044729913264 ) ) ;
#28704 = CARTESIAN_POINT ( 'NONE',  ( -33.56838050155253939, -293.1782717564379936, -193.7631116818319299 ) ) ;
#28705 = CARTESIAN_POINT ( 'NONE',  ( -16.90115065487985646, -280.9746345604610838, -200.1751036696183803 ) ) ;
#28706 = CARTESIAN_POINT ( 'NONE',  ( 13.81662648194687470, -273.8073065629759526, -213.0568152703448277 ) ) ;
#28707 = CARTESIAN_POINT ( 'NONE',  ( -62.72217063166173290, -290.0252844656328080, -343.0062984609721752 ) ) ;
#28708 = CARTESIAN_POINT ( 'NONE',  ( -64.82654988485565184, -281.5468771600368427, -340.9788388213065105 ) ) ;
#28709 = CARTESIAN_POINT ( 'NONE',  ( -112.6201884736154852, -291.0874582914054827, -254.2087439842300398 ) ) ;
#28710 = CARTESIAN_POINT ( 'NONE',  ( -23.77708614465076664, -289.2074546971101654, -342.1630151821632353 ) ) ;
#28711 = CARTESIAN_POINT ( 'NONE',  ( 160.5350683151633291, 249.5000000000000568, 20.22542485937379908 ) ) ;
#28712 = CARTESIAN_POINT ( 'NONE',  ( 119.9254157080543877, 149.4800609170424366, -261.9094989083125142 ) ) ;
#28713 = CARTESIAN_POINT ( 'NONE',  ( 6.105808943458286286, -59.49341857825391600, -350.9694942175905226 ) ) ;
#28714 = CARTESIAN_POINT ( 'NONE',  ( -37.30987171927208834, -277.5523547857346784, -195.3611179825600175 ) ) ;
#28715 = CARTESIAN_POINT ( 'NONE',  ( -74.57918986198156119, -278.7405550429625123, -207.3269355501208508 ) ) ;
#28716 = ORIENTED_EDGE ( 'NONE', *, *, #21995, .F. ) ;
#28717 = CARTESIAN_POINT ( 'NONE',  ( -85.67772412041780683, -278.2846146422053835, -215.2443795324813038 ) ) ;
#28718 = CARTESIAN_POINT ( 'NONE',  ( -2.563298046150888521, -274.1661232291770034, -201.6717726205803558 ) ) ;
#28719 = CARTESIAN_POINT ( 'NONE',  ( 169.1947799176787726, 229.7990775681149671, -190.7372803930986436 ) ) ;
#28720 = CARTESIAN_POINT ( 'NONE',  ( -70.95888190455409017, -278.1919750086883596, -201.7426701361403332 ) ) ;
#28721 = CARTESIAN_POINT ( 'NONE',  ( -81.62167398621286907, -281.6778557905246885, -330.5181259571628516 ) ) ;
#28722 = CARTESIAN_POINT ( 'NONE',  ( -88.93691533465818111, -299.0995654029789534, -214.5053440036580525 ) ) ;
#28723 = CARTESIAN_POINT ( 'NONE',  ( -90.80849229721653160, -291.7600144409868790, -220.5501434730140602 ) ) ;
#28724 = CARTESIAN_POINT ( 'NONE',  ( 18.18720715152066703, -286.9191921688429261, -318.5806597389935746 ) ) ;
#28725 = CARTESIAN_POINT ( 'NONE',  ( -55.31784767184479534, -274.4781564887141485, -195.5936724881837847 ) ) ;
#28726 = CARTESIAN_POINT ( 'NONE',  ( -105.4162409253727191, -272.9060437272266313, -243.8615407598908575 ) ) ;
#28727 = ORIENTED_EDGE ( 'NONE', *, *, #43406, .T. ) ;
#28728 = CARTESIAN_POINT ( 'NONE',  ( 221.8344101925596306, -0.9999999999999991118, 22.50000000000000000 ) ) ;
#28729 = DIRECTION ( 'NONE',  ( 0.000000000000000000, 0.000000000000000000, 1.000000000000000000 ) ) ;
#28730 = CARTESIAN_POINT ( 'NONE',  ( -90.07111969060639467, -281.2346664249291166, -216.1686317819166732 ) ) ;
#28731 = TOROIDAL_SURFACE ( 'NONE', #18101, 203.9779373800640485, 1.000000000000000000 ) ;
#28732 = CARTESIAN_POINT ( 'NONE',  ( 156.1965750133393271, 18.75975317436940415, 8.718057073926352984 ) ) ;
#28733 = CARTESIAN_POINT ( 'NONE',  ( 13.53979385763831722, -281.8644239470314119, -217.5144513001816904 ) ) ;
#28734 = CARTESIAN_POINT ( 'NONE',  ( -70.80875313821908890, -281.3768728751016965, -202.1413966379129761 ) ) ;
#28735 = AXIS2_PLACEMENT_3D ( 'NONE', #63922, #427, #50139 ) ;
#28736 = CARTESIAN_POINT ( 'NONE',  ( -110.4623556885065767, -283.6756369416274310, -265.4374810263855125 ) ) ;
#28737 = CARTESIAN_POINT ( 'NONE',  ( -109.0066130346584146, -280.1610287093493525, -289.7261829295458142 ) ) ;
#28738 = CARTESIAN_POINT ( 'NONE',  ( -24.45635332049452870, -272.6993305283129985, -197.7509529244380531 ) ) ;
#28739 = CARTESIAN_POINT ( 'NONE',  ( 10.19742947581765691, -229.5268262511776527, 22.50000000000000000 ) ) ;
#28740 = CARTESIAN_POINT ( 'NONE',  ( 175.2296996224750103, 15.00000000000000000, -15.00000000000000000 ) ) ;
#28741 = CARTESIAN_POINT ( 'NONE',  ( -25.78414542985145275, -277.7113298125578353, -346.3254632341079287 ) ) ;
#28742 = CARTESIAN_POINT ( 'NONE',  ( 164.7144138485119242, 214.9642006536927568, 22.97375162482067168 ) ) ;
#28743 = CARTESIAN_POINT ( 'NONE',  ( -107.0460999122108348, -276.7225593208636383, -301.7933369777632038 ) ) ;
#28744 = ORIENTED_EDGE ( 'NONE', *, *, #29988, .T. ) ;
#28745 = FACE_OUTER_BOUND ( 'NONE', #7274, .T. ) ;
#28746 = CARTESIAN_POINT ( 'NONE',  ( -78.24530373153159246, -285.5793213021553356, -333.6485734020911309 ) ) ;
#28747 = CARTESIAN_POINT ( 'NONE',  ( 18.60666309637325710, -292.0810507775216820, -223.2189672050852209 ) ) ;
#28748 = CARTESIAN_POINT ( 'NONE',  ( -5.676057623411916886, -287.9951255879259975, -340.4367904498428175 ) ) ;
#28749 = CARTESIAN_POINT ( 'NONE',  ( -65.45768030036708751, -283.9194548355274037, -201.8415027783975972 ) ) ;
#28751 = CARTESIAN_POINT ( 'NONE',  ( 20.28859750513982974, -286.4396493854808909, -316.8016478173460087 ) ) ;
#28750 = CARTESIAN_POINT ( 'NONE',  ( -108.5946758337290277, -283.3677698945090810, -251.9657823873016014 ) ) ;
#28752 = CARTESIAN_POINT ( 'NONE',  ( 16.12559053676564957, -283.4778493002770574, -320.7174535654094143 ) ) ;
#28753 = CARTESIAN_POINT ( 'NONE',  ( -54.84159006591922036, -271.8270095311204386, -197.4313264169590525 ) ) ;
#28754 = CARTESIAN_POINT ( 'NONE',  ( -102.2474340195895337, -282.4248041733705463, -310.2821164963623346 ) ) ;
#28755 = CARTESIAN_POINT ( 'NONE',  ( -69.91558977714404932, -297.4812203197503209, -337.9322058239084186 ) ) ;
#28756 = CARTESIAN_POINT ( 'NONE',  ( -29.62520417999557765, -284.1495032152307090, -195.5915779538694892 ) ) ;
#28757 = CARTESIAN_POINT ( 'NONE',  ( -72.25239122059259955, -280.5194574870578776, -205.9821455148923519 ) ) ;
#28758 = CARTESIAN_POINT ( 'NONE',  ( 6.454555433670044806, -288.6453714791052789, -209.2076132912932849 ) ) ;
#28759 = DIRECTION ( 'NONE',  ( 0.000000000000000000, 0.000000000000000000, 1.000000000000000000 ) ) ;
#28760 = DIRECTION ( 'NONE',  ( -0.000000000000000000, -1.000000000000000000, -0.000000000000000000 ) ) ;
#28761 = CARTESIAN_POINT ( 'NONE',  ( 18.33769170834741757, -294.7640749977289829, -219.2815768396147860 ) ) ;
#28762 = CARTESIAN_POINT ( 'NONE',  ( -79.78422865670603414, -275.6253767921893996, -332.2598985985115405 ) ) ;
#28763 = CARTESIAN_POINT ( 'NONE',  ( -99.89363930626977606, -290.3416422727881923, -225.7358591512989960 ) ) ;
#28764 = CARTESIAN_POINT ( 'NONE',  ( 21.14487628131042385, -292.5788476220254779, -315.3902543919811592 ) ) ;
#28765 = CARTESIAN_POINT ( 'NONE',  ( -64.98618941442560981, -278.3680884398996227, -202.2654082010966476 ) ) ;
#28766 = CARTESIAN_POINT ( 'NONE',  ( -55.57449699715751734, -295.9547298862773914, -198.3466138866595259 ) ) ;
#28767 = CARTESIAN_POINT ( 'NONE',  ( -62.98840970067398359, -293.0262335022118805, -201.4881206174120791 ) ) ;
#28768 = CARTESIAN_POINT ( 'NONE',  ( 10.64812456238589888, -278.9090924074130839, -330.4860931364851808 ) ) ;
#28769 = CARTESIAN_POINT ( 'NONE',  ( -8.666708665526414279, -293.1636797723633094, -341.1309623486849318 ) ) ;
#28770 = CARTESIAN_POINT ( 'NONE',  ( -34.52730176967966003, -290.6164701602526748, -344.1575610847003759 ) ) ;
#28771 = CARTESIAN_POINT ( 'NONE',  ( -69.17788141322843387, -289.8790089403597676, -201.3510858327785229 ) ) ;
#28772 = CARTESIAN_POINT ( 'NONE',  ( -0.6822781721375021924, -289.9805958015573992, -334.2277866984061916 ) ) ;
#28773 = CARTESIAN_POINT ( 'NONE',  ( 154.7659666677360235, 19.56018909072649237, -12.94946946942526189 ) ) ;
#28774 = CARTESIAN_POINT ( 'NONE',  ( -39.95353643232859753, -289.8885107740105695, -343.5256460532460210 ) ) ;
#28775 = DIRECTION ( 'NONE',  ( -0.7071067811864494290, 8.659560562353731078E-17, 0.7071067811866457165 ) ) ;
#28776 = CARTESIAN_POINT ( 'NONE',  ( -104.7990118038442660, -291.2854798970118395, -306.6587738163017320 ) ) ;
#28778 = CARTESIAN_POINT ( 'NONE',  ( -44.30020562026492570, -291.9618328155113431, -197.6427061757321439 ) ) ;
#28777 = CARTESIAN_POINT ( 'NONE',  ( 2.963977390181769422, -278.6100219335698398, -206.6295460341603700 ) ) ;
#28779 = CARTESIAN_POINT ( 'NONE',  ( -111.3181032338351883, -279.1524250212343077, -249.0717761634805356 ) ) ;
#28780 = CARTESIAN_POINT ( 'NONE',  ( 39.39097184169803256, -281.1419173055464285, -264.2095861541766908 ) ) ;
#28781 = CARTESIAN_POINT ( 'NONE',  ( 35.66283086640006417, -285.3306234409656099, -253.1201032097440304 ) ) ;
#28782 = CARTESIAN_POINT ( 'NONE',  ( 196.7383257810085695, 42.27872732282707346, 11.00000000000001243 ) ) ;
#28783 = CARTESIAN_POINT ( 'NONE',  ( 30.43264197193260401, -280.0943313019511720, -300.7775708613740449 ) ) ;
#28784 = CARTESIAN_POINT ( 'NONE',  ( -111.9179442045474673, -282.4497652697301646, -278.3225542173382792 ) ) ;
#28785 = FACE_OUTER_BOUND ( 'NONE', #89706, .T. ) ;
#28786 = CARTESIAN_POINT ( 'NONE',  ( -101.2994228653708149, -277.5846978210195175, -228.6468260384091309 ) ) ;
#28787 = CARTESIAN_POINT ( 'NONE',  ( -39.18623166806359137, -298.9697291282907372, -197.1366063800762163 ) ) ;
#28788 = CARTESIAN_POINT ( 'NONE',  ( 155.8725544043047080, 19.96731923950699894, -14.33077026901615803 ) ) ;
#28789 = CARTESIAN_POINT ( 'NONE',  ( -108.8890314041174321, -292.3891166012578537, -252.2149193404050607 ) ) ;
#28790 = CARTESIAN_POINT ( 'NONE',  ( 38.79493661825399897, -277.0589217242993527, -276.8278665254196653 ) ) ;
#28791 = CARTESIAN_POINT ( 'NONE',  ( 20.03644140286077402, -275.8560013074880999, -315.5458010475625770 ) ) ;
#28792 = CARTESIAN_POINT ( 'NONE',  ( 21.27234464330004471, -296.1957981175326040, -317.1725655096025207 ) ) ;
#28793 = CARTESIAN_POINT ( 'NONE',  ( -40.33663377911964432, -289.2554738408596791, -347.3159333614233333 ) ) ;
#28794 = CARTESIAN_POINT ( 'NONE',  ( 28.49497332547324291, -280.1234953656467610, -307.5466164315567994 ) ) ;
#28795 = CARTESIAN_POINT ( 'NONE',  ( -16.62457428114823443, -292.1459744064137567, -196.2004767964906762 ) ) ;
#28796 = EDGE_CURVE ( 'NONE', #45831, #69300, #62102, .T. ) ;
#28798 = CARTESIAN_POINT ( 'NONE',  ( -93.61295820892578945, -290.2739778298624174, -223.4698693404680228 ) ) ;
#28797 = VECTOR ( 'NONE', #80839, 1000.000000000000000 ) ;
#28799 = CARTESIAN_POINT ( 'NONE',  ( 18.03529585480070807, -292.2587546086457451, -321.0172525842050959 ) ) ;
#28800 = ORIENTED_EDGE ( 'NONE', *, *, #44642, .T. ) ;
#28801 = DIRECTION ( 'NONE',  ( 0.000000000000000000, 0.000000000000000000, 1.000000000000000000 ) ) ;
#28802 = CARTESIAN_POINT ( 'NONE',  ( -9.698385558259470685, -291.9307939020596905, -202.6771470504879744 ) ) ;
#28803 = CARTESIAN_POINT ( 'NONE',  ( -23.68628624284178130, -55.96374926131388605, 22.50000000000000000 ) ) ;
#28804 = CIRCLE ( 'NONE', #43914, 4.000000000000003553 ) ;
#28805 = CARTESIAN_POINT ( 'NONE',  ( 17.40634833298269157, -278.4094976428775681, -226.7417163044926838 ) ) ;
#28806 = CARTESIAN_POINT ( 'NONE',  ( -114.1311705925976128, -295.5846797632743232, -272.4513884326486277 ) ) ;
#28807 = CARTESIAN_POINT ( 'NONE',  ( -99.37870319314350809, -285.2687899150178055, -315.2235987037710174 ) ) ;
#28808 = CARTESIAN_POINT ( 'NONE',  ( -68.77301236666075113, -285.4603964340911375, -204.4605120308521862 ) ) ;
#28809 = CARTESIAN_POINT ( 'NONE',  ( 14.23023762699518535, -277.8320010408476151, -323.0729031931026611 ) ) ;
#28810 = CARTESIAN_POINT ( 'NONE',  ( 33.08367019892872207, -291.8959899469087986, -295.2566704506836004 ) ) ;
#28811 = CARTESIAN_POINT ( 'NONE',  ( 36.30124594681166172, -295.2096529922422405, -262.4719304339528207 ) ) ;
#28812 = CARTESIAN_POINT ( 'NONE',  ( 35.01970173093855720, -274.1848892468259464, -257.9998794282258245 ) ) ;
#28813 = VERTEX_POINT ( 'NONE', #80120 ) ;
#28814 = CARTESIAN_POINT ( 'NONE',  ( 194.9397804919432247, 41.66501297569659101, 13.69433569849578802 ) ) ;
#28815 = CARTESIAN_POINT ( 'NONE',  ( -96.49789439135609825, -295.5559563336266251, -319.6389903965605868 ) ) ;
#28816 = CARTESIAN_POINT ( 'NONE',  ( 36.18534113489588577, -289.6237193719618404, -282.0652704227585446 ) ) ;
#28817 = CARTESIAN_POINT ( 'NONE',  ( 202.3298055824671451, 295.8616505545806490, -54.00000000005272227 ) ) ;
#28818 = CARTESIAN_POINT ( 'NONE',  ( -35.49503363150593316, -299.1544289038358215, -193.6698978566819846 ) ) ;
#28819 = EDGE_CURVE ( 'NONE', #60748, #45831, #1508, .T. ) ;
#28820 = CARTESIAN_POINT ( 'NONE',  ( -11.99440577218066650, -287.0423975113939719, -201.7943086867818749 ) ) ;
#28821 = ORIENTED_EDGE ( 'NONE', *, *, #17291, .T. ) ;
#28822 = CARTESIAN_POINT ( 'NONE',  ( -59.22356883615201895, -278.8343923080984723, -196.7812020120217085 ) ) ;
#28823 = CARTESIAN_POINT ( 'NONE',  ( -11.08420626853754243, -295.3702643978236893, -342.6938683094772955 ) ) ;
#28824 = CARTESIAN_POINT ( 'NONE',  ( -79.86723194037270446, -287.7597614680824449, -333.1292517079456843 ) ) ;
#28825 = CARTESIAN_POINT ( 'NONE',  ( -112.2547608864246058, -297.1070404181467666, -252.6473487767363224 ) ) ;
#28826 = CARTESIAN_POINT ( 'NONE',  ( 33.79698566769963719, -294.1033403992008175, -286.8896772084623876 ) ) ;
#28827 = LINE ( 'NONE', #20785, #92963 ) ;
#28828 = FACE_OUTER_BOUND ( 'NONE', #23228, .T. ) ;
#28829 = CARTESIAN_POINT ( 'NONE',  ( 138.6539576904058606, 130.8284271247462414, -11.67157287525380838 ) ) ;
#28830 = CARTESIAN_POINT ( 'NONE',  ( 24.13311201855888299, -288.4663105816386519, -225.1554189438206208 ) ) ;
#28831 = CARTESIAN_POINT ( 'NONE',  ( -37.37352853689063181, -292.5523547857346784, -350.3611179825600175 ) ) ;
#28832 = CARTESIAN_POINT ( 'NONE',  ( -53.73065286795355178, -279.1958762765853521, -195.1753039448010725 ) ) ;
#28833 = CARTESIAN_POINT ( 'NONE',  ( -99.02953988683130149, -285.9759625273129018, -312.8145669772147812 ) ) ;
#28834 = CARTESIAN_POINT ( 'NONE',  ( -54.81212673754028941, -284.4065485833248772, -195.9743551455837860 ) ) ;
#28835 = CARTESIAN_POINT ( 'NONE',  ( -37.29111180848410356, -287.1313613514339522, -344.8011048372808887 ) ) ;
#28836 = CARTESIAN_POINT ( 'NONE',  ( 38.08518940720618673, -277.3149590415783905, -262.6816036032384432 ) ) ;
#28837 = CARTESIAN_POINT ( 'NONE',  ( -108.5564594920096937, -273.0983046918013315, -254.2196950087486869 ) ) ;
#28838 = ORIENTED_EDGE ( 'NONE', *, *, #82958, .F. ) ;
#28839 = CARTESIAN_POINT ( 'NONE',  ( -23.44187096779099733, -293.5556898561823687, -342.5798080740376577 ) ) ;
#28841 = CARTESIAN_POINT ( 'NONE',  ( -54.50869012156004345, -279.1744200107929146, -199.2512171389226410 ) ) ;
#28840 = CARTESIAN_POINT ( 'NONE',  ( -108.2896682300805367, -278.7789122217877207, -253.1743258968416797 ) ) ;
#28842 = CARTESIAN_POINT ( 'NONE',  ( -1.458348260171868471, -275.5963164111367405, -202.5829683382581550 ) ) ;
#28843 = CARTESIAN_POINT ( 'NONE',  ( -97.37609346310041758, -277.9871065381591961, -222.7808664332428918 ) ) ;
#28844 = CARTESIAN_POINT ( 'NONE',  ( 191.8446247329872847, 278.1462026667327336, -124.7934328400877888 ) ) ;
#28845 = CARTESIAN_POINT ( 'NONE',  ( -109.7812906963783206, -297.6688955621442574, -294.6739131878267131 ) ) ;
#28846 = CARTESIAN_POINT ( 'NONE',  ( -112.3452863284742875, -275.1604526064900824, -261.9424758988611188 ) ) ;
#28847 = CARTESIAN_POINT ( 'NONE',  ( 222.0386546523673985, 36.13108063356137478, 7.000000000000000000 ) ) ;
#28848 = CARTESIAN_POINT ( 'NONE',  ( -60.08753595986023299, -286.8299548504339782, -200.6699921097011270 ) ) ;
#28849 = CARTESIAN_POINT ( 'NONE',  ( -112.8157800602518108, -286.4239573457176107, -261.5499165210116530 ) ) ;
#28850 = CARTESIAN_POINT ( 'NONE',  ( 33.48938999505083558, -286.6618383989097083, -252.2315952118016185 ) ) ;
#28851 = CARTESIAN_POINT ( 'NONE',  ( -99.74224886571371940, -283.4615606868936766, -315.4579204112681055 ) ) ;
#28852 = CARTESIAN_POINT ( 'NONE',  ( -34.25974200469502762, -278.4913776758122594, -196.6128151678672396 ) ) ;
#28853 = CARTESIAN_POINT ( 'NONE',  ( -14.20311892320789937, -288.2157255676131058, -199.7701866989403925 ) ) ;
#28854 = CARTESIAN_POINT ( 'NONE',  ( 34.44009852084044354, -279.8141140215886935, -253.6853530091659366 ) ) ;
#28855 = CARTESIAN_POINT ( 'NONE',  ( -76.60522581770916872, -278.9043858114934551, -332.5467947163360805 ) ) ;
#28856 = CARTESIAN_POINT ( 'NONE',  ( 32.11836292259848591, -275.7421839848446439, -247.5425506151249806 ) ) ;
#28857 = CARTESIAN_POINT ( 'NONE',  ( 21.17572012678067495, -287.0165468532685509, -319.7951168747990778 ) ) ;
#28858 = CARTESIAN_POINT ( 'NONE',  ( -8.090866874796358132, -283.4816052470200134, -341.4706745622053177 ) ) ;
#28859 = CARTESIAN_POINT ( 'NONE',  ( 15.71563345589393990, -282.8172484453177162, -326.0786758621821946 ) ) ;
#28860 = ORIENTED_EDGE ( 'NONE', *, *, #92612, .T. ) ;
#28861 = VERTEX_POINT ( 'NONE', #23290 ) ;
#28862 = CARTESIAN_POINT ( 'NONE',  ( 0.1293585361110431431, -290.4196608702520166, -336.2704337970289430 ) ) ;
#28863 = CARTESIAN_POINT ( 'NONE',  ( -103.3812675367113485, -288.7298279289464062, -309.0933146043315674 ) ) ;
#28864 = CARTESIAN_POINT ( 'NONE',  ( -35.13138682590787454, -297.2776836930663080, -197.1999511348621184 ) ) ;
#28865 = CARTESIAN_POINT ( 'NONE',  ( 13.32242747412087702, -293.7140678336183441, -328.2802986577050319 ) ) ;
#28866 = CARTESIAN_POINT ( 'NONE',  ( -91.11178114890505242, -288.3130445725331015, -320.8289745958236381 ) ) ;
#28867 = CARTESIAN_POINT ( 'NONE',  ( 36.21137097158838714, -291.9050757092118147, -279.0514716277992306 ) ) ;
#28868 = CARTESIAN_POINT ( 'NONE',  ( 35.38747543088187797, -288.6227525034599353, -260.1113101462957502 ) ) ;
#28869 = CARTESIAN_POINT ( 'NONE',  ( -95.99890600148557951, -293.6948066931273615, -223.6242672951989618 ) ) ;
#28870 = CARTESIAN_POINT ( 'NONE',  ( -6.426996150012344700, -290.6462704095212075, -338.6932607126948369 ) ) ;
#28871 = CARTESIAN_POINT ( 'NONE',  ( -112.3565625322728465, -288.6131608099379378, -265.5863046297953360 ) ) ;
#28872 = AXIS2_PLACEMENT_3D ( 'NONE', #70738, #34280, #91055 ) ;
#28873 = CARTESIAN_POINT ( 'NONE',  ( -31.77159710093684097, -294.1224870392187540, -195.5176157910393613 ) ) ;
#28874 = CARTESIAN_POINT ( 'NONE',  ( -97.71955762335068130, -284.9172249295660322, -311.8973144673603883 ) ) ;
#28875 = CARTESIAN_POINT ( 'NONE',  ( 29.26234011649155420, -295.0905173491903497, -235.4076358884279045 ) ) ;
#28876 = CARTESIAN_POINT ( 'NONE',  ( 200.2296996224750103, 68.12454877777268791, -4.440892098500626793E-14 ) ) ;
#28877 = CARTESIAN_POINT ( 'NONE',  ( 164.6148405695019505, 214.9970011440366875, 23.11617803653516035 ) ) ;
#28878 = CARTESIAN_POINT ( 'NONE',  ( -49.47969221070077595, -275.8781716099782670, -195.9372561731233304 ) ) ;
#28879 = CARTESIAN_POINT ( 'NONE',  ( 35.19426935297148873, -280.6186970349644412, -260.4376077522010746 ) ) ;
#28880 = CARTESIAN_POINT ( 'NONE',  ( -10.27718706193942033, -280.6989166951829020, -340.3626569397173398 ) ) ;
#28881 = CARTESIAN_POINT ( 'NONE',  ( -110.6559660482669329, -296.0409708954169332, -247.1809637196172105 ) ) ;
#28882 = CARTESIAN_POINT ( 'NONE',  ( 3.507644941049418819, -272.8492172630388382, -208.5802881947172125 ) ) ;
#28883 = CARTESIAN_POINT ( 'NONE',  ( -108.5002517370127890, -276.3460535014623929, -292.3919735972970102 ) ) ;
#28884 = CARTESIAN_POINT ( 'NONE',  ( -109.2652040852746325, -298.0660697193143278, -255.1924947416337943 ) ) ;
#28885 = CARTESIAN_POINT ( 'NONE',  ( -18.04868583408125460, -296.2237972474559911, -341.3762890027979324 ) ) ;
#28886 = CARTESIAN_POINT ( 'NONE',  ( 151.4851178187871312, 20.00000000000000000, -3.492110388858666870 ) ) ;
#28887 = CARTESIAN_POINT ( 'NONE',  ( -23.47823908267664450, -295.6733556268970915, -342.2488046534497244 ) ) ;
#28888 = CARTESIAN_POINT ( 'NONE',  ( 129.8483263487583201, -299.5541904835127980, -201.6997734963854612 ) ) ;
#28890 = CARTESIAN_POINT ( 'NONE',  ( -106.7067850686869264, -296.8559767729030909, -247.4525667566919651 ) ) ;
#28889 = CARTESIAN_POINT ( 'NONE',  ( -7.960660604380052519, -284.4551204923432692, -200.9142994269091673 ) ) ;
#28891 = CARTESIAN_POINT ( 'NONE',  ( -86.10237042656079609, -283.7070983024665907, -329.9547169009252912 ) ) ;
#28892 = CARTESIAN_POINT ( 'NONE',  ( 38.65341023934551146, -287.3763871517948587, -282.9524159463294382 ) ) ;
#28893 = CARTESIAN_POINT ( 'NONE',  ( -76.21172389521086643, -297.5484079566459172, -334.9782067397379706 ) ) ;
#28894 = CARTESIAN_POINT ( 'NONE',  ( 37.24986043196271623, -291.6293351534392286, -276.3717350595569542 ) ) ;
#28895 = CARTESIAN_POINT ( 'NONE',  ( -82.13641513467004529, -278.6553788043834743, -207.9304177820912969 ) ) ;
#28896 = CARTESIAN_POINT ( 'NONE',  ( -4.829096099716524648, -292.1237833571632905, -337.9475929042657754 ) ) ;
#28897 = CARTESIAN_POINT ( 'NONE',  ( 153.5370352062774089, 129.8649369643341061, 11.69957875851211959 ) ) ;
#28898 = CARTESIAN_POINT ( 'NONE',  ( 30.33381368716085191, -285.9663571425842861, -241.8189539107204951 ) ) ;
#28900 = CARTESIAN_POINT ( 'NONE',  ( 198.5955908591174648, 68.60853014440941422, -10.61435496113653443 ) ) ;
#28899 = CARTESIAN_POINT ( 'NONE',  ( -106.2418717846092164, -289.0369085096439221, -304.1606323191239767 ) ) ;
#28901 = CARTESIAN_POINT ( 'NONE',  ( 207.7039919494849016, 30.29338434242851363, 15.02863188060213773 ) ) ;
#28902 = CARTESIAN_POINT ( 'NONE',  ( -107.6249629562468755, -297.8550489476252210, -293.0364799822762052 ) ) ;
#28903 = CARTESIAN_POINT ( 'NONE',  ( -67.14946832207321847, -281.0941991659597079, -200.0041478300858273 ) ) ;
#28905 = CARTESIAN_POINT ( 'NONE',  ( 22.59970398232882616, -281.7999614411745029, -312.0638224521202346 ) ) ;
#28904 = CARTESIAN_POINT ( 'NONE',  ( -112.7215773493294506, -294.5462066957920229, -272.3995915035764597 ) ) ;
#28906 = CARTESIAN_POINT ( 'NONE',  ( -32.01039082659227830, -295.1533505007510030, -347.1895868161587941 ) ) ;
#28907 = CARTESIAN_POINT ( 'NONE',  ( 23.55745648019969352, -285.0265905837824789, -225.6329733235589572 ) ) ;
#28908 = CARTESIAN_POINT ( 'NONE',  ( -101.7085883252702558, -281.0687960868983737, -231.7645705731140993 ) ) ;
#28909 = EDGE_CURVE ( 'NONE', #17995, #46866, #9057, .T. ) ;
#28910 = CARTESIAN_POINT ( 'NONE',  ( -90.20743865831647668, -296.3406560736297592, -219.6069813580631092 ) ) ;
#28911 = ORIENTED_EDGE ( 'NONE', *, *, #68922, .T. ) ;
#28912 = CARTESIAN_POINT ( 'NONE',  ( 201.2104617360081704, 69.18068689461284748, -10.00000000000000000 ) ) ;
#28913 = CARTESIAN_POINT ( 'NONE',  ( -1.619842738583425090, -284.5561992301912824, -335.9180515230037827 ) ) ;
#28914 = CARTESIAN_POINT ( 'NONE',  ( 128.9960186029002500, -299.5541904835127980, -189.6092331708328800 ) ) ;
#28915 = CARTESIAN_POINT ( 'NONE',  ( -54.42813229853333468, -283.3380690714491266, -195.3538533559490702 ) ) ;
#28916 = CARTESIAN_POINT ( 'NONE',  ( 3.407182085537348915, -275.7167100639817932, -335.5673362482120865 ) ) ;
#28917 = CARTESIAN_POINT ( 'NONE',  ( -14.84438489160445585, -292.1852371359844369, -200.9142259596434883 ) ) ;
#28918 = CARTESIAN_POINT ( 'NONE',  ( 35.83059945120395184, -283.1920351565196370, -279.5254299274858454 ) ) ;
#28919 = CARTESIAN_POINT ( 'NONE',  ( 20.46960276339095586, -276.5115508354709277, -224.4683240407934761 ) ) ;
#28920 = CARTESIAN_POINT ( 'NONE',  ( -27.45549092336016983, -284.5288100451078321, -345.9698869229168281 ) ) ;
#28921 = CARTESIAN_POINT ( 'NONE',  ( 35.82350422358431530, -280.4315655279017392, -276.8011701266889872 ) ) ;
#28922 = CARTESIAN_POINT ( 'NONE',  ( -110.5647853983429343, -280.7613765760755768, -254.0732343844262004 ) ) ;
#28923 = CARTESIAN_POINT ( 'NONE',  ( -94.14669870041457500, -273.4260333062524069, -218.3590358660443087 ) ) ;
#28924 = CARTESIAN_POINT ( 'NONE',  ( 37.59137671681521908, -275.6077516816897628, -288.1389085637092649 ) ) ;
#28925 = CARTESIAN_POINT ( 'NONE',  ( 36.86177358847764651, -295.5490182836845179, -276.2905938707750124 ) ) ;
#28926 = SPHERICAL_SURFACE ( 'NONE', #30915, 1.000000000000000000 ) ;
#28927 = ADVANCED_FACE ( 'NONE', ( #37935 ), #37034, .T. ) ;
#28928 = DIRECTION ( 'NONE',  ( 0.000000000000000000, 0.000000000000000000, -1.000000000000000000 ) ) ;
#28929 = CARTESIAN_POINT ( 'NONE',  ( -30.72284203198544361, -293.1089005543605026, -345.8362542708027263 ) ) ;
#28930 = CARTESIAN_POINT ( 'NONE',  ( -62.04461048427199188, -273.2297477483849093, -201.6024482632961110 ) ) ;
#28931 = AXIS2_PLACEMENT_3D ( 'NONE', #13448, #42298, #19593 ) ;
#28932 = CARTESIAN_POINT ( 'NONE',  ( 30.27548918993041127, -294.6105560745963317, -234.8832662389708048 ) ) ;
#28934 = CARTESIAN_POINT ( 'NONE',  ( 3.914688565619278471, -293.7991844086780588, -205.7543195144860420 ) ) ;
#28933 = CARTESIAN_POINT ( 'NONE',  ( -88.52914483777347243, -299.9090924074130271, -206.2264541496106460 ) ) ;
#28935 = CARTESIAN_POINT ( 'NONE',  ( 19.22774422849473908, -290.2339909411588792, -319.4277797221233186 ) ) ;
#28936 = CARTESIAN_POINT ( 'NONE',  ( -109.3763318661992088, -276.8139732446758217, -250.0395553538179456 ) ) ;
#28937 = CARTESIAN_POINT ( 'NONE',  ( -86.02895724524111642, -279.6528627423621742, -326.7398146488165480 ) ) ;
#28938 = CARTESIAN_POINT ( 'NONE',  ( 36.97392133928026681, -291.5657582740174121, -265.2411900562795495 ) ) ;
#28939 = CARTESIAN_POINT ( 'NONE',  ( 14.30178325449721477, -282.6287310706824769, -214.8524646059202894 ) ) ;
#28940 = CARTESIAN_POINT ( 'NONE',  ( -69.15569715810329399, -282.4011002079937498, -336.4211440577749954 ) ) ;
#28941 = ORIENTED_EDGE ( 'NONE', *, *, #61608, .F. ) ;
#28942 = CARTESIAN_POINT ( 'NONE',  ( -67.79705522980630406, -283.1299678863632607, -336.7279683861327726 ) ) ;
#28943 = CARTESIAN_POINT ( 'NONE',  ( 10.61894207598172279, -281.7764719849806738, -210.4493539139551501 ) ) ;
#28944 = CARTESIAN_POINT ( 'NONE',  ( -96.87356453975938564, -282.6969799694008998, -318.5892648632062105 ) ) ;
#28945 = CARTESIAN_POINT ( 'NONE',  ( -106.1291973049916066, -279.0527584682786824, -304.5556003163956120 ) ) ;
#28946 = CARTESIAN_POINT ( 'NONE',  ( 34.55429637435049273, -277.3996438837572214, -296.0840157304401146 ) ) ;
#28947 = CARTESIAN_POINT ( 'NONE',  ( 30.91033621190086578, -296.2662352645559167, -285.9065529553535612 ) ) ;
#28948 = VERTEX_POINT ( 'NONE', #1059 ) ;
#28949 = ORIENTED_EDGE ( 'NONE', *, *, #48544, .T. ) ;
#28950 = CARTESIAN_POINT ( 'NONE',  ( 10.49848309132422131, -300.6511726817209365, -195.3447991607771144 ) ) ;
#28951 = CARTESIAN_POINT ( 'NONE',  ( -86.20047067655202966, -275.7534441357573201, -326.8624646329412258 ) ) ;
#28952 = CARTESIAN_POINT ( 'NONE',  ( -61.38942291493036407, -293.5043150331485435, -198.2246214958697408 ) ) ;
#28953 = CARTESIAN_POINT ( 'NONE',  ( 27.24424671980931834, -293.3678520085264836, -304.7117541904410132 ) ) ;
#28954 = CARTESIAN_POINT ( 'NONE',  ( -114.1901376725091808, -290.0132347255718628, -274.0819445104036731 ) ) ;
#28955 = CARTESIAN_POINT ( 'NONE',  ( 200.3186454232214828, 250.0000000000000568, -3.421094783296261710 ) ) ;
#28957 = CARTESIAN_POINT ( 'NONE',  ( -6.665582515039180755, -284.8616166645765020, -203.2248413037354169 ) ) ;
#28956 = CARTESIAN_POINT ( 'NONE',  ( 38.64905473251574364, -292.2338358891450412, -278.8475973002811088 ) ) ;
#28958 = CARTESIAN_POINT ( 'NONE',  ( -96.10646393974624857, -293.0405384886427669, -225.0006945102907139 ) ) ;
#28959 = CARTESIAN_POINT ( 'NONE',  ( -41.34138630994763020, -284.4807912425298468, -196.7637859125881619 ) ) ;
#28960 = CARTESIAN_POINT ( 'NONE',  ( -34.81290807134679710, -284.3349348120583500, -343.8232720601941423 ) ) ;
#28961 = CARTESIAN_POINT ( 'NONE',  ( -20.53620572476283002, -289.7828224393147707, -345.3181941518132589 ) ) ;
#28962 = CARTESIAN_POINT ( 'NONE',  ( -5.537367688399023713, -280.9745577941933448, -204.5851886470320835 ) ) ;
#28963 = MANIFOLD_SOLID_BREP ( 'Fillet12', #46108 ) ;
#28964 = CARTESIAN_POINT ( 'NONE',  ( 38.83300420412186327, -292.2392755668338395, -261.7856932072620566 ) ) ;
#28965 = CARTESIAN_POINT ( 'NONE',  ( 14.50231543153340041, -289.1478536772306143, -327.1461622820708612 ) ) ;
#28966 = CARTESIAN_POINT ( 'NONE',  ( -1.823553757975173717, -289.0866774293936032, -338.6105735251213673 ) ) ;
#28967 = CARTESIAN_POINT ( 'NONE',  ( -12.02397293614165008, -286.5577425152166597, -201.8920542067419035 ) ) ;
#28968 = ORIENTED_EDGE ( 'NONE', *, *, #13331, .T. ) ;
#28969 = CARTESIAN_POINT ( 'NONE',  ( 144.2857639756989272, -299.5541904835127980, -195.3611179825600175 ) ) ;
#28970 = CARTESIAN_POINT ( 'NONE',  ( -44.65246856521751795, -297.0040102630856040, -345.8249270846321224 ) ) ;
#28971 = CARTESIAN_POINT ( 'NONE',  ( -111.1209207622825801, -294.9817350258296642, -290.6077195803351287 ) ) ;
#28972 = CARTESIAN_POINT ( 'NONE',  ( -110.1989010009386760, -277.7150034526537752, -262.4437083242016229 ) ) ;
#28973 = CARTESIAN_POINT ( 'NONE',  ( -41.18341899833677644, -273.5128063552895696, -193.4664108989695706 ) ) ;
#28974 = CARTESIAN_POINT ( 'NONE',  ( -38.37121490453610306, -293.5451649047367937, -344.0472622282470638 ) ) ;
#28975 = CARTESIAN_POINT ( 'NONE',  ( 16.16406211547253591, -276.5839931826102998, -219.1488325899674692 ) ) ;
#28976 = CARTESIAN_POINT ( 'NONE',  ( -62.42514791531172591, -271.8618995807586316, -200.4920538214416865 ) ) ;
#28977 = CARTESIAN_POINT ( 'NONE',  ( 28.75879494706067163, -295.1880379515787354, -302.3822187649667512 ) ) ;
#28978 = CARTESIAN_POINT ( 'NONE',  ( -15.48762485314155590, -295.8423641450490891, -340.3904097115009222 ) ) ;
#28979 = CARTESIAN_POINT ( 'NONE',  ( -43.47202469644348355, -255.6311900920820790, -443.8813325122532660 ) ) ;
#28980 = CARTESIAN_POINT ( 'NONE',  ( -111.9518616527507504, -294.6689553754105191, -261.2313741163425220 ) ) ;
#28981 = CARTESIAN_POINT ( 'NONE',  ( -26.23635635124255572, -298.8391810069481949, -193.4618585974712346 ) ) ;
#28982 = CARTESIAN_POINT ( 'NONE',  ( -95.34082787328908637, -275.2080839381553687, -222.7899847489195508 ) ) ;
#28983 = CARTESIAN_POINT ( 'NONE',  ( -103.0512861727144696, -291.0566334374165081, -302.6977651373611025 ) ) ;
#28984 = CARTESIAN_POINT ( 'NONE',  ( -0.7436776325022109724, -294.8852612765637105, -333.6064252522456854 ) ) ;
#28985 = CARTESIAN_POINT ( 'NONE',  ( -108.0712897170277955, -280.8694747177243016, -244.2154874713867230 ) ) ;
#28986 = CARTESIAN_POINT ( 'NONE',  ( -106.9633565252325269, -277.6464864830326746, -238.5141826871370938 ) ) ;
#28987 = CARTESIAN_POINT ( 'NONE',  ( -5.505300626159884025, -281.9928251520344702, -340.3593783448894214 ) ) ;
#28988 = CARTESIAN_POINT ( 'NONE',  ( 31.76003758802262311, -275.3358754356679015, -304.2205244116261724 ) ) ;
#28989 = CARTESIAN_POINT ( 'NONE',  ( -42.35684137575063346, -278.3897723389686121, -194.3263313773717300 ) ) ;
#28990 = CARTESIAN_POINT ( 'NONE',  ( -76.51480461952797896, -277.5296757884241288, -206.1487385595294768 ) ) ;
#28991 = EDGE_CURVE ( 'NONE', #74935, #79053, #81498, .T. ) ;
#28992 = CARTESIAN_POINT ( 'NONE',  ( -84.37769171075041186, -296.0741399835027323, -213.8247033711687664 ) ) ;
#28993 = CARTESIAN_POINT ( 'NONE',  ( -17.16330074450739218, -276.3126586687073427, -198.0734089972396816 ) ) ;
#28994 = DIRECTION ( 'NONE',  ( -0.000000000000000000, 0.000000000000000000, 1.000000000000000000 ) ) ;
#28995 = CIRCLE ( 'NONE', #12354, 0.4999999999999996114 ) ;
#28996 = CARTESIAN_POINT ( 'NONE',  ( -19.74583758605215422, -290.2972542834143610, -197.0354181444677977 ) ) ;
#28997 = CARTESIAN_POINT ( 'NONE',  ( -108.7984607606721568, -290.1880890298560871, -299.0478982113800726 ) ) ;
#28998 = CARTESIAN_POINT ( 'NONE',  ( -24.49852348394544421, -276.2157303263848576, -196.2469100033235065 ) ) ;
#28999 = CARTESIAN_POINT ( 'NONE',  ( -106.2062619362709057, -270.9421275431236609, -240.5198000244643026 ) ) ;
#29000 = CARTESIAN_POINT ( 'NONE',  ( -111.5625583934719316, -284.0010943134173544, -250.2759955948271511 ) ) ;
#29001 = CARTESIAN_POINT ( 'NONE',  ( 209.4593673012390127, 36.32691179220002198, 14.77866956795211273 ) ) ;
#29002 = AXIS2_PLACEMENT_3D ( 'NONE', #43885, #66163, #45736 ) ;
#29003 = CARTESIAN_POINT ( 'NONE',  ( -110.8748008331861428, -282.3616430174290031, -285.1860755719627605 ) ) ;
#29004 = CARTESIAN_POINT ( 'NONE',  ( 208.4306832106270804, -147.7221692137691775, 8.500000000000007105 ) ) ;
#29005 = CARTESIAN_POINT ( 'NONE',  ( 26.58791597075114410, -291.8549687587049561, -234.1999249923817956 ) ) ;
#29006 = CARTESIAN_POINT ( 'NONE',  ( -95.91733887330151731, -283.3238627160918668, -224.7360988177030094 ) ) ;
#29007 = CARTESIAN_POINT ( 'NONE',  ( 164.7123623445222904, 3.000000000000000000, 10.00000000000000178 ) ) ;
#29008 = LINE ( 'NONE', #72561, #21627 ) ;
#29009 = CARTESIAN_POINT ( 'NONE',  ( 36.01866949154955932, -291.7530438872581726, -286.0193155949615971 ) ) ;
#29010 = CARTESIAN_POINT ( 'NONE',  ( -73.96043540945811401, -282.0089730032079842, -337.3661485315952291 ) ) ;
#29011 = CARTESIAN_POINT ( 'NONE',  ( -67.10683697970357287, -279.0491425883923284, -337.8924221682263465 ) ) ;
#29012 = CARTESIAN_POINT ( 'NONE',  ( -46.47346337248296066, -287.1437782387467905, -194.3044311099714889 ) ) ;
#29013 = CARTESIAN_POINT ( 'NONE',  ( 34.28415687976975335, -287.7389726811379091, -284.5231338214018706 ) ) ;
#29014 = CARTESIAN_POINT ( 'NONE',  ( -69.49259107951876047, -278.9090272880847579, -336.5694392468197975 ) ) ;
#29015 = CARTESIAN_POINT ( 'NONE',  ( -100.7176125718345361, -278.8536731337037509, -307.0154808950087499 ) ) ;
#29016 = CARTESIAN_POINT ( 'NONE',  ( -86.45986791267628746, -287.3706700735061190, -213.6142503674073510 ) ) ;
#29017 = VERTEX_POINT ( 'NONE', #32728 ) ;
#29018 = CARTESIAN_POINT ( 'NONE',  ( -68.17550808821938801, -297.4917492424456782, -199.7474200918037184 ) ) ;
#29019 = CARTESIAN_POINT ( 'NONE',  ( -56.46314082938407353, -291.2795465154296721, -342.5689762963320391 ) ) ;
#29020 = CARTESIAN_POINT ( 'NONE',  ( 197.2369698562987992, 24.81718856582945776, 11.94944555321362500 ) ) ;
#29021 = CARTESIAN_POINT ( 'NONE',  ( 44.71564893372296723, -284.0519495502702512, -270.3284710469131937 ) ) ;
#29022 = EDGE_LOOP ( 'NONE', ( #10470, #67848, #1361, #77970, #29205 ) ) ;
#29023 = CARTESIAN_POINT ( 'NONE',  ( 35.59791381397667465, -292.2337612449141488, -292.5908475678988339 ) ) ;
#29024 = CARTESIAN_POINT ( 'NONE',  ( 35.24695587551692455, -288.9024075812861838, -257.3617023465223497 ) ) ;
#29025 = CARTESIAN_POINT ( 'NONE',  ( -32.92462837685746990, -281.8687089084618265, -196.4797029203458578 ) ) ;
#29026 = CARTESIAN_POINT ( 'NONE',  ( 20.14170289193872065, -289.6638870726213781, -320.7223159298603719 ) ) ;
#29027 = CARTESIAN_POINT ( 'NONE',  ( 2.934854232252313455, -289.8390752478499621, -335.4701596716221275 ) ) ;
#29028 = CARTESIAN_POINT ( 'NONE',  ( -86.14440799429006290, -285.7291711685608675, -327.3110639944490003 ) ) ;
#29029 = CARTESIAN_POINT ( 'NONE',  ( -113.7173849210784340, -278.8462860324142980, -260.1699688639847068 ) ) ;
#29030 = VERTEX_POINT ( 'NONE', #89523 ) ;
#29031 = CARTESIAN_POINT ( 'NONE',  ( -44.68056695131800637, -293.2240498334932113, -345.6162875106165302 ) ) ;
#29032 = CARTESIAN_POINT ( 'NONE',  ( 34.32520115508302894, -281.0268715361618774, -242.0578943965372503 ) ) ;
#29033 = CARTESIAN_POINT ( 'NONE',  ( -107.4810670066979270, -274.7305812070057414, -246.0437436730007335 ) ) ;
#29034 = LINE ( 'NONE', #65051, #79325 ) ;
#29035 = CARTESIAN_POINT ( 'NONE',  ( -110.4542110544635705, -292.8376638359844719, -287.0812184334320705 ) ) ;
#29036 = CARTESIAN_POINT ( 'NONE',  ( -63.19103103557907275, -271.9598535799216847, -198.9063343454448045 ) ) ;
#29037 = CARTESIAN_POINT ( 'NONE',  ( -70.96441198728437882, -279.1036397310989514, -205.4817611755388782 ) ) ;
#29038 = CARTESIAN_POINT ( 'NONE',  ( 20.53039896733878322, -277.4390960191549311, -320.5689112606822846 ) ) ;
#29039 = CARTESIAN_POINT ( 'NONE',  ( -52.77624482539867046, -299.2759051960790657, -198.3563983033112663 ) ) ;
#29040 = CARTESIAN_POINT ( 'NONE',  ( -99.60468865110435388, -283.0127284061310888, -315.3514211874347097 ) ) ;
#29041 = CARTESIAN_POINT ( 'NONE',  ( -103.7448378495758732, -291.8753908846409217, -303.0505247013063581 ) ) ;
#29042 = CARTESIAN_POINT ( 'NONE',  ( -37.62469496349078213, -299.5687839072248266, -194.0549736053249319 ) ) ;
#29043 = CARTESIAN_POINT ( 'NONE',  ( -112.2156779358013807, -297.9613861491866373, -254.1166292051446192 ) ) ;
#29044 = CARTESIAN_POINT ( 'NONE',  ( -41.10660323687478979, -297.0997811996043652, -345.1125715942354759 ) ) ;
#29045 = CARTESIAN_POINT ( 'NONE',  ( -95.73109890873644190, -281.9066092731093818, -317.1864960370452309 ) ) ;
#29046 = CARTESIAN_POINT ( 'NONE',  ( -113.1504587761377962, -290.3861378248961387, -256.9903886155433952 ) ) ;
#29047 = CARTESIAN_POINT ( 'NONE',  ( -92.31723490415963340, -271.2811946360124011, -219.8492604868421552 ) ) ;
#29048 = CARTESIAN_POINT ( 'NONE',  ( -57.56345499142655342, -287.3956018723699231, -196.8385141738557138 ) ) ;
#29049 = EDGE_CURVE ( 'NONE', #66900, #60939, #24687, .T. ) ;
#29050 = CARTESIAN_POINT ( 'NONE',  ( -66.67518959869019568, -290.5789104255426878, -203.1765031529651537 ) ) ;
#29051 = CARTESIAN_POINT ( 'NONE',  ( -88.93230042470179342, -231.1883730374851496, -347.8443031440752975 ) ) ;
#29052 = VERTEX_POINT ( 'NONE', #69643 ) ;
#29053 = CARTESIAN_POINT ( 'NONE',  ( -111.4188318680573531, -289.3637765323534836, -251.5685398234625438 ) ) ;
#29054 = CARTESIAN_POINT ( 'NONE',  ( 22.76489284886658737, -287.7964449033113965, -311.8474175847650827 ) ) ;
#29055 = ORIENTED_EDGE ( 'NONE', *, *, #33498, .T. ) ;
#29056 = CARTESIAN_POINT ( 'NONE',  ( -102.2641411289027644, -286.1685318409749925, -229.5374831143345489 ) ) ;
#29057 = CARTESIAN_POINT ( 'NONE',  ( -43.20455690560347506, -277.4615066705574691, -343.1465175980730464 ) ) ;
#29058 = EDGE_CURVE ( 'NONE', #48695, #78455, #27654, .T. ) ;
#29059 = CARTESIAN_POINT ( 'NONE',  ( 39.40230404837005551, -292.4720146818851845, -270.3238875060144437 ) ) ;
#29060 = CARTESIAN_POINT ( 'NONE',  ( -88.24783923721381029, -284.3942640320466921, -328.0679437294831473 ) ) ;
#29061 = CARTESIAN_POINT ( 'NONE',  ( -5.724965787271730555, -284.1640090736559046, -339.8095871122327480 ) ) ;
#29062 = CARTESIAN_POINT ( 'NONE',  ( -99.76883797504858364, -284.2870556920759100, -315.4901381478383655 ) ) ;
#29063 = CARTESIAN_POINT ( 'NONE',  ( 21.34343563640646124, -281.2761103640312967, -226.8873150514334043 ) ) ;
#29064 = CARTESIAN_POINT ( 'NONE',  ( 161.7396164022935920, 220.2077545383955055, -205.3692606286431328 ) ) ;
#29065 = CIRCLE ( 'NONE', #330, 0.4999999999999922839 ) ;
#29066 = CARTESIAN_POINT ( 'NONE',  ( 188.5613963121770951, 271.4186816058274871, -139.2599248928845554 ) ) ;
#29067 = CARTESIAN_POINT ( 'NONE',  ( -13.84510484761940674, -91.62221105869700466, -356.6869422256752387 ) ) ;
#29068 = CARTESIAN_POINT ( 'NONE',  ( -59.51486978482670764, -272.9548539942754246, -200.5875524095781088 ) ) ;
#29069 = CARTESIAN_POINT ( 'NONE',  ( -33.44423038639822465, -294.5120093366608103, -347.2139082883693959 ) ) ;
#29070 = CARTESIAN_POINT ( 'NONE',  ( -46.54096165037511668, -155.7550357926132563, -361.7467890835505386 ) ) ;
#29071 = CARTESIAN_POINT ( 'NONE',  ( -73.69567043240977000, -272.2651325181229254, -202.9844239935560779 ) ) ;
#29072 = CARTESIAN_POINT ( 'NONE',  ( -95.43246076348934537, -299.0543825337038584, -224.1406786409301617 ) ) ;
#29073 = CARTESIAN_POINT ( 'NONE',  ( 35.48248658103275233, -288.7328330255010087, -260.0965237433304083 ) ) ;
#29074 = ORIENTED_EDGE ( 'NONE', *, *, #25349, .T. ) ;
#29075 = CARTESIAN_POINT ( 'NONE',  ( -53.22880859076300908, -296.1921927033925499, -345.5182221984113653 ) ) ;
#29076 = VECTOR ( 'NONE', #20970, 1000.000000000000000 ) ;
#29077 = CARTESIAN_POINT ( 'NONE',  ( 26.41802359045723136, -287.5556859434273065, -234.5828957379837618 ) ) ;
#29078 = CARTESIAN_POINT ( 'NONE',  ( -5.231116456524945946, -273.3852703353703077, -200.7162838074785327 ) ) ;
#29079 = PRODUCT_RELATED_PRODUCT_CATEGORY ( 'part', '', ( #28567 ) ) ;
#29080 = CARTESIAN_POINT ( 'NONE',  ( 1.696222031992290491, -295.3467683073545800, -336.5441932651527281 ) ) ;
#29081 = CARTESIAN_POINT ( 'NONE',  ( -4.523087606019172036, -295.1235927253036380, -339.9634032918083335 ) ) ;
#29082 = CARTESIAN_POINT ( 'NONE',  ( -110.1224613021566938, -290.6361096159917565, -276.6320202256051743 ) ) ;
#29083 = ORIENTED_EDGE ( 'NONE', *, *, #70067, .F. ) ;
#29084 = CARTESIAN_POINT ( 'NONE',  ( -5.739231721537038311, -276.3846104338207397, -201.7273202418811024 ) ) ;
#29085 = CARTESIAN_POINT ( 'NONE',  ( 29.60800248004706248, -273.8608169705200339, -233.0263933446041733 ) ) ;
#29086 = ORIENTED_EDGE ( 'NONE', *, *, #53233, .T. ) ;
#29087 = CARTESIAN_POINT ( 'NONE',  ( -114.0183494559465345, -277.9727153105167190, -277.3192688016152943 ) ) ;
#29088 = CARTESIAN_POINT ( 'NONE',  ( 7.836552397029881156, -273.0810117970672195, -212.0056048599940084 ) ) ;
#29089 = CARTESIAN_POINT ( 'NONE',  ( -56.95749592203973322, -274.8729576808760839, -199.6721604216728849 ) ) ;
#29090 = CARTESIAN_POINT ( 'NONE',  ( 22.66550013739908920, -277.0780269395269784, -312.4308675841695617 ) ) ;
#29091 = CARTESIAN_POINT ( 'NONE',  ( 25.29638150318346490, -276.7367111557689441, -227.3212688693693337 ) ) ;
#29092 = CARTESIAN_POINT ( 'NONE',  ( 35.29331601246170891, -273.8296556770546886, -290.4730998508809421 ) ) ;
#29093 = CARTESIAN_POINT ( 'NONE',  ( -12.96644529667286605, -295.3784107777237296, -339.3328077123313733 ) ) ;
#29094 = CARTESIAN_POINT ( 'NONE',  ( 34.01298760567167534, -292.3624934326741140, -288.3578803892060023 ) ) ;
#29095 = FACE_OUTER_BOUND ( 'NONE', #56992, .T. ) ;
#29096 = CARTESIAN_POINT ( 'NONE',  ( -111.7663152143852017, -278.7995440758169821, -289.9193693193631702 ) ) ;
#29097 = CARTESIAN_POINT ( 'NONE',  ( 18.99749941439776180, -275.0609477616424670, -223.9402756868155393 ) ) ;
#29098 = CARTESIAN_POINT ( 'NONE',  ( -69.56974447718572208, -284.3216321490796759, -200.9591563923111721 ) ) ;
#29099 = CARTESIAN_POINT ( 'NONE',  ( -100.0349930674739909, -299.1113143510482359, -228.8698566592242400 ) ) ;
#29100 = CARTESIAN_POINT ( 'NONE',  ( 165.2494399300530290, -11.64849832608277325, -3.999999999999998224 ) ) ;
#29101 = CARTESIAN_POINT ( 'NONE',  ( -27.80540380412180568, -285.3735181291838217, -197.8238118626960045 ) ) ;
#29102 = CARTESIAN_POINT ( 'NONE',  ( -104.0539731783285760, -276.3628978860571124, -302.5335886159700749 ) ) ;
#29103 = CARTESIAN_POINT ( 'NONE',  ( -24.24240343840943623, -275.4564811043995860, -342.8269542996873724 ) ) ;
#29104 = CARTESIAN_POINT ( 'NONE',  ( -76.02661583374984389, -285.5686600949732110, -334.6734646758580425 ) ) ;
#29105 = CARTESIAN_POINT ( 'NONE',  ( 9.931441982945049318, -277.5887519358110467, -326.5071823024180162 ) ) ;
#29106 = CARTESIAN_POINT ( 'NONE',  ( 155.7140808774799723, 20.00000000000000355, 15.62500000000000000 ) ) ;
#29107 = CARTESIAN_POINT ( 'NONE',  ( 11.29094710910536925, -273.1126274212361409, -211.6298916813352662 ) ) ;
#29108 = CARTESIAN_POINT ( 'NONE',  ( 35.74464626691104741, -276.1836842788366084, -268.8516020120518419 ) ) ;
#29109 = CARTESIAN_POINT ( 'NONE',  ( -17.50101914013604798, -282.3077298326380742, -197.8602503900464740 ) ) ;
#29110 = CARTESIAN_POINT ( 'NONE',  ( 214.2238915819278589, 32.98517505407394168, 10.50000000000000000 ) ) ;
#29111 = CARTESIAN_POINT ( 'NONE',  ( 33.49558159549865621, -289.1335185447226763, -244.0667513925443473 ) ) ;
#29112 = CARTESIAN_POINT ( 'NONE',  ( 34.77791310673228509, -291.2865290003802556, -249.7297042914721601 ) ) ;
#29113 = DIRECTION ( 'NONE',  ( 0.000000000000000000, 1.000000000000000000, 0.000000000000000000 ) ) ;
#29114 = CARTESIAN_POINT ( 'NONE',  ( -44.59312579435954405, -296.7534150013375438, -197.2724766090933883 ) ) ;
#29115 = CARTESIAN_POINT ( 'NONE',  ( -108.1732005711365900, -288.9818407512015597, -248.0975386458894718 ) ) ;
#29116 = CARTESIAN_POINT ( 'NONE',  ( -110.5532707284312579, -275.4615312476335589, -297.1751512281608143 ) ) ;
#29117 = CARTESIAN_POINT ( 'NONE',  ( 198.7793562774353404, 65.30699008317354526, -10.61576606199975714 ) ) ;
#29118 = CARTESIAN_POINT ( 'NONE',  ( -20.66694027677849732, -287.3218445494675848, -344.8777644420810020 ) ) ;
#29119 = CARTESIAN_POINT ( 'NONE',  ( -34.79878517241586167, -284.6198431166550904, -344.1298700032400575 ) ) ;
#29120 = CARTESIAN_POINT ( 'NONE',  ( -66.77557355800242078, -283.9116180920170223, -200.3067026336862284 ) ) ;
#29121 = CARTESIAN_POINT ( 'NONE',  ( -53.80396825775465430, -284.6927346109205246, -342.1378737106871313 ) ) ;
#29122 = CARTESIAN_POINT ( 'NONE',  ( -108.8757939604941356, -285.1522222404969398, -285.7657808063830203 ) ) ;
#29123 = CARTESIAN_POINT ( 'NONE',  ( -97.89818579242142960, -293.1414589367479948, -225.4917633979897005 ) ) ;
#29124 = CIRCLE ( 'NONE', #44240, 35.00000000000002842 ) ;
#29125 = CARTESIAN_POINT ( 'NONE',  ( -73.93855528857008608, -273.9133214114679049, -202.5787884180904541 ) ) ;
#29126 = VECTOR ( 'NONE', #88842, 1000.000000000000000 ) ;
#29127 = CARTESIAN_POINT ( 'NONE',  ( -101.9712361042727053, -289.1538301272617559, -231.1152126964408922 ) ) ;
#29128 = CARTESIAN_POINT ( 'NONE',  ( -91.32903597740350676, -277.7941952117706137, -325.3390414846945760 ) ) ;
#29129 = CARTESIAN_POINT ( 'NONE',  ( 37.28745169635097056, -295.5729872885106602, -273.5342989218363527 ) ) ;
#29130 = CARTESIAN_POINT ( 'NONE',  ( -48.18343439339133027, -258.3625464905466629, -448.5700876443984839 ) ) ;
#29131 = CARTESIAN_POINT ( 'NONE',  ( -37.37352853689063892, -294.5519495502701943, -195.3611179825600175 ) ) ;
#29132 = CARTESIAN_POINT ( 'NONE',  ( -10.81328570904239328, -281.3837926511320688, -338.9532680287605899 ) ) ;
#29133 = CIRCLE ( 'NONE', #44185, 204.0731808058633590 ) ;
#29134 = CARTESIAN_POINT ( 'NONE',  ( -95.25635016124610388, -277.2094317784462305, -222.6872571060159487 ) ) ;
#29135 = CARTESIAN_POINT ( 'NONE',  ( -49.58870742807535947, -272.3787209193567946, -194.9903466706304869 ) ) ;
#29136 = CARTESIAN_POINT ( 'NONE',  ( 26.72985948596472028, -274.4193969354574278, -235.0600287624716316 ) ) ;
#29137 = AXIS2_PLACEMENT_3D ( 'NONE', #77058, #41030, #63350 ) ;
#29138 = CARTESIAN_POINT ( 'NONE',  ( 20.71728216863201055, -294.4383003060963802, -224.9549889925963555 ) ) ;
#29139 = CARTESIAN_POINT ( 'NONE',  ( 13.05642461154988254, -293.7187528058617545, -217.2250899937149597 ) ) ;
#29140 = CARTESIAN_POINT ( 'NONE',  ( 12.87746693168394074, -294.1625748489303760, -212.7708275576423489 ) ) ;
#29141 = CARTESIAN_POINT ( 'NONE',  ( 38.73387060940101634, -294.7591191398213368, -261.7645859195664002 ) ) ;
#29142 = CARTESIAN_POINT ( 'NONE',  ( -102.7691010398401232, -295.9452183478330767, -302.8521253715268244 ) ) ;
#29143 = CARTESIAN_POINT ( 'NONE',  ( -106.9602979986835152, -292.1872567162244536, -298.3975410176632295 ) ) ;
#29144 = CARTESIAN_POINT ( 'NONE',  ( -18.91633803435625794, -282.9881023005478369, -345.1790751643713406 ) ) ;
#29145 = CARTESIAN_POINT ( 'NONE',  ( -27.13901650990876746, -272.3199669271991183, -195.2338429297683717 ) ) ;
#29146 = CARTESIAN_POINT ( 'NONE',  ( 12.07920372808245801, -286.5505921830846887, -211.2443200335937092 ) ) ;
#29147 = CARTESIAN_POINT ( 'NONE',  ( -84.01601927443815043, -279.6765865250532670, -328.6801328073227637 ) ) ;
#29148 = CARTESIAN_POINT ( 'NONE',  ( -25.09069824947386707, -285.2708164133159130, -198.1063198607274671 ) ) ;
#29149 = CARTESIAN_POINT ( 'NONE',  ( -40.28641619419729381, -287.0889835343469940, -345.3160326648110185 ) ) ;
#29150 = CARTESIAN_POINT ( 'NONE',  ( -39.52749759425856269, -278.1646025339778134, -194.6150090660700300 ) ) ;
#29151 = CARTESIAN_POINT ( 'NONE',  ( 175.8323451578035872, 256.8656992060370499, -165.6361338323774817 ) ) ;
#29152 = CARTESIAN_POINT ( 'NONE',  ( -101.8284908261481689, -283.5909078835904324, -304.8118204259590698 ) ) ;
#29153 = CARTESIAN_POINT ( 'NONE',  ( 26.40003754083123511, -283.3193200034374968, -312.8464048170004048 ) ) ;
#29154 = CARTESIAN_POINT ( 'NONE',  ( 3.046116274273402258, -287.5830129726841733, -335.7047413454131402 ) ) ;
#29155 = CARTESIAN_POINT ( 'NONE',  ( -111.6264491077817382, -280.3668226175572613, -253.3841780930724497 ) ) ;
#29156 = CARTESIAN_POINT ( 'NONE',  ( -94.82910094152910574, -279.1797260664491205, -320.8437587737985837 ) ) ;
#29157 = CARTESIAN_POINT ( 'NONE',  ( -105.5135257091426411, -278.7358286499509177, -244.1120337001885616 ) ) ;
#29158 = CARTESIAN_POINT ( 'NONE',  ( -72.70881258811427017, -275.5616681384973390, -204.5690950504262275 ) ) ;
#29159 = CARTESIAN_POINT ( 'NONE',  ( 39.44106649991496738, -293.4798670779348981, -264.5812608086622504 ) ) ;
#29160 = CARTESIAN_POINT ( 'NONE',  ( -29.01410478942843341, -286.9661779110084012, -344.5399421679449006 ) ) ;
#29161 = CARTESIAN_POINT ( 'NONE',  ( -79.17245378939333023, -293.0984648964697499, -206.6063663710047820 ) ) ;
#29162 = AXIS2_PLACEMENT_3D ( 'NONE', #78292, #43678, #614 ) ;
#29163 = CARTESIAN_POINT ( 'NONE',  ( -105.2534035761517544, -295.1042164483267811, -297.9695697255476716 ) ) ;
#29164 = CARTESIAN_POINT ( 'NONE',  ( 29.50771087166731377, -293.6140288923708113, -299.7421277621942295 ) ) ;
#29165 = CARTESIAN_POINT ( 'NONE',  ( -58.86515589873064869, -292.8597201375199575, -196.7524679427423280 ) ) ;
#29166 = CARTESIAN_POINT ( 'NONE',  ( 2.752970255155656520, -281.2568265818979967, -209.1750191052834964 ) ) ;
#29167 = EDGE_CURVE ( 'NONE', #74948, #9812, #7963, .T. ) ;
#29168 = CARTESIAN_POINT ( 'NONE',  ( -33.34066139994413902, -297.0214765620827393, -193.6709412598685844 ) ) ;
#29169 = CARTESIAN_POINT ( 'NONE',  ( -74.37094452355594854, -290.1826304870281206, -337.7716094566268339 ) ) ;
#29170 = CARTESIAN_POINT ( 'NONE',  ( -33.15113654118997744, -281.1395202298446634, -346.0228669787665012 ) ) ;
#29171 = CARTESIAN_POINT ( 'NONE',  ( -99.00964989773964930, -290.2720389287857756, -316.4568578516767730 ) ) ;
#29172 = CARTESIAN_POINT ( 'NONE',  ( -4.588881145092316594, -286.8293658582298349, -205.0974961436477315 ) ) ;
#29173 = DIRECTION ( 'NONE',  ( 0.7957555401921969640, 0.6056179655966498210, 0.000000000000000000 ) ) ;
#29174 = CARTESIAN_POINT ( 'NONE',  ( 82.97595463368493540, 83.32078986060837167, -300.5379249362064797 ) ) ;
#29175 = CARTESIAN_POINT ( 'NONE',  ( -82.68567550127887955, -218.7616381193585369, -348.8841751239126552 ) ) ;
#29176 = CARTESIAN_POINT ( 'NONE',  ( -109.4469695386476928, -277.5852997139115246, -282.8219877990129021 ) ) ;
#29177 = CARTESIAN_POINT ( 'NONE',  ( -14.19830883110518727, -279.2796668975616967, -200.7473343617472210 ) ) ;
#29178 = CARTESIAN_POINT ( 'NONE',  ( 39.68618914801349717, -275.2290613558049586, -271.1756566901154315 ) ) ;
#29179 = CARTESIAN_POINT ( 'NONE',  ( 7.539219266477946491, -59.96618086862105912, -352.3314556225434444 ) ) ;
#29180 = CARTESIAN_POINT ( 'NONE',  ( -111.8232840950418705, -277.3419118533252572, -253.2994666690804877 ) ) ;
#29181 = CARTESIAN_POINT ( 'NONE',  ( -51.35076606621438344, -281.2521097727154142, -343.7322939613135304 ) ) ;
#29182 = CARTESIAN_POINT ( 'NONE',  ( 35.40617110913215981, -295.5934885642024028, -292.4876899309440432 ) ) ;
#29183 = CARTESIAN_POINT ( 'NONE',  ( -60.28423373526529616, -292.2390053195602491, -200.9421277696114885 ) ) ;
#29184 = CARTESIAN_POINT ( 'NONE',  ( -97.76383482057222807, -288.6577371769941465, -312.2211252530668730 ) ) ;
#29185 = CARTESIAN_POINT ( 'NONE',  ( 38.82207225999194122, -276.0708005949307449, -259.7595821425560416 ) ) ;
#29186 = CARTESIAN_POINT ( 'NONE',  ( -109.8042172097347873, -296.5968520368127201, -279.6079501035316071 ) ) ;
#29187 = ORIENTED_EDGE ( 'NONE', *, *, #38462, .T. ) ;
#29188 = CARTESIAN_POINT ( 'NONE',  ( -113.5000000000000568, -218.8335761803644743, -447.4016117689005796 ) ) ;
#29189 = CARTESIAN_POINT ( 'NONE',  ( 196.4697998462662270, 24.53660424933035600, 13.19104620540694306 ) ) ;
#29190 = TOROIDAL_SURFACE ( 'NONE', #62522, 1.000000000000000000, 0.5000000000000000000 ) ;
#29191 = CARTESIAN_POINT ( 'NONE',  ( -85.89841427233375271, -281.3061899865826376, -212.4002453333106644 ) ) ;
#29192 = CIRCLE ( 'NONE', #42837, 4.000000000000003553 ) ;
#29193 = AXIS2_PLACEMENT_3D ( 'NONE', #82520, #10539, #3444 ) ;
#29194 = CARTESIAN_POINT ( 'NONE',  ( -38.37195606870359654, -281.1186155180223523, -197.0467910506306737 ) ) ;
#29195 = CARTESIAN_POINT ( 'NONE',  ( -79.36923148431291963, -281.2537324225068005, -206.9919011014411296 ) ) ;
#29196 = CARTESIAN_POINT ( 'NONE',  ( -29.43111246164405159, -282.0083793114825994, -343.2185905112864361 ) ) ;
#29197 = CARTESIAN_POINT ( 'NONE',  ( 20.41082872211825716, -273.3918059169424737, -224.5658914370737023 ) ) ;
#29199 = CARTESIAN_POINT ( 'NONE',  ( 209.8744251295252070, 28.03846817292547655, 13.95110425196124737 ) ) ;
#29198 = CIRCLE ( 'NONE', #3430, 1.000000000000000888 ) ;
#29200 = DIRECTION ( 'NONE',  ( 0.000000000000000000, 0.000000000000000000, -1.000000000000000000 ) ) ;
#29201 = CARTESIAN_POINT ( 'NONE',  ( 22.52164770151876283, -277.0021341095891216, -318.5539008113069031 ) ) ;
#29202 = LINE ( 'NONE', #6504, #11176 ) ;
#29203 = CARTESIAN_POINT ( 'NONE',  ( 36.51795177621814759, -277.3840819300374392, -257.2589640638132664 ) ) ;
#29204 = CARTESIAN_POINT ( 'NONE',  ( -34.33260792502838399, -275.5897465108141660, -346.7126186761420854 ) ) ;
#29205 = ORIENTED_EDGE ( 'NONE', *, *, #34990, .T. ) ;
#29206 = CARTESIAN_POINT ( 'NONE',  ( 208.6392664839860061, 27.72544851617926298, 12.02381566707519944 ) ) ;
#29207 = CARTESIAN_POINT ( 'NONE',  ( -94.99526159398773473, -285.8641524627857962, -318.9039933696400908 ) ) ;
#29208 = CIRCLE ( 'NONE', #77605, 0.5000000000000003331 ) ;
#29209 = CARTESIAN_POINT ( 'NONE',  ( 33.93041027460741788, -292.9674106166887100, -286.9355972965731780 ) ) ;
#29210 = CARTESIAN_POINT ( 'NONE',  ( -2.261994383531324093, -285.8526435615632408, -201.9159302307698454 ) ) ;
#29211 = CARTESIAN_POINT ( 'NONE',  ( -81.24500300977861400, -281.8975713842697814, -330.0107499586101198 ) ) ;
#29213 = CARTESIAN_POINT ( 'NONE',  ( -7.658711325376004631, -284.5241356925522496, -202.0952086587204235 ) ) ;
#29212 = CARTESIAN_POINT ( 'NONE',  ( -32.12187460345364798, -281.5597411000109673, -343.7649893997270851 ) ) ;
#29214 = CARTESIAN_POINT ( 'NONE',  ( 27.21152764206630437, -283.2312158833216245, -305.2897779658824220 ) ) ;
#29215 = CARTESIAN_POINT ( 'NONE',  ( 25.27517611454112867, -272.9947051450940307, -229.0800392881023981 ) ) ;
#29216 = CARTESIAN_POINT ( 'NONE',  ( -64.24547228200616189, -284.1067889720205244, -199.0545507684197162 ) ) ;
#29217 = CARTESIAN_POINT ( 'NONE',  ( -110.0239771372214506, -298.3140285296810816, -288.9139008688837862 ) ) ;
#29218 = CIRCLE ( 'NONE', #82122, 24.99999999999999645 ) ;
#29219 = CARTESIAN_POINT ( 'NONE',  ( -108.9925003029575805, -279.2941737878839490, -285.5127279019183106 ) ) ;
#29220 = CARTESIAN_POINT ( 'NONE',  ( -8.080888646031574751, -288.4345302546277594, -201.0683073677778907 ) ) ;
#29221 = CARTESIAN_POINT ( 'NONE',  ( 197.0002228694559960, 291.9912828655285466, -7.756604549753964406 ) ) ;
#29222 = EDGE_CURVE ( 'NONE', #61220, #18301, #4307, .T. ) ;
#29223 = EDGE_CURVE ( 'NONE', #72640, #66586, #83839, .T. ) ;
#29224 = CYLINDRICAL_SURFACE ( 'NONE', #42830, 0.9999999999999954481 ) ;
#29225 = CARTESIAN_POINT ( 'NONE',  ( 34.99832134895100211, -295.7534755775664621, -292.3613768722133273 ) ) ;
#29226 = AXIS2_PLACEMENT_3D ( 'NONE', #43119, #7588, #50692 ) ;
#29227 = CARTESIAN_POINT ( 'NONE',  ( -112.2794960780222056, -276.5127736138019827, -273.4151946129711064 ) ) ;
#29228 = CARTESIAN_POINT ( 'NONE',  ( -89.38962818188210235, -288.9604741283120006, -326.8869705227680811 ) ) ;
#29229 = CARTESIAN_POINT ( 'NONE',  ( 6.522246961676673394, -292.8450356590520869, -329.7745567149770523 ) ) ;
#29230 = CARTESIAN_POINT ( 'NONE',  ( -110.7735600908295623, -277.1976498108247142, -273.3620210332728675 ) ) ;
#29231 = CARTESIAN_POINT ( 'NONE',  ( -99.46853136960000086, -295.2466248455440336, -229.6341334135434806 ) ) ;
#29232 = CARTESIAN_POINT ( 'NONE',  ( -91.13146940179331068, -292.5827084799610134, -220.2635266549310984 ) ) ;
#29233 = CARTESIAN_POINT ( 'NONE',  ( 31.95455697924148097, -277.6233781216988064, -236.9535640164627353 ) ) ;
#29234 = CARTESIAN_POINT ( 'NONE',  ( 19.00451588280505533, -292.7387156367883563, -321.8949498740161062 ) ) ;
#29235 = CARTESIAN_POINT ( 'NONE',  ( -56.25112352216549283, -290.8998438329404053, -341.7505921185205011 ) ) ;
#29236 = CARTESIAN_POINT ( 'NONE',  ( -92.06652323086579770, -289.5240729087989848, -217.5684731567962729 ) ) ;
#29237 = CARTESIAN_POINT ( 'NONE',  ( 34.59047430127931477, -289.1813606261325731, -285.9488803882938441 ) ) ;
#29238 = CARTESIAN_POINT ( 'NONE',  ( 197.8477145984406889, 64.61450673763175701, 7.741079165001056417 ) ) ;
#29239 = CARTESIAN_POINT ( 'NONE',  ( -63.86993052914272084, -290.2098368975118774, -338.5979298408167324 ) ) ;
#29240 = CARTESIAN_POINT ( 'NONE',  ( 208.6208076322478746, 32.98517505407394168, 14.69807322781335657 ) ) ;
#29241 = CARTESIAN_POINT ( 'NONE',  ( 18.36664193314086191, -289.4789523294811033, -322.9404803148823930 ) ) ;
#29242 = CARTESIAN_POINT ( 'NONE',  ( -78.98046635984833586, -277.5143013959537370, -207.4923281208132266 ) ) ;
#29243 = CARTESIAN_POINT ( 'NONE',  ( -11.52044663751431131, -280.7126117459726515, -197.7861401916131001 ) ) ;
#29244 = CARTESIAN_POINT ( 'NONE',  ( 37.65786152474048976, -281.0012496004908940, -252.9593128452560222 ) ) ;
#29245 = CARTESIAN_POINT ( 'NONE',  ( 22.76137158689731166, -286.1649596487548024, -315.2448564677266063 ) ) ;
#29246 = CARTESIAN_POINT ( 'NONE',  ( 196.1970748449012376, 41.31174257127814542, 11.68933045232663659 ) ) ;
#29247 = CARTESIAN_POINT ( 'NONE',  ( 36.65827000853134621, -279.7763308771675383, -276.8828409284703866 ) ) ;
#29248 = CARTESIAN_POINT ( 'NONE',  ( -67.66808405344656308, -283.6541095774777546, -201.7518474469312366 ) ) ;
#29249 = CARTESIAN_POINT ( 'NONE',  ( -101.6168586613798226, -254.6069401012266837, -324.2417600373901791 ) ) ;
#29250 = CARTESIAN_POINT ( 'NONE',  ( -95.36587843930522013, -277.7067649605712631, -220.7839922678124935 ) ) ;
#29251 = CARTESIAN_POINT ( 'NONE',  ( -110.6265477432470448, -283.7595028859212789, -247.5810751916764332 ) ) ;
#29252 = CARTESIAN_POINT ( 'NONE',  ( -52.69608049951457929, -298.7919627706066308, -198.7014422940439715 ) ) ;
#29253 = CARTESIAN_POINT ( 'NONE',  ( -25.29839699456137225, -293.8082183287192493, -197.4983689543639400 ) ) ;
#29254 = CARTESIAN_POINT ( 'NONE',  ( -111.8726039430083148, -274.1897108684652835, -253.5162175010727310 ) ) ;
#29255 = CARTESIAN_POINT ( 'NONE',  ( 27.88207604144076157, -274.7734016328113285, -237.5290222701762559 ) ) ;
#29256 = CARTESIAN_POINT ( 'NONE',  ( -7.160732329261499274, -296.6564308431242125, -339.0344453613610085 ) ) ;
#29257 = CARTESIAN_POINT ( 'NONE',  ( -17.72227886142927034, -288.9725431679455596, -344.8196857477736330 ) ) ;
#29258 = AXIS2_PLACEMENT_3D ( 'NONE', #38153, #23508, #66147 ) ;
#29259 = CARTESIAN_POINT ( 'NONE',  ( 33.23362328162392743, -279.9802170391257619, -297.3507071184428128 ) ) ;
#29260 = CARTESIAN_POINT ( 'NONE',  ( 13.28007226992709633, -292.5708787839383263, -212.3401203716051668 ) ) ;
#29261 = CARTESIAN_POINT ( 'NONE',  ( -37.53858739657136567, -291.1084099755564694, -197.1136035078857276 ) ) ;
#29262 = AXIS2_PLACEMENT_3D ( 'NONE', #73373, #23157, #88488 ) ;
#29263 = CARTESIAN_POINT ( 'NONE',  ( 20.72167270563129904, -292.2064658009685445, -317.8538452146927398 ) ) ;
#29264 = VERTEX_POINT ( 'NONE', #54488 ) ;
#29265 = DIRECTION ( 'NONE',  ( 1.000000000000000000, -0.000000000000000000, 0.000000000000000000 ) ) ;
#29266 = AXIS2_PLACEMENT_3D ( 'NONE', #37447, #51649, #37902 ) ;
#29267 = CARTESIAN_POINT ( 'NONE',  ( -85.96531210550035951, -290.8645795948653472, -215.7610847968657595 ) ) ;
#29268 = CARTESIAN_POINT ( 'NONE',  ( -4.884362290657007222, -287.4104553945318798, -200.7957427265180286 ) ) ;
#29269 = CARTESIAN_POINT ( 'NONE',  ( -82.13390479932378696, -299.9090924074130271, -214.2458315076590907 ) ) ;
#29270 = CARTESIAN_POINT ( 'NONE',  ( 1.639595032869546998, -293.6029651139949124, -336.4918887361526458 ) ) ;
#29271 = CARTESIAN_POINT ( 'NONE',  ( -113.7148909600849720, -285.8001219697132456, -275.7001598946342256 ) ) ;
#29272 = CARTESIAN_POINT ( 'NONE',  ( -83.64623087291148806, -285.2297540012796730, -213.8606071217083127 ) ) ;
#29273 = VECTOR ( 'NONE', #88118, 1000.000000000000000 ) ;
#29274 = CARTESIAN_POINT ( 'NONE',  ( -21.48514559712777938, -278.3654041614892094, -342.3808043153999279 ) ) ;
#29275 = CARTESIAN_POINT ( 'NONE',  ( 35.03484017148956298, -291.8079632433044708, -288.6226409280334906 ) ) ;
#29276 = CARTESIAN_POINT ( 'NONE',  ( 35.20536456878092224, -295.1215613726804463, -255.7017380611010253 ) ) ;
#29277 = CARTESIAN_POINT ( 'NONE',  ( 32.89190705290275218, -274.6283159817035084, -291.7206337176042439 ) ) ;
#29278 = EDGE_LOOP ( 'NONE', ( #72356, #12541, #22828 ) ) ;
#29279 = CARTESIAN_POINT ( 'NONE',  ( 195.8903875302077893, 41.38157328953137437, 12.21596753353894549 ) ) ;
#29280 = CARTESIAN_POINT ( 'NONE',  ( 24.86668721480743827, -293.8210822821598072, -315.7249218374769271 ) ) ;
#29281 = CARTESIAN_POINT ( 'NONE',  ( 25.46620039976995287, -290.0140475019359769, -310.3171166358277446 ) ) ;
#29282 = CARTESIAN_POINT ( 'NONE',  ( -67.97253149468437528, -295.6499112059328240, -201.8875048730719186 ) ) ;
#29283 = CIRCLE ( 'NONE', #41345, 7.500000000000007105 ) ;
#29284 = CARTESIAN_POINT ( 'NONE',  ( -86.18782160283986116, -296.7913387945891941, -329.4842854023831364 ) ) ;
#29285 = CARTESIAN_POINT ( 'NONE',  ( -35.93981945779435705, -286.7216110189032747, -197.2726277867202214 ) ) ;
#29286 = CARTESIAN_POINT ( 'NONE',  ( -111.6028824227297633, -277.3661766502970636, -289.8575166249461290 ) ) ;
#29287 = CARTESIAN_POINT ( 'NONE',  ( -5.831873850135859350, -295.3000434646322105, -340.5069919516442951 ) ) ;
#29288 = CARTESIAN_POINT ( 'NONE',  ( -3.631936701984918692, -286.7517272837823157, -338.2279774776856698 ) ) ;
#29289 = CARTESIAN_POINT ( 'NONE',  ( -113.6310857095020737, -296.7519522179055116, -281.0311381682540173 ) ) ;
#29290 = CARTESIAN_POINT ( 'NONE',  ( -102.4303384963426424, -291.3361796951817837, -237.1499812616203258 ) ) ;
#29291 = CARTESIAN_POINT ( 'NONE',  ( 196.7846939763287821, 69.56630120087481828, -10.93783953956503652 ) ) ;
#29292 = DIRECTION ( 'NONE',  ( 0.000000000000000000, 0.000000000000000000, 1.000000000000000000 ) ) ;
#29293 = CARTESIAN_POINT ( 'NONE',  ( 199.4771156391435909, 285.7106110357494799, -96.36288505264877813 ) ) ;
#29294 = CARTESIAN_POINT ( 'NONE',  ( 26.54658699536406985, -288.5191017968975302, -228.6358915518084132 ) ) ;
#29295 = CARTESIAN_POINT ( 'NONE',  ( 36.57525178469694538, -285.4809262143061801, -305.9938812882205070 ) ) ;
#29296 = ORIENTED_EDGE ( 'NONE', *, *, #43478, .F. ) ;
#29297 = CARTESIAN_POINT ( 'NONE',  ( -111.2369941724989815, -278.1678896626916071, -249.0820600895909536 ) ) ;
#29298 = CARTESIAN_POINT ( 'NONE',  ( -65.99468213782841985, -285.4280788798551498, -339.5056209625559518 ) ) ;
#29299 = CARTESIAN_POINT ( 'NONE',  ( -110.5487124253690752, -282.8495047764516244, -292.3004167816417862 ) ) ;
#29300 = CARTESIAN_POINT ( 'NONE',  ( -12.83645460561090346, -286.8109863193118372, -340.6519931993403247 ) ) ;
#29301 = CARTESIAN_POINT ( 'NONE',  ( 37.91362374878300301, -277.5296628082317056, -279.5738039945867399 ) ) ;
#29302 = AXIS2_PLACEMENT_3D ( 'NONE', #44842, #73745, #37735 ) ;
#29303 = CARTESIAN_POINT ( 'NONE',  ( -109.4226045148370474, -296.8872537692310516, -282.2914014885336655 ) ) ;
#29304 = ORIENTED_EDGE ( 'NONE', *, *, #3303, .F. ) ;
#29305 = CARTESIAN_POINT ( 'NONE',  ( -15.46187376323332430, -293.4479043495455244, -340.5752933853732998 ) ) ;
#29306 = CARTESIAN_POINT ( 'NONE',  ( -41.01184010622842635, -280.6585464203695324, -193.5375054045942704 ) ) ;
#29308 = CARTESIAN_POINT ( 'NONE',  ( -105.6065024531201288, -278.2511735350688582, -244.0696297045502661 ) ) ;
#29307 = CARTESIAN_POINT ( 'NONE',  ( -97.99360814509853412, -279.1174730904012904, -229.6469081054717947 ) ) ;
#29309 = CARTESIAN_POINT ( 'NONE',  ( 37.64025098092676558, -276.4288790567144929, -254.1994124060468323 ) ) ;
#29310 = CARTESIAN_POINT ( 'NONE',  ( -39.96620078074518290, -276.0047035939931561, -347.0201001841069228 ) ) ;
#29311 = CARTESIAN_POINT ( 'NONE',  ( -100.2453943390851236, -246.1090379458852624, -332.2849923024065220 ) ) ;
#29312 = CARTESIAN_POINT ( 'NONE',  ( -74.30528925763134396, -296.9585367403147984, -337.2956196989208024 ) ) ;
#29313 = CARTESIAN_POINT ( 'NONE',  ( -43.18343439339132317, -253.0206516614774159, -465.6442049081569508 ) ) ;
#29314 = CARTESIAN_POINT ( 'NONE',  ( 82.62159395231145709, -301.6989411204110638, -194.0647457283005224 ) ) ;
#29315 = CARTESIAN_POINT ( 'NONE',  ( -25.10369573999069104, -287.2914145170660163, -198.0291962984408372 ) ) ;
#29316 = AXIS2_PLACEMENT_3D ( 'NONE', #20071, #71216, #48469 ) ;
#29317 = CARTESIAN_POINT ( 'NONE',  ( -96.80166308453296153, -286.9541282856457087, -223.0484682661965792 ) ) ;
#29318 = CARTESIAN_POINT ( 'NONE',  ( -0.9478882906663393948, -287.9042454304174044, -333.8179859903800093 ) ) ;
#29319 = CARTESIAN_POINT ( 'NONE',  ( 21.55885624896204789, -281.7268570729345925, -319.8611317393966260 ) ) ;
#29320 = CARTESIAN_POINT ( 'NONE',  ( -109.2705305424456839, -276.7358167689553170, -286.9303279340336985 ) ) ;
#29321 = CARTESIAN_POINT ( 'NONE',  ( -102.8502652135940423, -285.9432923757050276, -305.3917056556606440 ) ) ;
#29322 = CARTESIAN_POINT ( 'NONE',  ( -101.4050829579864939, -277.5261855262379527, -233.9387247141416140 ) ) ;
#29323 = CARTESIAN_POINT ( 'NONE',  ( -3.626410889033343743, -277.9125844165016019, -335.6644314573221095 ) ) ;
#29324 = CARTESIAN_POINT ( 'NONE',  ( -0.5206695426793234160, -275.0480880899304452, -207.2418393351161967 ) ) ;
#29325 = CARTESIAN_POINT ( 'NONE',  ( -29.03556492624219132, -287.7441644428831751, -346.5656431372566431 ) ) ;
#29326 = CARTESIAN_POINT ( 'NONE',  ( -14.28597327597590372, -281.1464063719410547, -197.0073684124253930 ) ) ;
#29327 = CARTESIAN_POINT ( 'NONE',  ( 23.35823728496385598, -282.6767960259183496, -317.6586672783503218 ) ) ;
#29328 = VERTEX_POINT ( 'NONE', #62075 ) ;
#29329 = VERTEX_POINT ( 'NONE', #76747 ) ;
#29330 = CARTESIAN_POINT ( 'NONE',  ( 175.2296996224750103, 249.5000000000000568, 0.000000000000000000 ) ) ;
#29331 = CARTESIAN_POINT ( 'NONE',  ( -84.37897997720746446, -291.5516279490882425, -329.8233233905046404 ) ) ;
#29332 = CARTESIAN_POINT ( 'NONE',  ( -97.78039800873339971, -288.6065142076912480, -317.2702010392779925 ) ) ;
#29333 = CARTESIAN_POINT ( 'NONE',  ( -48.90079259854451976, -272.9601759853975977, -197.9924531407881716 ) ) ;
#29334 = CARTESIAN_POINT ( 'NONE',  ( -98.26241506037216311, -290.5279766158877237, -223.4145625515403708 ) ) ;
#29335 = CARTESIAN_POINT ( 'NONE',  ( -7.959686154167663119, -287.1400919220389483, -337.9982419961565938 ) ) ;
#29336 = EDGE_CURVE ( 'NONE', #13609, #11375, #54861, .T. ) ;
#29337 = CARTESIAN_POINT ( 'NONE',  ( -34.80034623468725385, -290.3243715381823904, -196.3914246220124369 ) ) ;
#29338 = CARTESIAN_POINT ( 'NONE',  ( 20.68075937321216529, -289.3870619719614297, -315.3317201925223685 ) ) ;
#29339 = CARTESIAN_POINT ( 'NONE',  ( -54.49178911615187815, -294.3376638359846424, -195.3683826091709363 ) ) ;
#29340 = VECTOR ( 'NONE', #69848, 1000.000000000000114 ) ;
#29341 = CARTESIAN_POINT ( 'NONE',  ( 37.60706707357442724, -289.6027893337953287, -274.2920378283252489 ) ) ;
#29342 = CARTESIAN_POINT ( 'NONE',  ( -67.56760762968578149, -289.6564177005360534, -201.5254206859607962 ) ) ;
#29343 = CARTESIAN_POINT ( 'NONE',  ( -112.1069892527627019, -292.4682656310608877, -276.9071561157421115 ) ) ;
#29344 = CARTESIAN_POINT ( 'NONE',  ( -85.00586868677645214, -284.6704331258662251, -325.9626960450234492 ) ) ;
#29345 = CARTESIAN_POINT ( 'NONE',  ( 33.71106479835332692, -295.2337867547405494, -245.6775512770311707 ) ) ;
#29346 = DIRECTION ( 'NONE',  ( 0.000000000000000000, 0.000000000000000000, 1.000000000000000000 ) ) ;
#29347 = ADVANCED_FACE ( 'NONE', ( #32256 ), #82894, .T. ) ;
#29348 = FACE_OUTER_BOUND ( 'NONE', #52071, .T. ) ;
#29349 = CIRCLE ( 'NONE', #88320, 2.397123461337413719 ) ;
#29350 = CARTESIAN_POINT ( 'NONE',  ( 51.45114908912319862, -301.0756357822836549, -194.7723165178934721 ) ) ;
#29351 = CARTESIAN_POINT ( 'NONE',  ( -21.36288250136400535, -282.0392451996212912, -341.8084761257622404 ) ) ;
#29352 = CARTESIAN_POINT ( 'NONE',  ( -94.97486941952470829, -281.8891917100678484, -318.3550597851880752 ) ) ;
#29353 = CARTESIAN_POINT ( 'NONE',  ( -111.4390201347630978, -295.4939936698626184, -290.7018649857376431 ) ) ;
#29354 = CARTESIAN_POINT ( 'NONE',  ( 7.968710264204084126, -272.9210247110358409, -211.8381248859341781 ) ) ;
#29355 = CARTESIAN_POINT ( 'NONE',  ( -96.43069591213753711, -276.0073951301653779, -315.6358877594307160 ) ) ;
#29356 = CARTESIAN_POINT ( 'NONE',  ( -108.6575319309426533, -298.1006870904590755, -252.5529825906557733 ) ) ;
#29357 = AXIS2_PLACEMENT_3D ( 'NONE', #50185, #79082, #21793 ) ;
#29358 = CIRCLE ( 'NONE', #83732, 0.4999999999999989453 ) ;
#29359 = CARTESIAN_POINT ( 'NONE',  ( 33.69018346364105554, -295.2299990685132229, -289.6404662875638678 ) ) ;
#29360 = DIRECTION ( 'NONE',  ( -0.000000000000000000, -0.000000000000000000, -1.000000000000000000 ) ) ;
#29361 = CARTESIAN_POINT ( 'NONE',  ( -95.72702990780005905, -296.7367685734482166, -314.4697889355977622 ) ) ;
#29362 = DIRECTION ( 'NONE',  ( -0.000000000000000000, -1.000000000000000000, -0.000000000000000000 ) ) ;
#29364 = CARTESIAN_POINT ( 'NONE',  ( -92.19067496786476568, -295.8644903838483629, -318.5336200872338281 ) ) ;
#29363 = CARTESIAN_POINT ( 'NONE',  ( -86.65413264193442444, -283.3912579401395533, -213.3123178136127081 ) ) ;
#29365 = VECTOR ( 'NONE', #85336, 1000.000000000000000 ) ;
#29366 = CARTESIAN_POINT ( 'NONE',  ( -107.9261298496792847, -284.9459327910967090, -239.4570626986516402 ) ) ;
#29367 = CARTESIAN_POINT ( 'NONE',  ( 39.68124680641609814, -287.2338093497587010, -271.5551979139354444 ) ) ;
#29368 = CARTESIAN_POINT ( 'NONE',  ( -34.76937862477920049, -290.0843910736490443, -195.5720038592361618 ) ) ;
#29369 = CARTESIAN_POINT ( 'NONE',  ( -110.3929701802472891, -278.0515976507305140, -246.3664729343311990 ) ) ;
#29370 = CARTESIAN_POINT ( 'NONE',  ( -110.4542110544635705, -276.2666405000204009, -253.6410175316879361 ) ) ;
#29371 = DIRECTION ( 'NONE',  ( -0.000000000000000000, -0.000000000000000000, -1.000000000000000000 ) ) ;
#29372 = AXIS2_PLACEMENT_3D ( 'NONE', #36486, #22732, #36957 ) ;
#29373 = CARTESIAN_POINT ( 'NONE',  ( 34.08397165204494428, -286.5687793604742524, -287.2579791386397687 ) ) ;
#29374 = CARTESIAN_POINT ( 'NONE',  ( -111.3309290714171311, -289.7267738329644544, -250.1349356681278948 ) ) ;
#29375 = CARTESIAN_POINT ( 'NONE',  ( -86.44010706348282724, -280.8113878483986241, -211.7434181945305056 ) ) ;
#29377 = CARTESIAN_POINT ( 'NONE',  ( 35.37382106602651533, -281.1238157988054809, -263.1534771295596897 ) ) ;
#29376 = CARTESIAN_POINT ( 'NONE',  ( -110.7102911236716096, -294.3518889388678872, -287.6058608085305650 ) ) ;
#29378 = CARTESIAN_POINT ( 'NONE',  ( 32.23093163559096297, -294.1430603046895271, -303.4800983943899837 ) ) ;
#29379 = CARTESIAN_POINT ( 'NONE',  ( 4.404843850108581371, -284.6898753263513981, -207.3183114559111857 ) ) ;
#29380 = CARTESIAN_POINT ( 'NONE',  ( -111.0359012744987552, -280.7321098370366030, -256.3579892542754806 ) ) ;
#29381 = CARTESIAN_POINT ( 'NONE',  ( -105.1843630470213071, -295.2426135724037977, -297.9433864827450975 ) ) ;
#29382 = EDGE_LOOP ( 'NONE', ( #47639, #21150, #5210, #41236 ) ) ;
#29383 = DIRECTION ( 'NONE',  ( 0.000000000000000000, -1.000000000000000000, 0.000000000000000000 ) ) ;
#29384 = CARTESIAN_POINT ( 'NONE',  ( 13.04512740545966487, -284.3239562838868437, -325.4339280745186898 ) ) ;
#29385 = LINE ( 'NONE', #36474, #92748 ) ;
#29386 = CARTESIAN_POINT ( 'NONE',  ( -114.2704648735229114, -282.0523547857346784, -270.3284710469133074 ) ) ;
#29387 = CARTESIAN_POINT ( 'NONE',  ( -24.17719436905932895, -273.4131884429230581, -194.6046558516751190 ) ) ;
#29388 = EDGE_CURVE ( 'NONE', #54193, #19058, #75803, .T. ) ;
#29389 = CARTESIAN_POINT ( 'NONE',  ( -110.3370706542666824, -290.3746258537798326, -271.1832409830090569 ) ) ;
#29390 = CARTESIAN_POINT ( 'NONE',  ( 24.25147850832910379, -282.5154955652085391, -229.8094174413233759 ) ) ;
#29391 = CARTESIAN_POINT ( 'NONE',  ( 7.804399590131722242, -276.2807535519903013, -211.9807266404847894 ) ) ;
#29392 = CARTESIAN_POINT ( 'NONE',  ( 34.85771441707441909, -283.4642594479661852, -294.8908787054024287 ) ) ;
#29393 = CARTESIAN_POINT ( 'NONE',  ( 34.45682094086119918, -280.1464296584865679, -255.0662503580414864 ) ) ;
#29394 = CARTESIAN_POINT ( 'NONE',  ( -112.1554295852688341, -280.6201449716169805, -265.0784547196565768 ) ) ;
#29395 = CARTESIAN_POINT ( 'NONE',  ( -9.110314918286391617, -298.3964705767396595, -193.3611128246564306 ) ) ;
#29396 = CARTESIAN_POINT ( 'NONE',  ( -26.99441807673987626, -274.0134300104894578, -194.0060905329540901 ) ) ;
#29397 = CARTESIAN_POINT ( 'NONE',  ( 21.67960775317680699, -296.0985604750633229, -315.7449705802935682 ) ) ;
#29398 = CYLINDRICAL_SURFACE ( 'NONE', #82335, 4.999999999999990230 ) ;
#29399 = DIRECTION ( 'NONE',  ( 0.000000000000000000, 0.000000000000000000, 1.000000000000000000 ) ) ;
#29400 = CARTESIAN_POINT ( 'NONE',  ( 23.03015009568990834, -292.3115946483538323, -316.1382430998243080 ) ) ;
#29401 = CARTESIAN_POINT ( 'NONE',  ( -32.68084841259125284, -273.6200948604792984, -197.4358600290842389 ) ) ;
#29402 = AXIS2_PLACEMENT_3D ( 'NONE', #83456, #68342, #60779 ) ;
#29403 = CARTESIAN_POINT ( 'NONE',  ( -79.23013442843488008, -293.0184713644013641, -206.5165470158291612 ) ) ;
#29405 = CARTESIAN_POINT ( 'NONE',  ( 15.15482162060935245, -293.9782228119782417, -214.5018866470483658 ) ) ;
#29404 = CARTESIAN_POINT ( 'NONE',  ( -115.3430155898818299, -299.2662352645559167, -252.5904736702033517 ) ) ;
#29406 = CARTESIAN_POINT ( 'NONE',  ( 25.05179979218134534, -290.1118196252296570, -311.7013548735850463 ) ) ;
#29407 = CARTESIAN_POINT ( 'NONE',  ( -110.3909528865244170, -276.7617036368711751, -254.0595481132388329 ) ) ;
#29408 = AXIS2_PLACEMENT_3D ( 'NONE', #90791, #62914, #26438 ) ;
#29409 = CARTESIAN_POINT ( 'NONE',  ( -36.42437046259212963, -278.9607565800590123, -344.8081824879960777 ) ) ;
#29410 = CARTESIAN_POINT ( 'NONE',  ( 28.41893540962738740, -292.0993153451026387, -305.3546201167088157 ) ) ;
#29411 = CARTESIAN_POINT ( 'NONE',  ( 16.95783756074546389, -284.1494412613818099, -323.2742158642019490 ) ) ;
#29412 = ORIENTED_EDGE ( 'NONE', *, *, #11598, .F. ) ;
#29413 = CARTESIAN_POINT ( 'NONE',  ( -76.14195257550034057, -283.2526503301240837, -332.2806628266311009 ) ) ;
#29414 = CARTESIAN_POINT ( 'NONE',  ( -77.34306858593862444, -280.6090111245109711, -204.8673559265859865 ) ) ;
#29415 = CARTESIAN_POINT ( 'NONE',  ( -67.73797821593642254, -282.2372106319593286, -340.6752346150220774 ) ) ;
#29416 = CIRCLE ( 'NONE', #89879, 4.999999999999990230 ) ;
#29417 = CARTESIAN_POINT ( 'NONE',  ( -45.61231619327399756, -278.0956526534120599, -346.7318830156660852 ) ) ;
#29418 = CARTESIAN_POINT ( 'NONE',  ( 0.000000000000000000, 0.000000000000000000, 0.000000000000000000 ) ) ;
#29419 = CARTESIAN_POINT ( 'NONE',  ( -4.277598507016923790, -278.1443385272478395, -339.1466519217938753 ) ) ;
#29420 = CARTESIAN_POINT ( 'NONE',  ( -53.35057174420112602, -294.3376638359845288, -200.3683826091709648 ) ) ;
#29421 = ORIENTED_EDGE ( 'NONE', *, *, #70753, .T. ) ;
#29422 = CARTESIAN_POINT ( 'NONE',  ( -95.17157845193695209, -299.2114048752402482, -222.5843956695094050 ) ) ;
#29423 = CARTESIAN_POINT ( 'NONE',  ( -110.6635947713711658, -276.3908901595825682, -284.4197173372234602 ) ) ;
#29424 = CARTESIAN_POINT ( 'NONE',  ( -112.6647734145734461, -292.4441738851839432, -259.9546471555673293 ) ) ;
#29425 = CARTESIAN_POINT ( 'NONE',  ( 14.38254807697182791, -293.6500238913429257, -322.0897589086158064 ) ) ;
#29426 = CARTESIAN_POINT ( 'NONE',  ( 39.51652991492730393, -287.0030712347661392, -265.8282772508179050 ) ) ;
#29427 = DIRECTION ( 'NONE',  ( 0.3262578496237564796, 0.000000000000000000, 0.9452808130703185263 ) ) ;
#29429 = CARTESIAN_POINT ( 'NONE',  ( -99.71799481791592257, -282.4117782820048319, -309.8984088639176093 ) ) ;
#29428 = CARTESIAN_POINT ( 'NONE',  ( -34.89185439275038192, -293.5966742589454270, -346.7326084105980044 ) ) ;
#29430 = CARTESIAN_POINT ( 'NONE',  ( -56.35955021846258717, -291.1600894936623831, -342.1723946049600045 ) ) ;
#29431 = CARTESIAN_POINT ( 'NONE',  ( -69.05593939818318461, -284.1071736670024279, -203.8271667218678829 ) ) ;
#29432 = CARTESIAN_POINT ( 'NONE',  ( -15.97322681195358030, -284.0851011460346172, -340.6791940734782997 ) ) ;
#29433 = CARTESIAN_POINT ( 'NONE',  ( -23.34304231179140743, -289.8187538933159431, -345.8926001683159939 ) ) ;
#29434 = CARTESIAN_POINT ( 'NONE',  ( 0.4263973098515957960, -281.0621068020741404, -207.7600969120641707 ) ) ;
#29435 = CARTESIAN_POINT ( 'NONE',  ( -32.05531119196263035, -293.7818161457046813, -346.7946078279915696 ) ) ;
#29436 = AXIS2_PLACEMENT_3D ( 'NONE', #69100, #84217, #18910 ) ;
#29437 = CARTESIAN_POINT ( 'NONE',  ( 32.72183580609387832, -288.7587914706627998, -301.9088556574972131 ) ) ;
#29438 = CARTESIAN_POINT ( 'NONE',  ( 36.72687429895443501, -288.3061303840279948, -291.2270650345608374 ) ) ;
#29439 = CARTESIAN_POINT ( 'NONE',  ( -14.56801953567258856, -286.5222624954222397, -200.9513450132330377 ) ) ;
#29440 = EDGE_LOOP ( 'NONE', ( #63428, #20319, #43522, #20586 ) ) ;
#29441 = EDGE_CURVE ( 'NONE', #16112, #86133, #17094, .T. ) ;
#29442 = CARTESIAN_POINT ( 'NONE',  ( 196.1797262162750712, 26.01001517850438560, 13.20229404944032048 ) ) ;
#29444 = AXIS2_PLACEMENT_3D ( 'NONE', #7055, #12763, #86554 ) ;
#29443 = CARTESIAN_POINT ( 'NONE',  ( 14.64857673874188571, -296.1898147139193043, -325.4729732402030891 ) ) ;
#29445 = CARTESIAN_POINT ( 'NONE',  ( -96.14321264268662048, -294.5742223207029156, -319.3271825074128287 ) ) ;
#29446 = CARTESIAN_POINT ( 'NONE',  ( -95.79232511482905466, -278.2289813013987327, -226.2162438935023374 ) ) ;
#29447 = EDGE_CURVE ( 'NONE', #83522, #20445, #3847, .T. ) ;
#29448 = CARTESIAN_POINT ( 'NONE',  ( 76.20810742708401619, -298.7873891220818336, -193.4751467522457915 ) ) ;
#29449 = CARTESIAN_POINT ( 'NONE',  ( -0.4272579244908135676, -293.0321571942099013, -334.2004753444669518 ) ) ;
#29450 = CARTESIAN_POINT ( 'NONE',  ( 28.75633267816644789, -276.8664871371324807, -237.0591049793897582 ) ) ;
#29451 = CARTESIAN_POINT ( 'NONE',  ( -67.53861845606866154, -271.7913473142361909, -202.5311828194123223 ) ) ;
#29452 = CARTESIAN_POINT ( 'NONE',  ( 34.71711950422785975, -294.9402849152867248, -284.3130719310346990 ) ) ;
#29453 = CARTESIAN_POINT ( 'NONE',  ( 35.14573082668061232, -294.7799478305428238, -281.6369579766840729 ) ) ;
#29454 = CARTESIAN_POINT ( 'NONE',  ( -43.33278562674490075, -269.6489459241407758, -433.2630959494377976 ) ) ;
#29455 = CARTESIAN_POINT ( 'NONE',  ( -90.32477271515504924, -295.3043287394883691, -217.0429930663200366 ) ) ;
#29456 = CARTESIAN_POINT ( 'NONE',  ( -65.51240090560530405, -298.3448893561983937, -198.7519519267593466 ) ) ;
#29457 = DIRECTION ( 'NONE',  ( 0.000000000000000000, 0.000000000000000000, 1.000000000000000000 ) ) ;
#29458 = CARTESIAN_POINT ( 'NONE',  ( -48.08369117180302510, -290.1332854373709438, -342.8555095877779877 ) ) ;
#29459 = CARTESIAN_POINT ( 'NONE',  ( -18.21087668178067531, -295.1319818954327161, -340.8316726912700574 ) ) ;
#29460 = CARTESIAN_POINT ( 'NONE',  ( -90.15783077263444056, -279.7737683951879148, -324.1823107775127255 ) ) ;
#29461 = CARTESIAN_POINT ( 'NONE',  ( -61.87354465805472614, -278.4247818858306687, -197.8381067584539039 ) ) ;
#29462 = CARTESIAN_POINT ( 'NONE',  ( -70.43378196511422118, -282.8255107998761559, -339.7890100509052331 ) ) ;
#29463 = CARTESIAN_POINT ( 'NONE',  ( 21.77781754669398850, -274.2384729107440080, -221.1859675820693951 ) ) ;
#29464 = CARTESIAN_POINT ( 'NONE',  ( -98.73354046499858327, -282.0562806750648406, -312.5503565990406969 ) ) ;
#29465 = CARTESIAN_POINT ( 'NONE',  ( -86.27522419327856085, -277.7864740231936480, -211.8804546012555932 ) ) ;
#29466 = CARTESIAN_POINT ( 'NONE',  ( -39.50827033262464738, -278.0248805922515203, -195.2129372993834977 ) ) ;
#29467 = EDGE_CURVE ( 'NONE', #92884, #16098, #90908, .T. ) ;
#29468 = CARTESIAN_POINT ( 'NONE',  ( -52.72205844680755149, -296.5358998172821998, -198.4431201703008014 ) ) ;
#29469 = CARTESIAN_POINT ( 'NONE',  ( 8.542096661990747464, -278.4243122993293582, -329.7528266304913700 ) ) ;
#29470 = CARTESIAN_POINT ( 'NONE',  ( 195.3067512911517554, 24.77037501708018041, 13.15092252244243731 ) ) ;
#29471 = CARTESIAN_POINT ( 'NONE',  ( 16.33606428778431052, -290.8294433668969532, -217.3999566058536459 ) ) ;
#29472 = CARTESIAN_POINT ( 'NONE',  ( -91.59852996751116905, -289.7989041982640401, -325.0730742556975770 ) ) ;
#29473 = CARTESIAN_POINT ( 'NONE',  ( -0.9557631166994403626, -276.5341259932836806, -204.5734499503155064 ) ) ;
#29474 = CARTESIAN_POINT ( 'NONE',  ( -104.9985950553105312, -270.9780595309036926, -237.9953148188567127 ) ) ;
#29475 = CARTESIAN_POINT ( 'NONE',  ( -114.1937163747865753, -283.7183314760066537, -272.8338147801064224 ) ) ;
#29476 = CARTESIAN_POINT ( 'NONE',  ( 197.2116943569230330, 275.5000000000000568, -11.92446933126074882 ) ) ;
#29477 = CARTESIAN_POINT ( 'NONE',  ( -84.65766999013339955, -283.4005230564154090, -212.1038891505074560 ) ) ;
#29478 =( BOUNDED_SURFACE ( )  B_SPLINE_SURFACE ( 3, 2, ( 
 ( #79844, #14984, #86939 ),
 ( #36286, #309, #22091 ),
 ( #29189, #50961, #43840 ),
 ( #7405, #55374, #10855 ),
 ( #46371, #83761, #40189 ),
 ( #54416, #18433, #2838 ),
 ( #62001, #83287, #75731 ),
 ( #77141, #62482, #32659 ),
 ( #11337, #69108, #90380 ),
 ( #54882, #82371, #89449 ),
 ( #47290, #10390, #39255 ),
 ( #25997, #90836, #60611 ),
 ( #69568, #61547, #41115 ),
 ( #3774, #61086, #33573 ) ),
 .UNSPECIFIED., .F., .F., .F. ) 
 B_SPLINE_SURFACE_WITH_KNOTS ( ( 4, 2, 2, 2, 2, 2, 4 ),
 ( 3, 3 ),
 ( -2.168404344971008868E-19, 0.001236320232021350871, 0.001854480348032026523, 0.002472640464042702175, 0.003090800580053378044, 0.003708960696064053479, 0.004945280928085404350 ),
 ( 0.000000000000000000, 1.000000000000000000 ),
 .UNSPECIFIED. ) 
 GEOMETRIC_REPRESENTATION_ITEM ( )  RATIONAL_B_SPLINE_SURFACE ( (
 ( 1.000000000000000000, 0.8108476219622878789, 1.000000000000000000),
 ( 1.000000000000000000, 0.8255659973181316280, 1.000000000000000000),
 ( 1.000000000000000000, 0.8395011523844640999, 1.000000000000000000),
 ( 1.000000000000000000, 0.8588211550359595714, 1.000000000000000000),
 ( 1.000000000000000000, 0.8649348442247276614, 1.000000000000000000),
 ( 1.000000000000000000, 0.8760455507363352767, 1.000000000000000000),
 ( 1.000000000000000000, 0.8810998449843068236, 1.000000000000000000),
 ( 1.000000000000000000, 0.8900036393297112713, 1.000000000000000000),
 ( 1.000000000000000000, 0.8938622710284911399, 1.000000000000000000),
 ( 1.000000000000000000, 0.8997338558210890014, 1.000000000000000000),
 ( 1.000000000000000000, 0.9018082123496811153, 1.000000000000000000),
 ( 1.000000000000000000, 0.9050182246966690380, 1.000000000000000000),
 ( 1.000000000000000000, 0.9029724514273207436, 1.000000000000000000),
 ( 1.000000000000000000, 0.8966167345234181685, 1.000000000000000000) ) ) 
 REPRESENTATION_ITEM ( '' )  SURFACE ( )  );
#29479 = CARTESIAN_POINT ( 'NONE',  ( 209.4803090767392462, 35.69423656899339647, 14.26380412667038833 ) ) ;
#29480 = CARTESIAN_POINT ( 'NONE',  ( 36.10524484218158392, -292.3525312242224459, -270.7774077021125549 ) ) ;
#29481 = CARTESIAN_POINT ( 'NONE',  ( -100.6505410521979229, -283.2182040647455210, -231.4965382461817853 ) ) ;
#29482 = CARTESIAN_POINT ( 'NONE',  ( 204.6539576904058606, 300.0210572133868823, 3.999999999999991562 ) ) ;
#29483 = DIRECTION ( 'NONE',  ( 1.000000000000000000, 0.000000000000000000, 0.000000000000000000 ) ) ;
#29484 = CARTESIAN_POINT ( 'NONE',  ( 37.53304326110730216, -291.4857647407284844, -265.2035058653610236 ) ) ;
#29485 = CARTESIAN_POINT ( 'NONE',  ( -113.6326290101110743, -283.0728794613543187, -267.1243326976565413 ) ) ;
#29486 = CARTESIAN_POINT ( 'NONE',  ( -16.13166826601583637, -278.3735794856958705, -341.1011678043516895 ) ) ;
#29487 = CARTESIAN_POINT ( 'NONE',  ( -89.62649528327484916, -286.5398606072567418, -214.3040598409220081 ) ) ;
#29488 = CARTESIAN_POINT ( 'NONE',  ( -104.5975538124137358, -284.9346704430700470, -241.8472131398092699 ) ) ;
#29489 =( BOUNDED_CURVE ( )  B_SPLINE_CURVE ( 3, ( #69392, #19666, #48064, #76506 ),
 .UNSPECIFIED., .F., .F. ) 
 B_SPLINE_CURVE_WITH_KNOTS ( ( 4, 4 ),
 ( 5.759586531581287971, 6.283185307179586232 ),
 .UNSPECIFIED. ) 
 CURVE ( )  GEOMETRIC_REPRESENTATION_ITEM ( )  RATIONAL_B_SPLINE_CURVE ( ( 1.000000000000000000, 0.9772838841927120601, 0.9772838841927120601, 1.000000000000000000 ) ) 
 REPRESENTATION_ITEM ( '' )  );
#29490 = AXIS2_PLACEMENT_3D ( 'NONE', #31742, #75758, #33137 ) ;
#29491 = CARTESIAN_POINT ( 'NONE',  ( -37.79531972675044216, -278.4831812290463517, -343.9615045579537878 ) ) ;
#29492 = CARTESIAN_POINT ( 'NONE',  ( -99.61052880182131730, -279.8845740610955204, -231.8561862011571861 ) ) ;
#29493 = CARTESIAN_POINT ( 'NONE',  ( -96.03168533942694296, -287.1941086566839658, -223.6654405631720977 ) ) ;
#29494 = ORIENTED_EDGE ( 'NONE', *, *, #43350, .T. ) ;
#29495 = CARTESIAN_POINT ( 'NONE',  ( -34.85676911289912283, -294.8550630333614322, -347.3210109293037249 ) ) ;
#29496 = CARTESIAN_POINT ( 'NONE',  ( -66.95896003704004329, -291.4219878731375957, -338.9339645148407385 ) ) ;
#29497 = CARTESIAN_POINT ( 'NONE',  ( 196.8928068234201021, 24.78327594025822478, 12.47839767815188772 ) ) ;
#29498 = ADVANCED_BREP_SHAPE_REPRESENTATION ( '', ( #58100, #18940 ), #56754 ) ;
#29499 = AXIS2_PLACEMENT_3D ( 'NONE', #35349, #41959, #85055 ) ;
#29500 = CARTESIAN_POINT ( 'NONE',  ( -99.90806341382572953, -287.6948066931273047, -220.5068182859052968 ) ) ;
#29501 = CARTESIAN_POINT ( 'NONE',  ( 37.03484810655034210, -280.2375941489960383, -251.6629473883713501 ) ) ;
#29502 = CARTESIAN_POINT ( 'NONE',  ( 37.81383276167081675, -292.1119220558337020, -283.0132909945513688 ) ) ;
#29503 = CARTESIAN_POINT ( 'NONE',  ( 31.61659694450847624, -288.7270066686413088, -244.2275381038584499 ) ) ;
#29504 = CARTESIAN_POINT ( 'NONE',  ( -41.12509386878392803, -281.7640248183469680, -196.4445437477745031 ) ) ;
#29505 = CARTESIAN_POINT ( 'NONE',  ( 36.11965804806346370, -288.7096862772360168, -249.1487703829839120 ) ) ;
#29506 = CARTESIAN_POINT ( 'NONE',  ( -109.3039150921467666, -286.2796852836164021, -291.5360506709352535 ) ) ;
#29507 = CARTESIAN_POINT ( 'NONE',  ( -82.54456722724030726, -277.8176108042473516, -332.6965076942007613 ) ) ;
#29508 = ORIENTED_EDGE ( 'NONE', *, *, #61091, .F. ) ;
#29509 = CARTESIAN_POINT ( 'NONE',  ( -33.68671046397255964, -296.1182331951688411, -195.7175501496955690 ) ) ;
#29510 = CARTESIAN_POINT ( 'NONE',  ( 36.65675019654054267, -291.4364267330344660, -255.0154737681453696 ) ) ;
#29511 = CARTESIAN_POINT ( 'NONE',  ( -28.22289647405976964, -279.9980152433248577, -193.8493513623973570 ) ) ;
#29512 = CARTESIAN_POINT ( 'NONE',  ( -92.95903433394393289, -275.1033183609162052, -221.1922496042566877 ) ) ;
#29513 = DIRECTION ( 'NONE',  ( -1.000000000000000000, 0.000000000000000000, 0.000000000000000000 ) ) ;
#29514 = CLOSED_SHELL ( 'NONE', ( #63024, #58384, #8572, #25906, #86201, #90366, #64306, #71705, #86978, #28694, #11597, #3779, #45814, #65404, #57136, #24501, #56322, #67787, #21204, #57559, #74931, #33563 ) ) ;
#29515 = CARTESIAN_POINT ( 'NONE',  ( 21.31550574532285580, -284.6948066931273615, -317.0979686699210447 ) ) ;
#29516 = CARTESIAN_POINT ( 'NONE',  ( -32.72152071888341851, -272.3494587132752258, -194.5020598458118855 ) ) ;
#29517 = FACE_OUTER_BOUND ( 'NONE', #81114, .T. ) ;
#29518 = CARTESIAN_POINT ( 'NONE',  ( -108.6654609815782493, -278.2692726800484024, -254.4637435219671602 ) ) ;
#29519 = CARTESIAN_POINT ( 'NONE',  ( 25.74862499282144768, -277.3348026351846443, -313.8996969709345422 ) ) ;
#29520 = CARTESIAN_POINT ( 'NONE',  ( -44.64548351082566313, -299.3833389556023121, -197.0844480371542033 ) ) ;
#29521 = CARTESIAN_POINT ( 'NONE',  ( -112.2979457114078770, -283.4031087708121390, -286.9255818186777560 ) ) ;
#29522 = CARTESIAN_POINT ( 'NONE',  ( -96.56588323903820026, -291.6974498406003704, -314.7722385256952293 ) ) ;
#29523 = CARTESIAN_POINT ( 'NONE',  ( -40.43174374055428189, -299.5342198424431785, -194.0653840559467369 ) ) ;
#29524 = CARTESIAN_POINT ( 'NONE',  ( -33.37555111840804045, -299.3058391120957253, -193.7573961459067107 ) ) ;
#29525 = CARTESIAN_POINT ( 'NONE',  ( 22.81505689442831297, -296.1610629426511991, -314.8717123808947349 ) ) ;
#29526 = CARTESIAN_POINT ( 'NONE',  ( -100.5939507280918406, -282.0118106660077615, -310.4479420050581098 ) ) ;
#29527 = CARTESIAN_POINT ( 'NONE',  ( -68.95677777649038376, -271.6545389789197316, -202.7280798775381641 ) ) ;
#29528 = CARTESIAN_POINT ( 'NONE',  ( -0.1249202024432567587, -288.1388069382073809, -203.8529829890120482 ) ) ;
#29529 = CARTESIAN_POINT ( 'NONE',  ( 20.59331829107336986, -287.1026851902126396, -315.3009178560034798 ) ) ;
#29530 = CARTESIAN_POINT ( 'NONE',  ( -11.52259850706730937, -92.40725766065216362, -359.8631175693950581 ) ) ;
#29531 = ORIENTED_EDGE ( 'NONE', *, *, #72303, .F. ) ;
#29532 = CARTESIAN_POINT ( 'NONE',  ( -80.22505478101170695, -288.1948350395160787, -333.6676294675148711 ) ) ;
#29533 = CARTESIAN_POINT ( 'NONE',  ( -78.18975759646480128, -289.2847136255032297, -330.9490417433148082 ) ) ;
#29534 = ORIENTED_EDGE ( 'NONE', *, *, #77089, .F. ) ;
#29535 = CARTESIAN_POINT ( 'NONE',  ( -68.38827364194628444, -286.7334435362445788, -200.2211765921711049 ) ) ;
#29536 = CARTESIAN_POINT ( 'NONE',  ( -78.64046503454702020, -277.9584427451038664, -330.6431104899335764 ) ) ;
#29537 = ADVANCED_FACE ( 'NONE', ( #44894 ), #8911, .T. ) ;
#29538 = CARTESIAN_POINT ( 'NONE',  ( 24.57306022929602562, -291.8692496294517014, -225.1056767595034955 ) ) ;
#29539 = CARTESIAN_POINT ( 'NONE',  ( -90.36184359896449791, -284.4300827330563379, -326.1313139827984173 ) ) ;
#29540 = CARTESIAN_POINT ( 'NONE',  ( 27.72402831107037002, -283.5989735226227708, -310.3255460710678335 ) ) ;
#29541 = CARTESIAN_POINT ( 'NONE',  ( -58.47686732894896977, -283.6512811276439834, -344.4371987148072094 ) ) ;
#29542 = CARTESIAN_POINT ( 'NONE',  ( 9.286779929751507012, -281.0464595154438712, -214.1002583805804136 ) ) ;
#29543 = CARTESIAN_POINT ( 'NONE',  ( 5.883814447466332531, -58.44289898758961499, -354.8377425840699289 ) ) ;
#29544 = CARTESIAN_POINT ( 'NONE',  ( -99.14903296997707116, -279.9796998010316429, -312.5497661480141005 ) ) ;
#29545 = CARTESIAN_POINT ( 'NONE',  ( 196.0938070543772653, 285.1859344014769704, -111.4769352986099022 ) ) ;
#29546 = CARTESIAN_POINT ( 'NONE',  ( 63.78990005684839559, 47.06080592420466502, -315.5780313746797106 ) ) ;
#29547 = CARTESIAN_POINT ( 'NONE',  ( -16.58508189228268392, -273.5243249269602188, -200.1530018079023989 ) ) ;
#29548 = CARTESIAN_POINT ( 'NONE',  ( -66.90659241535628610, -294.9369876294423420, -341.4065981007842083 ) ) ;
#29549 = CARTESIAN_POINT ( 'NONE',  ( 189.5630867786578051, 267.9798697570337254, -137.6296589465633247 ) ) ;
#29550 = CARTESIAN_POINT ( 'NONE',  ( -100.7901325871747247, -271.8049220511685462, -227.5164554647896011 ) ) ;
#29551 = CARTESIAN_POINT ( 'NONE',  ( -111.6196797160949785, -298.3977315625589881, -271.5054065634899985 ) ) ;
#29552 = CARTESIAN_POINT ( 'NONE',  ( -42.68314824806152075, -290.4359842322951977, -343.7108522039593481 ) ) ;
#29553 = ORIENTED_EDGE ( 'NONE', *, *, #940, .F. ) ;
#29554 = CARTESIAN_POINT ( 'NONE',  ( -27.76526590967355190, -295.8747547571860537, -346.5792802118221516 ) ) ;
#29555 = CARTESIAN_POINT ( 'NONE',  ( -30.53178661845068476, -286.6327936377331298, -197.5667993515575631 ) ) ;
#29556 = CARTESIAN_POINT ( 'NONE',  ( -21.40555116452913609, -273.1722495103118149, -195.3442421139377245 ) ) ;
#29557 = CARTESIAN_POINT ( 'NONE',  ( 37.26270513387246552, -294.1243896541595291, -251.9670554436861494 ) ) ;
#29558 = CARTESIAN_POINT ( 'NONE',  ( -2.089625521674100650, -292.9985220296296689, -201.9590867474784659 ) ) ;
#29559 = CARTESIAN_POINT ( 'NONE',  ( -57.65697699456558212, -291.9492503865397453, -200.1919834250715553 ) ) ;
#29560 = ORIENTED_EDGE ( 'NONE', *, *, #75324, .T. ) ;
#29561 = CARTESIAN_POINT ( 'NONE',  ( -18.92507311505876544, -276.2074475718442272, -197.0258683489562088 ) ) ;
#29562 = CARTESIAN_POINT ( 'NONE',  ( 4.658348096915016612, -273.4001194884110078, -206.2356692151504376 ) ) ;
#29563 = ORIENTED_EDGE ( 'NONE', *, *, #14429, .T. ) ;
#29564 = ADVANCED_FACE ( 'NONE', ( #30709 ), #88909, .T. ) ;
#29565 = CARTESIAN_POINT ( 'NONE',  ( -97.88436887837400491, -277.4246251232415261, -317.8386091141192082 ) ) ;
#29566 = PRODUCT_DEFINITION_CONTEXT ( 'detailed design', #73513, 'design' ) ;
#29567 = CARTESIAN_POINT ( 'NONE',  ( 36.40021857569557540, -274.0044083474932677, -274.3762493418935833 ) ) ;
#29568 = CARTESIAN_POINT ( 'NONE',  ( -89.47160099107149733, -274.3757369873686116, -218.8179369648386228 ) ) ;
#29569 = CARTESIAN_POINT ( 'NONE',  ( 35.34113345345461710, -276.6167951493111445, -279.7446308801069108 ) ) ;
#29570 = CARTESIAN_POINT ( 'NONE',  ( -20.74755565520646527, -299.8567466513939053, -194.1566811824129957 ) ) ;
#29571 = CARTESIAN_POINT ( 'NONE',  ( 36.87662076604977557, -273.4046722380957135, -257.2470163978131836 ) ) ;
#29572 = CARTESIAN_POINT ( 'NONE',  ( -84.53759500551639405, -296.3734507739600303, -326.2526592484402386 ) ) ;
#29573 = CARTESIAN_POINT ( 'NONE',  ( 33.31084321856834407, -292.3974848506645685, -290.9877463449442416 ) ) ;
#29574 = LINE ( 'NONE', #64653, #60830 ) ;
#29575 = CARTESIAN_POINT ( 'NONE',  ( -5.304678688281513566, -277.1341018165870764, -340.3122163352838925 ) ) ;
#29576 = CARTESIAN_POINT ( 'NONE',  ( -0.5481045156054616951, -274.7224734834068158, -207.2970917509907167 ) ) ;
#29577 = VECTOR ( 'NONE', #43389, 1000.000000000000000 ) ;
#29578 = CARTESIAN_POINT ( 'NONE',  ( -113.8328822883666049, -283.2777944278572022, -267.1184951608079245 ) ) ;
#29579 = CARTESIAN_POINT ( 'NONE',  ( -73.69677811966252534, -297.5333320837584097, -336.2094960699198509 ) ) ;
#29580 = DIRECTION ( 'NONE',  ( -0.000000000000000000, -0.000000000000000000, 1.000000000000000000 ) ) ;
#29581 = CARTESIAN_POINT ( 'NONE',  ( -102.3772737991617277, -284.2038733483617534, -236.8502856486077519 ) ) ;
#29582 = EDGE_CURVE ( 'NONE', #57029, #85724, #15923, .T. ) ;
#29583 = CARTESIAN_POINT ( 'NONE',  ( -108.9473365334323347, -277.0364277085984099, -251.5868965467641942 ) ) ;
#29584 = CARTESIAN_POINT ( 'NONE',  ( -102.3861380289366707, -276.6618199710036947, -304.7790786095912949 ) ) ;
#29585 = CARTESIAN_POINT ( 'NONE',  ( -68.71584529783726225, -285.4646510790976777, -338.4973293159447962 ) ) ;
#29586 = CARTESIAN_POINT ( 'NONE',  ( 17.57248324751267887, -276.0644018987672439, -221.5871324460565290 ) ) ;
#29587 = DIRECTION ( 'NONE',  ( 0.000000000000000000, 0.000000000000000000, 1.000000000000000000 ) ) ;
#29588 = CARTESIAN_POINT ( 'NONE',  ( 38.82280831909432095, -273.9983404106151852, -274.0260221535552887 ) ) ;
#29589 = CARTESIAN_POINT ( 'NONE',  ( -64.11375111489769552, -281.7040289383692766, -200.0688658715786232 ) ) ;
#29590 = CARTESIAN_POINT ( 'NONE',  ( 151.4990408432631739, 130.0000000000000568, 12.49999999999999289 ) ) ;
#29591 = CARTESIAN_POINT ( 'NONE',  ( -40.77596817475892266, -287.9295556933017224, -194.8279836521215600 ) ) ;
#29592 = CARTESIAN_POINT ( 'NONE',  ( 154.7156223832750186, 19.57420759269872690, -12.98093464719507395 ) ) ;
#29593 = CARTESIAN_POINT ( 'NONE',  ( 37.40524269709768390, -291.6386379643914779, -277.1095863507511012 ) ) ;
#29594 = CARTESIAN_POINT ( 'NONE',  ( 144.2857639756989272, -299.5541904835127980, -201.5153591320744226 ) ) ;
#29595 = CARTESIAN_POINT ( 'NONE',  ( -83.48731640819566735, -272.0886817432012776, -213.1612440780648114 ) ) ;
#29596 = CARTESIAN_POINT ( 'NONE',  ( -99.31791905587400038, -289.2501573249719513, -229.4044334768249769 ) ) ;
#29597 = CARTESIAN_POINT ( 'NONE',  ( 143.8719904363247224, 176.7915900130879550, -240.1109971732525139 ) ) ;
#29598 = CARTESIAN_POINT ( 'NONE',  ( -72.58284060742491306, -295.5854839513073671, -204.1418306257749009 ) ) ;
#29599 = CARTESIAN_POINT ( 'NONE',  ( -113.1273492954476012, -288.9141755857889962, -279.7000315954782081 ) ) ;
#29600 = CARTESIAN_POINT ( 'NONE',  ( -42.97385589386844629, -284.7244129787180782, -343.9965295405752386 ) ) ;
#29601 = CARTESIAN_POINT ( 'NONE',  ( -37.95152406823138591, -284.2844759463075661, -194.3768950662571910 ) ) ;
#29602 = CARTESIAN_POINT ( 'NONE',  ( -87.31577472453834332, -285.1902734362008118, -324.4490244565558896 ) ) ;
#29603 = EDGE_CURVE ( 'NONE', #64179, #84307, #51819, .T. ) ;
#29604 = CARTESIAN_POINT ( 'NONE',  ( -73.86856342126864661, -284.3530359149967808, -333.8096173749000855 ) ) ;
#29605 = CARTESIAN_POINT ( 'NONE',  ( -79.59698675849078597, -291.5994511851951074, -332.8172295792726914 ) ) ;
#29606 = CARTESIAN_POINT ( 'NONE',  ( -70.12662235580337722, -273.9652705430538617, -200.6983546470103761 ) ) ;
#29607 = CARTESIAN_POINT ( 'NONE',  ( -51.44103206270705186, -287.3109468979891972, -344.5940152338362168 ) ) ;
#29608 = CARTESIAN_POINT ( 'NONE',  ( 26.06688202920612341, -276.1299213946431905, -314.1380885840816291 ) ) ;
#29609 = CARTESIAN_POINT ( 'NONE',  ( -17.76539404128532240, -296.7783278587023688, -342.3931597405695015 ) ) ;
#29610 = FACE_OUTER_BOUND ( 'NONE', #92635, .T. ) ;
#29611 = CARTESIAN_POINT ( 'NONE',  ( -54.42813229853333468, -291.7662352645558599, -345.3683826091709648 ) ) ;
#29612 = CARTESIAN_POINT ( 'NONE',  ( -70.45200056094631691, -282.1828846080255744, -335.9873214110297681 ) ) ;
#29613 = CARTESIAN_POINT ( 'NONE',  ( -81.49055733870788742, -275.6511190922333867, -331.1961969318503520 ) ) ;
#29614 = CARTESIAN_POINT ( 'NONE',  ( -112.8552825989664115, -271.1750533094028128, -259.0283548681853745 ) ) ;
#29615 = CARTESIAN_POINT ( 'NONE',  ( 27.95605332482075056, -274.4553207953253491, -237.4963030304643610 ) ) ;
#29616 = CARTESIAN_POINT ( 'NONE',  ( 23.90683462294566652, -294.5085036339241924, -229.3815530336137272 ) ) ;
#29617 = CARTESIAN_POINT ( 'NONE',  ( 33.53289891645359688, -294.2506797210995160, -251.9166158477855788 ) ) ;
#29618 = CARTESIAN_POINT ( 'NONE',  ( -102.6550473413429927, -285.8430338034438023, -305.2859476292934460 ) ) ;
#29619 = CARTESIAN_POINT ( 'NONE',  ( 6.145874232696984407, -294.0550847829957206, -207.5324846392213658 ) ) ;
#29620 = CARTESIAN_POINT ( 'NONE',  ( 12.94168331329148280, -294.0524942904685304, -212.6993488351442636 ) ) ;
#29621 = CARTESIAN_POINT ( 'NONE',  ( -98.73445341626768368, -295.8377693647446449, -309.9496714945110512 ) ) ;
#29622 = CARTESIAN_POINT ( 'NONE',  ( -110.8952903346242351, -292.3632559662616472, -285.0851424638776166 ) ) ;
#29623 = CARTESIAN_POINT ( 'NONE',  ( -13.41992111698593781, -282.9165543405028416, -343.5509293871369891 ) ) ;
#29624 = CARTESIAN_POINT ( 'NONE',  ( -69.58423332470269429, -271.7719288451023090, -201.7851074256025186 ) ) ;
#29625 = CARTESIAN_POINT ( 'NONE',  ( -33.72520494221807752, -285.9298046426694100, -193.4460936564299800 ) ) ;
#29626 = CARTESIAN_POINT ( 'NONE',  ( -93.95808570444467023, -279.8546664687211774, -319.0071012647097746 ) ) ;
#29627 = CARTESIAN_POINT ( 'NONE',  ( -60.08719069992943673, -284.5455757794537703, -200.5773579602496000 ) ) ;
#29628 = CARTESIAN_POINT ( 'NONE',  ( 37.70092827517243705, -285.5671982561229925, -271.5457951417682807 ) ) ;
#29629 = CARTESIAN_POINT ( 'NONE',  ( -73.16043522044930114, -277.7221382641683363, -203.5832180051226032 ) ) ;
#29630 = CARTESIAN_POINT ( 'NONE',  ( -75.31871349344845612, -193.4224457575235192, -358.3059354159982490 ) ) ;
#29631 = CARTESIAN_POINT ( 'NONE',  ( -108.9880835656874751, -284.2484207508248346, -256.0508355904121913 ) ) ;
#29632 = CARTESIAN_POINT ( 'NONE',  ( 18.85836328065643386, -282.0444514180719011, -218.3076686106557247 ) ) ;
#29633 = CARTESIAN_POINT ( 'NONE',  ( -7.023918916874150931, -287.7227311347126033, -340.8994394802101056 ) ) ;
#29634 = CARTESIAN_POINT ( 'NONE',  ( -17.54588820591202136, -278.4010216360529171, -343.9448542552958656 ) ) ;
#29635 = CARTESIAN_POINT ( 'NONE',  ( -42.75445766322408758, -278.4342814747827788, -346.6762562500495051 ) ) ;
#29636 = CARTESIAN_POINT ( 'NONE',  ( -91.29538787645398656, -279.0905971059065109, -221.1879588114905175 ) ) ;
#29637 = CARTESIAN_POINT ( 'NONE',  ( -2.160214114160412091, -276.5002122664850503, -204.5271613436518123 ) ) ;
#29638 = CARTESIAN_POINT ( 'NONE',  ( 21.31044597694716813, -292.8793304468553629, -220.4518400622679053 ) ) ;
#29639 = CARTESIAN_POINT ( 'NONE',  ( 11.16540628403935465, -286.3970434720236540, -327.1648582220523735 ) ) ;
#29640 = TOROIDAL_SURFACE ( 'NONE', #13029, 204.0731808058633590, 35.00000000000000000 ) ;
#29641 = CARTESIAN_POINT ( 'NONE',  ( -3.693172007110046007, -294.0888342864424772, -201.9784882843183595 ) ) ;
#29642 = CARTESIAN_POINT ( 'NONE',  ( 28.66692138427277214, -292.9036584168970307, -302.3699572380102722 ) ) ;
#29643 = CARTESIAN_POINT ( 'NONE',  ( -5.536134208376211951, -294.2885853628543487, -336.1053927999683424 ) ) ;
#29644 = CARTESIAN_POINT ( 'NONE',  ( -79.43628431113995703, -292.5780917485774353, -206.1919484113753924 ) ) ;
#29645 = CARTESIAN_POINT ( 'NONE',  ( 35.45303499439760486, -282.1083515570405780, -263.1330287051370078 ) ) ;
#29646 = ADVANCED_FACE ( 'NONE', ( #9373 ), #73797, .T. ) ;
#29647 = CARTESIAN_POINT ( 'NONE',  ( -108.9427853834417022, -271.9642400710333163, -242.5362613821383775 ) ) ;
#29648 = CARTESIAN_POINT ( 'NONE',  ( -28.98000735492000857, -289.6003541596352875, -346.8566749568366276 ) ) ;
#29649 = CARTESIAN_POINT ( 'NONE',  ( -66.12922475595220817, -281.5644939876680724, -340.4577718518989968 ) ) ;
#29650 = CARTESIAN_POINT ( 'NONE',  ( -31.82405520611115435, -289.3177330542793015, -347.1945156574853968 ) ) ;
#29651 = CARTESIAN_POINT ( 'NONE',  ( -85.74333724841939386, -285.6936461556302902, -215.6184101304806688 ) ) ;
#29652 = CARTESIAN_POINT ( 'NONE',  ( 102.7371733172544026, 116.6117108518458849, -282.8160689236807457 ) ) ;
#29653 = CARTESIAN_POINT ( 'NONE',  ( 43.56306698794277565, 12.70319086556685129, -330.1861164527855408 ) ) ;
#29654 = CARTESIAN_POINT ( 'NONE',  ( -105.6623585921115733, -259.9751593823307871, -315.4586869756183773 ) ) ;
#29655 = CARTESIAN_POINT ( 'NONE',  ( -108.7621599872536819, -277.9588375987510176, -254.4381302097820026 ) ) ;
#29656 = CARTESIAN_POINT ( 'NONE',  ( 13.55958273807232572, -279.7054289642043727, -217.5335106749859619 ) ) ;
#29657 = CARTESIAN_POINT ( 'NONE',  ( -13.06513110315417947, -274.0258880468310849, -197.3105020519171546 ) ) ;
#29658 = CARTESIAN_POINT ( 'NONE',  ( 104.6247447840909359, 114.2303491467357190, -280.5431434108185726 ) ) ;
#29659 = CARTESIAN_POINT ( 'NONE',  ( -109.9838096901949456, -277.4292583091490769, -246.4924618822047648 ) ) ;
#29660 = CARTESIAN_POINT ( 'NONE',  ( -101.8346370661179066, -282.0678389936044255, -307.9444638383147890 ) ) ;
#29661 = CARTESIAN_POINT ( 'NONE',  ( -47.47397414952396133, -296.9393943911057931, -345.6692253503870234 ) ) ;
#29662 = CARTESIAN_POINT ( 'NONE',  ( -36.21146232590110969, -292.5590134654867143, -197.2958349120321202 ) ) ;
#29663 = CARTESIAN_POINT ( 'NONE',  ( -26.41801957244197396, -287.5951950692532364, -343.0893071873571785 ) ) ;
#29664 = CARTESIAN_POINT ( 'NONE',  ( 53.49099207302668191, -299.6531962426988684, -193.4152503488299715 ) ) ;
#29665 = CARTESIAN_POINT ( 'NONE',  ( -96.88396652854682145, -297.3085692605815211, -228.1270261086731637 ) ) ;
#29666 = ORIENTED_EDGE ( 'NONE', *, *, #50363, .T. ) ;
#29667 = DIRECTION ( 'NONE',  ( -0.000000000000000000, 1.000000000000000000, -0.000000000000000000 ) ) ;
#29668 = CARTESIAN_POINT ( 'NONE',  ( -111.0034862210051898, -280.6867964607517365, -253.5309227219060801 ) ) ;
#29669 = CARTESIAN_POINT ( 'NONE',  ( -11.64763532457017980, -281.4743203664924636, -201.6485640219812012 ) ) ;
#29670 = CARTESIAN_POINT ( 'NONE',  ( -99.62193874892432177, -279.7291091066461490, -313.8943913686511564 ) ) ;
#29671 = CARTESIAN_POINT ( 'NONE',  ( 27.05627497650192836, -281.0852336521578536, -305.2367434235862333 ) ) ;
#29672 = CARTESIAN_POINT ( 'NONE',  ( 5.596289705310259599, -273.1250789456464645, -210.4061601779694115 ) ) ;
#29673 = CARTESIAN_POINT ( 'NONE',  ( 207.9416365392708883, 29.59756043702767769, 14.84194439653736630 ) ) ;
#29674 = CARTESIAN_POINT ( 'NONE',  ( 154.4601611254704494, 20.78894139178057543, 13.92477262272432625 ) ) ;
#29675 = CARTESIAN_POINT ( 'NONE',  ( 25.18952843175291889, -275.7619677009976726, -225.6843382456580684 ) ) ;
#29676 = EDGE_LOOP ( 'NONE', ( #16566, #92275, #43042, #40209 ) ) ;
#29677 = CARTESIAN_POINT ( 'NONE',  ( 25.24712700583817337, -276.9943808510390113, -229.0375246421661757 ) ) ;
#29678 = CARTESIAN_POINT ( 'NONE',  ( -111.9133656767005505, -276.9168792142654638, -287.0246408058439442 ) ) ;
#29679 = ORIENTED_EDGE ( 'NONE', *, *, #60782, .F. ) ;
#29680 = CARTESIAN_POINT ( 'NONE',  ( 199.1510190623362462, 40.29428703769173126, 9.290748352207996774 ) ) ;
#29681 = CARTESIAN_POINT ( 'NONE',  ( 35.01319601417345240, -283.2617440155767099, -249.2631720134422153 ) ) ;
#29682 = CARTESIAN_POINT ( 'NONE',  ( -60.29995964451961044, -290.9440341732312731, -200.8420003874190627 ) ) ;
#29683 = CARTESIAN_POINT ( 'NONE',  ( -3.526687819948334912, -285.8353794678967006, -201.2824517417850245 ) ) ;
#29684 = CARTESIAN_POINT ( 'NONE',  ( -43.03289678459244527, -281.3646855581001773, -344.2061018596274380 ) ) ;
#29686 = CARTESIAN_POINT ( 'NONE',  ( 16.07959904350122216, -284.8970256550888394, -218.5202172164138119 ) ) ;
#29685 = CARTESIAN_POINT ( 'NONE',  ( -51.14608356377940623, -281.8066404029955265, -342.6959869423694727 ) ) ;
#29687 = CARTESIAN_POINT ( 'NONE',  ( -57.23549509702517923, -280.9947449096526952, -199.7115077534392356 ) ) ;
#29688 = CARTESIAN_POINT ( 'NONE',  ( -75.39540825008494096, -271.5449969383657844, -205.6720558086690573 ) ) ;
#29689 = CARTESIAN_POINT ( 'NONE',  ( -95.19567575923966274, -283.6289367563189217, -220.6900871061976090 ) ) ;
#29690 = CARTESIAN_POINT ( 'NONE',  ( -39.03643339669644519, -297.0735797004466576, -345.3419724147339025 ) ) ;
#29691 = CARTESIAN_POINT ( 'NONE',  ( -62.40068736496046853, -280.6593845261911042, -201.4929380460660582 ) ) ;
#29692 = CARTESIAN_POINT ( 'NONE',  ( -31.06299756793917766, -288.1314472803235844, -195.4441591420193447 ) ) ;
#29693 = FACE_OUTER_BOUND ( 'NONE', #32910, .T. ) ;
#29694 = CARTESIAN_POINT ( 'NONE',  ( 208.8914842347286367, 1.063508326896293932, -7.500000000000007105 ) ) ;
#29695 = CARTESIAN_POINT ( 'NONE',  ( 20.19769092011089739, -294.7991740664695612, -221.3665428511745858 ) ) ;
#29696 = CARTESIAN_POINT ( 'NONE',  ( -86.43307149172063930, -275.7331791087937063, -327.1312379804949160 ) ) ;
#29697 = EDGE_CURVE ( 'NONE', #51603, #63777, #91133, .T. ) ;
#29698 = CARTESIAN_POINT ( 'NONE',  ( 24.00710202841647600, -287.3667044554251788, -316.6264753786940673 ) ) ;
#29699 = CARTESIAN_POINT ( 'NONE',  ( 11.47508901242241919, -291.1420479501269938, -214.9452667130525469 ) ) ;
#29700 = CARTESIAN_POINT ( 'NONE',  ( -73.09647887856914394, -276.2214312034078603, -334.5849379539266124 ) ) ;
#29701 = CARTESIAN_POINT ( 'NONE',  ( -94.55055087073878894, -295.3514543126955800, -223.0337089603132483 ) ) ;
#29702 = CARTESIAN_POINT ( 'NONE',  ( -33.49928954266992065, -293.4166720004045601, -196.9559029614337078 ) ) ;
#29703 = CARTESIAN_POINT ( 'NONE',  ( -37.37352853689063892, -282.5519495502701943, -195.3611179825600175 ) ) ;
#29704 = CARTESIAN_POINT ( 'NONE',  ( 0.000000000000000000, 0.000000000000000000, 7.500000000000000000 ) ) ;
#29705 = CARTESIAN_POINT ( 'NONE',  ( -53.16455317388895452, -293.7312148252159432, -345.0633148318088388 ) ) ;
#29706 = CARTESIAN_POINT ( 'NONE',  ( 36.06810186874872670, -289.0533909609868033, -262.7821084795058937 ) ) ;
#29707 = CARTESIAN_POINT ( 'NONE',  ( -99.06048478801183421, -288.1964447471899007, -314.7090962722040786 ) ) ;
#29708 = CARTESIAN_POINT ( 'NONE',  ( 20.83436606291492055, -289.6072228468266303, -315.4472600817837815 ) ) ;
#29709 = EDGE_CURVE ( 'NONE', #90266, #82861, #59065, .T. ) ;
#29710 = DIRECTION ( 'NONE',  ( 0.000000000000000000, 1.000000000000000000, 0.000000000000000000 ) ) ;
#29711 = CARTESIAN_POINT ( 'NONE',  ( -37.25759145717675835, -289.8539069934169561, -343.5225467091082692 ) ) ;
#29712 = CARTESIAN_POINT ( 'NONE',  ( -47.80257052418233599, -229.5268262511776527, -22.50000000000000000 ) ) ;
#29713 = CARTESIAN_POINT ( 'NONE',  ( 21.19556808880022913, -289.4263085862942830, -319.7716123078234318 ) ) ;
#29714 = CARTESIAN_POINT ( 'NONE',  ( -96.39193230797211243, -277.2124155529683094, -223.5479052408409473 ) ) ;
#29715 = CARTESIAN_POINT ( 'NONE',  ( -107.4016407626999410, -279.2946764044959309, -238.3368548032771059 ) ) ;
#29716 = CARTESIAN_POINT ( 'NONE',  ( 9.192648859285828422, -282.0991723277315373, -331.6823920704227930 ) ) ;
#29717 = CARTESIAN_POINT ( 'NONE',  ( 37.62803344409771000, -285.5971482527808689, -273.8783461424195593 ) ) ;
#29718 = CARTESIAN_POINT ( 'NONE',  ( 208.8121973762197854, 29.40831337191700712, 14.72017627883221813 ) ) ;
#29719 = CARTESIAN_POINT ( 'NONE',  ( -93.12115690444468896, -277.3795053782364448, -221.3569160722253457 ) ) ;
#29720 = CARTESIAN_POINT ( 'NONE',  ( -38.72196233910162277, -281.0693086123899889, -345.3484204329287763 ) ) ;
#29721 = CARTESIAN_POINT ( 'NONE',  ( 188.2019740231993410, 44.81720372851549428, 15.00000000000000000 ) ) ;
#29722 = CARTESIAN_POINT ( 'NONE',  ( -90.85672083596389825, -276.2743181753925228, -324.8304469205484111 ) ) ;
#29723 = CARTESIAN_POINT ( 'NONE',  ( -96.94090207010110305, -282.8223639851920552, -318.6459036166726264 ) ) ;
#29724 = CARTESIAN_POINT ( 'NONE',  ( -107.3540425892165189, -273.6375896358426303, -248.9537119329646941 ) ) ;
#29725 = CARTESIAN_POINT ( 'NONE',  ( -108.5288931497206590, -292.4066420526079355, -250.8977172977807015 ) ) ;
#29726 = CARTESIAN_POINT ( 'NONE',  ( -31.96955077377693044, -299.4332532737373640, -193.8530929171411685 ) ) ;
#29727 = CARTESIAN_POINT ( 'NONE',  ( 35.62283468078590687, -275.2710516445213784, -274.3180060180289388 ) ) ;
#29728 = CARTESIAN_POINT ( 'NONE',  ( -97.18517654658869276, -297.9339028520907959, -315.5902180864870843 ) ) ;
#29729 = CARTESIAN_POINT ( 'NONE',  ( 14.60527427079775897, -288.5118035591880243, -327.2709647863877649 ) ) ;
#29730 = CARTESIAN_POINT ( 'NONE',  ( 16.21993980794121271, -278.8844712294798569, -216.9917134188006855 ) ) ;
#29731 = CARTESIAN_POINT ( 'NONE',  ( -61.68656851459968493, -291.5778041804223335, -197.2547913010251364 ) ) ;
#29732 = CARTESIAN_POINT ( 'NONE',  ( -50.80644922200760050, -288.2870082993838992, -342.3998316710440690 ) ) ;
#29733 = CARTESIAN_POINT ( 'NONE',  ( -11.76386655225271305, -292.7191181844610242, -340.9199342683379541 ) ) ;
#29734 = ORIENTED_EDGE ( 'NONE', *, *, #79978, .F. ) ;
#29735 = CARTESIAN_POINT ( 'NONE',  ( 222.8344101925596306, 0.000000000000000000, -7.000000000000000888 ) ) ;
#29736 = CARTESIAN_POINT ( 'NONE',  ( -95.00300048304677603, -289.4279681657196761, -315.2496168284164355 ) ) ;
#29737 = CARTESIAN_POINT ( 'NONE',  ( 175.2296996224750103, 247.0000000000001137, 0.000000000000000000 ) ) ;
#29738 = CARTESIAN_POINT ( 'NONE',  ( -18.25216422122220905, -287.2334494808496856, -195.9529088622287816 ) ) ;
#29739 = CARTESIAN_POINT ( 'NONE',  ( 30.89617123739170168, -289.8376638359844719, -254.7536222014695397 ) ) ;
#29740 = CARTESIAN_POINT ( 'NONE',  ( 4.090187254265777561, -293.5676309641667103, -335.0473681626875759 ) ) ;
#29741 = CARTESIAN_POINT ( 'NONE',  ( -3.098444572333995062, -283.9245090316514961, -338.7913035223452312 ) ) ;
#29742 = CARTESIAN_POINT ( 'NONE',  ( -108.6644501535277669, -284.5914832033960806, -254.7443171341209904 ) ) ;
#29743 = CARTESIAN_POINT ( 'NONE',  ( 32.57244656632658319, -277.1658799861546640, -293.0162624318310804 ) ) ;
#29744 = CARTESIAN_POINT ( 'NONE',  ( 18.28995487035879108, -292.2687581093666154, -320.1495058370633160 ) ) ;
#29745 = CARTESIAN_POINT ( 'NONE',  ( 34.22434477708029732, -274.1326527220981006, -254.0127974215033930 ) ) ;
#29746 = ORIENTED_EDGE ( 'NONE', *, *, #22620, .T. ) ;
#29747 = CARTESIAN_POINT ( 'NONE',  ( 201.7194887906492795, 294.2213704821156739, -83.28174295417332473 ) ) ;
#29748 = CARTESIAN_POINT ( 'NONE',  ( -4.515403015387063235, -294.2980979854356747, -340.0044460302239031 ) ) ;
#29749 = CARTESIAN_POINT ( 'NONE',  ( 27.61216122733912570, -288.9832629575090550, -233.8921314275067971 ) ) ;
#29750 = CARTESIAN_POINT ( 'NONE',  ( -112.8372558150556273, -297.8011794446631484, -256.8735836710407057 ) ) ;
#29751 = CARTESIAN_POINT ( 'NONE',  ( 32.76537310381092993, -287.9293844090824450, -249.6072950097953367 ) ) ;
#29752 = CARTESIAN_POINT ( 'NONE',  ( -67.62684590583617705, -276.4986784579949699, -340.8992648155894472 ) ) ;
#29753 = CARTESIAN_POINT ( 'NONE',  ( 23.95275577669692524, -294.8230175471387611, -316.7971219267862466 ) ) ;
#29754 = CARTESIAN_POINT ( 'NONE',  ( 4.849513116717326433, -286.6283170989492532, -333.2912936024492865 ) ) ;
#29755 = CARTESIAN_POINT ( 'NONE',  ( -27.74626068950224322, -295.2668818956235555, -346.7928735307040711 ) ) ;
#29756 = CARTESIAN_POINT ( 'NONE',  ( -94.31006874709630949, -291.5310353280050890, -224.6609182701506597 ) ) ;
#29757 = DIRECTION ( 'NONE',  ( 0.000000000000000000, 1.000000000000000000, 0.000000000000000000 ) ) ;
#29758 = CYLINDRICAL_SURFACE ( 'NONE', #81041, 8.000000000000000000 ) ;
#29759 = CARTESIAN_POINT ( 'NONE',  ( -62.10227321113477927, -183.1506894772463170, -358.8537685376831519 ) ) ;
#29760 = CARTESIAN_POINT ( 'NONE',  ( 1.155022920908411965, -288.0764393216227859, -204.4618544009913137 ) ) ;
#29761 = CARTESIAN_POINT ( 'NONE',  ( -119.3990491898856732, -282.0523547857346784, -270.3284710469131937 ) ) ;
#29762 = ORIENTED_EDGE ( 'NONE', *, *, #26156, .T. ) ;
#29763 = EDGE_CURVE ( 'NONE', #46033, #41118, #65521, .T. ) ;
#29764 = CARTESIAN_POINT ( 'NONE',  ( -92.99424422427587444, -278.6279363653633254, -217.2180408081439396 ) ) ;
#29765 = CARTESIAN_POINT ( 'NONE',  ( 32.04369037306253887, -283.9184661579258204, -298.3913874970971278 ) ) ;
#29766 = CARTESIAN_POINT ( 'NONE',  ( -37.67646286175954629, -140.7588499655415717, -363.8534987691544984 ) ) ;
#29767 = EDGE_CURVE ( 'NONE', #40624, #8082, #23605, .T. ) ;
#29768 = CARTESIAN_POINT ( 'NONE',  ( -97.59110767480697746, -282.4941414840032508, -317.3570240334217942 ) ) ;
#29769 = CARTESIAN_POINT ( 'NONE',  ( -2.717962632440341864, -286.6708970228537510, -336.3159260395974002 ) ) ;
#29770 = CARTESIAN_POINT ( 'NONE',  ( 1.759910812504751787, -276.4297121997193472, -205.4660526705447978 ) ) ;
#29771 = CARTESIAN_POINT ( 'NONE',  ( -108.5384183649809415, -297.2606848406528570, -253.9594182480530264 ) ) ;
#29772 = CARTESIAN_POINT ( 'NONE',  ( -66.26252143338784606, -294.1237160610095316, -337.9246404924402896 ) ) ;
#29773 = CARTESIAN_POINT ( 'NONE',  ( -79.86133719354405969, -280.1451829868925643, -206.2238955369903977 ) ) ;
#29775 = CARTESIAN_POINT ( 'NONE',  ( -89.54056185941973922, -278.6412010428995245, -219.1115467767951372 ) ) ;
#29774 = CARTESIAN_POINT ( 'NONE',  ( -35.11763588454444829, -277.0234491840425335, -343.3272302418863546 ) ) ;
#29776 = CARTESIAN_POINT ( 'NONE',  ( -63.46477523918077424, -274.7992083076206882, -198.2564894473110826 ) ) ;
#29777 = CARTESIAN_POINT ( 'NONE',  ( 10.32314135161459312, -275.3325809395210513, -330.5084956586987914 ) ) ;
#29778 = CARTESIAN_POINT ( 'NONE',  ( 179.6752721477509169, 254.2973581423329961, -166.6431896920282156 ) ) ;
#29779 = CARTESIAN_POINT ( 'NONE',  ( -10.71106274343912368, -274.7048202316581182, -340.5280600799721924 ) ) ;
#29780 = CARTESIAN_POINT ( 'NONE',  ( -110.6449482852799946, -297.7042436808759476, -291.9766556290427388 ) ) ;
#29781 = DIRECTION ( 'NONE',  ( 0.000000000000000000, 1.000000000000000000, 0.000000000000000000 ) ) ;
#29782 = CARTESIAN_POINT ( 'NONE',  ( -101.2450674239233592, -254.4445186991787295, -323.9438275447045612 ) ) ;
#29783 = CARTESIAN_POINT ( 'NONE',  ( -97.61790235991986719, -286.2109432409814076, -228.6135647561198994 ) ) ;
#29784 = CARTESIAN_POINT ( 'NONE',  ( -112.5925965042998769, -286.1739043468507475, -281.2807622910634677 ) ) ;
#29785 = CARTESIAN_POINT ( 'NONE',  ( -44.02544850248704478, -285.3139989042971933, -197.5653751410347070 ) ) ;
#29786 = CARTESIAN_POINT ( 'NONE',  ( -93.68795063020233727, -277.6222391076884719, -222.6810054055959824 ) ) ;
#29787 = CARTESIAN_POINT ( 'NONE',  ( -93.47790634488630701, -285.7317266225302888, -318.9560847290463812 ) ) ;
#29788 = CARTESIAN_POINT ( 'NONE',  ( -95.32449036965496703, -277.6675213438728065, -224.8578092472863830 ) ) ;
#29789 = CARTESIAN_POINT ( 'NONE',  ( -74.15666704628830530, -278.6335669687546783, -333.7557887727306252 ) ) ;
#29790 = CARTESIAN_POINT ( 'NONE',  ( 24.03949023665031604, -276.5937399026541925, -310.0819035771052654 ) ) ;
#29791 = CARTESIAN_POINT ( 'NONE',  ( 6.084558092747128555, -281.4280190228291758, -206.9709064587487717 ) ) ;
#29792 = CARTESIAN_POINT ( 'NONE',  ( -18.92704234247923978, -283.3137170489985692, -345.1182903697914526 ) ) ;
#29793 = ORIENTED_EDGE ( 'NONE', *, *, #91737, .T. ) ;
#29794 = VERTEX_POINT ( 'NONE', #38726 ) ;
#29795 = CARTESIAN_POINT ( 'NONE',  ( 196.0143093133015952, 19.33012701892214480, -12.49999999999990941 ) ) ;
#29796 = CARTESIAN_POINT ( 'NONE',  ( 23.17020799508900808, -290.0295222843496390, -315.9529424533939164 ) ) ;
#29797 = CARTESIAN_POINT ( 'NONE',  ( -113.7595386947123188, -289.1905403695295149, -274.0505922470043174 ) ) ;
#29798 = CARTESIAN_POINT ( 'NONE',  ( -91.95864403717160940, -296.4438922646780270, -221.6826713633446957 ) ) ;
#29799 = CARTESIAN_POINT ( 'NONE',  ( -58.90214686079597328, -291.1289142516320680, -196.5474341360076096 ) ) ;
#29800 = CARTESIAN_POINT ( 'NONE',  ( 36.34830397062242469, -286.0411795505942791, -271.0618650333080382 ) ) ;
#29801 = ADVANCED_FACE ( 'NONE', ( #67632 ), #88066, .T. ) ;
#29802 = CARTESIAN_POINT ( 'NONE',  ( 31.77846675940804744, -289.0841707938824356, -295.0498407896378126 ) ) ;
#29803 = CARTESIAN_POINT ( 'NONE',  ( -85.33152481854864391, -293.9090924074130839, -210.2361428286349110 ) ) ;
#29804 = CARTESIAN_POINT ( 'NONE',  ( -3.928262803169098039, -290.6116789329420271, -337.5210523720245988 ) ) ;
#29805 = CARTESIAN_POINT ( 'NONE',  ( -2.669583632924863892, -286.5945727649223613, -337.0534921139679341 ) ) ;
#29806 = CARTESIAN_POINT ( 'NONE',  ( -76.24198274950093435, -284.5269780908135999, -332.4708768190238288 ) ) ;
#29807 = CARTESIAN_POINT ( 'NONE',  ( -111.5460350991995568, -292.3987112919415949, -282.3504924057641006 ) ) ;
#29808 = CARTESIAN_POINT ( 'NONE',  ( 82.17145489947652948, -297.7796885176689443, -194.3909460517409400 ) ) ;
#29809 = CARTESIAN_POINT ( 'NONE',  ( -35.09237171215954021, -122.5496321078137356, 22.50000000000000000 ) ) ;
#29810 = CARTESIAN_POINT ( 'NONE',  ( -110.8446223043016090, -274.7442409379967216, -253.7560814164667704 ) ) ;
#29811 = CARTESIAN_POINT ( 'NONE',  ( 5.678810554957125944, -281.6493811923922976, -329.5374425309335606 ) ) ;
#29812 = CARTESIAN_POINT ( 'NONE',  ( -107.0828554234159782, -282.1911459966474354, -298.0919542509653297 ) ) ;
#29813 = CARTESIAN_POINT ( 'NONE',  ( 37.62412235618065637, -292.9613778286965839, -287.2812034886450760 ) ) ;
#29814 = CARTESIAN_POINT ( 'NONE',  ( -105.3013900511996894, -271.1821081635329733, -240.9148730300615000 ) ) ;
#29815 = CARTESIAN_POINT ( 'NONE',  ( 33.88729742345162776, -273.9133530706120041, -292.0326489164241366 ) ) ;
#29816 = CARTESIAN_POINT ( 'NONE',  ( -110.8680053135456518, -297.8885935144015775, -268.7386087679097955 ) ) ;
#29817 = CARTESIAN_POINT ( 'NONE',  ( 191.4749582765727212, 14.19731191252289015, 13.00000000000000178 ) ) ;
#29818 = CARTESIAN_POINT ( 'NONE',  ( -92.96320937524791361, -294.0767609092507087, -322.1511459606825269 ) ) ;
#29819 = CARTESIAN_POINT ( 'NONE',  ( 19.29814411840298050, -295.6384095970662997, -317.3430609234796407 ) ) ;
#29820 = DIRECTION ( 'NONE',  ( -0.2456588035076310295, 0.9693563597868428694, 0.000000000000000000 ) ) ;
#29821 = CARTESIAN_POINT ( 'NONE',  ( -47.80604814447011108, -295.9913262450705247, -342.8217581472771371 ) ) ;
#29822 = CARTESIAN_POINT ( 'NONE',  ( 151.9709352735115147, -299.5541904835127980, -195.3611179825600175 ) ) ;
#29824 = CARTESIAN_POINT ( 'NONE',  ( -109.2758583226734999, -296.7161096486238421, -257.9322449509696753 ) ) ;
#29823 = CARTESIAN_POINT ( 'NONE',  ( -106.4082784846803520, -282.9663592302003394, -240.0941494502931448 ) ) ;
#29825 = CARTESIAN_POINT ( 'NONE',  ( -105.4320937364439459, -285.0176559456355676, -234.2928403639612043 ) ) ;
#29826 = CARTESIAN_POINT ( 'NONE',  ( 31.09865369464192497, -283.8915037598907816, -302.5037184260195318 ) ) ;
#29827 = CARTESIAN_POINT ( 'NONE',  ( 14.58631384061667902, -288.0119228364881678, -327.2596236029493184 ) ) ;
#29828 = CARTESIAN_POINT ( 'NONE',  ( -25.08432277463506921, -290.2085090175638129, -196.4856837645282326 ) ) ;
#29829 = CARTESIAN_POINT ( 'NONE',  ( -112.5573669640215400, -277.9469855783382854, -254.5890389006116266 ) ) ;
#29830 = CARTESIAN_POINT ( 'NONE',  ( -85.33152481854862970, -281.1952119285918457, -330.4860931364851808 ) ) ;
#29831 = CARTESIAN_POINT ( 'NONE',  ( -43.40344324565903378, -262.7186194818502827, -501.1297839416856164 ) ) ;
#29832 = CARTESIAN_POINT ( 'NONE',  ( 34.10033695288255018, -286.1255794015199854, -253.4792213777357688 ) ) ;
#29833 = CARTESIAN_POINT ( 'NONE',  ( -110.9316640555430951, -289.7443468063224259, -248.7738597223181785 ) ) ;
#29834 = DIRECTION ( 'NONE',  ( 0.000000000000000000, 0.000000000000000000, 1.000000000000000000 ) ) ;
#29835 = CARTESIAN_POINT ( 'NONE',  ( -104.4545002634570778, -298.5632294854839870, -239.5409319625470062 ) ) ;
#29836 = CARTESIAN_POINT ( 'NONE',  ( -104.2861592644941169, -280.4582188159449174, -233.5230170216956935 ) ) ;
#29838 = CARTESIAN_POINT ( 'NONE',  ( 27.80217441984163429, -280.7697317689558076, -237.2586403522886087 ) ) ;
#29837 = CARTESIAN_POINT ( 'NONE',  ( -27.97776951857643013, -292.9540812017858684, -345.1844125850856244 ) ) ;
#29839 = CARTESIAN_POINT ( 'NONE',  ( 25.71587312414331805, -294.3034169401998952, -314.5739754410757882 ) ) ;
#29840 = CARTESIAN_POINT ( 'NONE',  ( -4.100380887461235524, -284.5668441562411317, -202.4916536080753815 ) ) ;
#29841 = CARTESIAN_POINT ( 'NONE',  ( -109.5089367781370555, -280.2895844519035791, -290.7790171108649133 ) ) ;
#29842 = CARTESIAN_POINT ( 'NONE',  ( -88.67529979404858409, -294.8526760979827372, -322.6652419775610952 ) ) ;
#29843 = ORIENTED_EDGE ( 'NONE', *, *, #93160, .T. ) ;
#29844 = FACE_OUTER_BOUND ( 'NONE', #50121, .T. ) ;
#29845 = CARTESIAN_POINT ( 'NONE',  ( 34.69441767856497449, -283.2787612697925965, -250.7509760322479906 ) ) ;
#29846 = CARTESIAN_POINT ( 'NONE',  ( -42.40023858212408925, -294.6253196379149131, -343.2473281353082371 ) ) ;
#29847 = DIRECTION ( 'NONE',  ( 0.000000000000000000, 0.000000000000000000, 1.000000000000000000 ) ) ;
#29848 = CARTESIAN_POINT ( 'NONE',  ( -69.91165696735023971, -274.9809262143061233, -337.9199732462171255 ) ) ;
#29849 = CARTESIAN_POINT ( 'NONE',  ( -44.01851614842487947, -273.1670796337138540, -193.7600351154993348 ) ) ;
#29850 = ADVANCED_FACE ( 'NONE', ( #46292 ), #75196, .T. ) ;
#29851 = CARTESIAN_POINT ( 'NONE',  ( -99.71050631250705010, -290.9079440987432008, -232.4252244301009114 ) ) ;
#29852 = CARTESIAN_POINT ( 'NONE',  ( -39.74303679590553884, -281.5416073825505237, -196.6942784055590039 ) ) ;
#29853 = CARTESIAN_POINT ( 'NONE',  ( 19.60328686438878520, -276.4941641392466636, -223.4174403061531962 ) ) ;
#29854 = CARTESIAN_POINT ( 'NONE',  ( -37.29407993814776034, -284.6516504174961710, -346.5740357033037071 ) ) ;
#29855 = CARTESIAN_POINT ( 'NONE',  ( 28.50052263533785180, -280.7855805256578492, -302.9099147549125632 ) ) ;
#29856 = CARTESIAN_POINT ( 'NONE',  ( -79.74225785221808849, -279.6250536594727123, -332.2886568374822787 ) ) ;
#29857 = EDGE_LOOP ( 'NONE', ( #3411, #64395, #55491, #62493 ) ) ;
#29858 = CARTESIAN_POINT ( 'NONE',  ( -55.33155968404423675, -273.6601949049922382, -195.4921326973236262 ) ) ;
#29859 = CARTESIAN_POINT ( 'NONE',  ( 22.95707219933349563, -294.8731732784926862, -226.6888813508244027 ) ) ;
#29860 = CARTESIAN_POINT ( 'NONE',  ( 200.4892204403987250, 64.44609543878978286, -7.254661561165810291 ) ) ;
#29861 = FACE_OUTER_BOUND ( 'NONE', #46487, .T. ) ;
#29862 = CARTESIAN_POINT ( 'NONE',  ( 32.27213237797947443, -292.0803596796338866, -300.3970232711724861 ) ) ;
#29863 = CARTESIAN_POINT ( 'NONE',  ( -4.071069848576229333, -274.0108493904762099, -205.3005232761462935 ) ) ;
#29864 = CARTESIAN_POINT ( 'NONE',  ( 208.6208076322478746, 32.98517505407394168, 9.000000000000001776 ) ) ;
#29865 = CARTESIAN_POINT ( 'NONE',  ( 23.41136716800506079, -294.4511363629974312, -224.1685001544242937 ) ) ;
#29867 = CARTESIAN_POINT ( 'NONE',  ( -70.73853485298552357, -292.8264709683612068, -201.4215781596171269 ) ) ;
#29866 = CARTESIAN_POINT ( 'NONE',  ( -114.2704648735229114, -281.0519495502701943, -270.3937649182068981 ) ) ;
#29868 = EDGE_CURVE ( 'NONE', #39851, #4210, #12568, .T. ) ;
#29869 = CARTESIAN_POINT ( 'NONE',  ( -48.30502295628507170, -291.1920234105690497, -344.4393204964492270 ) ) ;
#29870 = CARTESIAN_POINT ( 'NONE',  ( 37.53276211602584311, -273.5684581208294048, -271.6411216969615907 ) ) ;
#29871 = CARTESIAN_POINT ( 'NONE',  ( -21.31971061796216205, -278.7653718859305059, -343.1094634837012336 ) ) ;
#29872 = CARTESIAN_POINT ( 'NONE',  ( -6.184020329435577779, -292.7193597693570268, -337.9666886910082439 ) ) ;
#29873 = CARTESIAN_POINT ( 'NONE',  ( -39.57497621063551918, -281.8848327648923373, -194.6163948914206401 ) ) ;
#29874 = VERTEX_POINT ( 'NONE', #26406 ) ;
#29875 = CARTESIAN_POINT ( 'NONE',  ( -16.13041171608157853, -282.4369113983623834, -340.2336356887971078 ) ) ;
#29876 = CARTESIAN_POINT ( 'NONE',  ( -82.06976748427655366, -280.5375797162723757, -208.0643082766190730 ) ) ;
#29877 = CARTESIAN_POINT ( 'NONE',  ( 4.316821878109750266, -281.2991373976518048, -334.7089206967824566 ) ) ;
#29878 = CARTESIAN_POINT ( 'NONE',  ( -80.08519197534438661, -278.5562526798925091, -334.1888374775280681 ) ) ;
#29879 = CARTESIAN_POINT ( 'NONE',  ( 0.000000000000000000, 0.000000000000000000, 0.000000000000000000 ) ) ;
#29880 = CARTESIAN_POINT ( 'NONE',  ( -5.555776691504733300, -278.1617103164889500, -339.7323139232078120 ) ) ;
#29881 = EDGE_CURVE ( 'NONE', #6956, #70876, #40114, .T. ) ;
#29882 = CARTESIAN_POINT ( 'NONE',  ( -37.30987171927208124, -285.5519495502701375, -340.3611179825599606 ) ) ;
#29883 = ORIENTED_EDGE ( 'NONE', *, *, #80555, .T. ) ;
#29884 = CARTESIAN_POINT ( 'NONE',  ( -37.16992363897267637, -300.0544674696619722, -195.3581240247519588 ) ) ;
#29885 = CARTESIAN_POINT ( 'NONE',  ( -26.81390449538187681, -274.9376996216893190, -344.2597804861110831 ) ) ;
#29886 = CARTESIAN_POINT ( 'NONE',  ( -81.36182585714203697, -293.2226735973649738, -208.4240326264954035 ) ) ;
#29887 = CARTESIAN_POINT ( 'NONE',  ( -14.80711000723318271, -291.7005820484347396, -200.8191528386145137 ) ) ;
#29888 = CARTESIAN_POINT ( 'NONE',  ( 5.517839968940424278, -287.9961654821806860, -334.2562408463186898 ) ) ;
#29889 = FACE_OUTER_BOUND ( 'NONE', #48367, .T. ) ;
#29891 = CARTESIAN_POINT ( 'NONE',  ( -87.48720168815138720, -282.1653598646322507, -324.5777872468449914 ) ) ;
#29890 = CARTESIAN_POINT ( 'NONE',  ( 32.79082963577867815, -291.7373925767483911, -240.0290465019735962 ) ) ;
#29892 = CARTESIAN_POINT ( 'NONE',  ( -110.8426426442360366, -292.2762838640759355, -280.8673370803383023 ) ) ;
#29893 = CARTESIAN_POINT ( 'NONE',  ( -108.0143939209926316, -283.3078378712709195, -249.3018142383234874 ) ) ;
#29894 = CARTESIAN_POINT ( 'NONE',  ( 10.24064517707352628, -283.6951550247052865, -326.4384471757738311 ) ) ;
#29895 = CARTESIAN_POINT ( 'NONE',  ( -12.28915658069333894, -289.6754272798460761, -342.9784532819220999 ) ) ;
#29896 = CARTESIAN_POINT ( 'NONE',  ( 35.62769696183987378, -282.0928510664701889, -274.0292959800119661 ) ) ;
#29897 = CARTESIAN_POINT ( 'NONE',  ( 32.96606803641201822, -291.9575536951258528, -239.9501585557781596 ) ) ;
#29898 = CARTESIAN_POINT ( 'NONE',  ( -7.415474350190210728, -287.2373957677201588, -199.5332645620786991 ) ) ;
#29899 = CARTESIAN_POINT ( 'NONE',  ( 37.08647723653804462, -288.2886935976654854, -289.8540222710630019 ) ) ;
#29900 = CARTESIAN_POINT ( 'NONE',  ( -103.4863637256166840, -285.1373171418991888, -239.3562761901939098 ) ) ;
#29901 = ORIENTED_EDGE ( 'NONE', *, *, #54992, .T. ) ;
#29902 = CARTESIAN_POINT ( 'NONE',  ( 194.5542095385274592, 25.91226055734863465, 14.23298358910922445 ) ) ;
#29903 = CARTESIAN_POINT ( 'NONE',  ( -8.830514221867677094, -296.5436719518422706, -340.6122701827032415 ) ) ;
#29904 = CARTESIAN_POINT ( 'NONE',  ( -61.45214101821655817, -294.0436133027067171, -343.0249402414153792 ) ) ;
#29905 = CARTESIAN_POINT ( 'NONE',  ( -109.3613197716933172, -277.7856305141615962, -257.0726705564470080 ) ) ;
#29906 = CARTESIAN_POINT ( 'NONE',  ( -9.148401514218059916, -297.7450392380144990, -193.4660680483073634 ) ) ;
#29907 = CARTESIAN_POINT ( 'NONE',  ( 34.74175376992908326, -292.2330047438293263, -285.7409537183996804 ) ) ;
#29908 = CARTESIAN_POINT ( 'NONE',  ( -3.663327443979457421, -276.2629734623603213, -204.4398270365678627 ) ) ;
#29909 = CARTESIAN_POINT ( 'NONE',  ( -107.8412844219014914, -294.4953213123518481, -293.0612262769406584 ) ) ;
#29910 = CARTESIAN_POINT ( 'NONE',  ( 26.14376430493017978, -295.2598141657338147, -307.1948838743196575 ) ) ;
#29911 = CARTESIAN_POINT ( 'NONE',  ( 19.07977054083941226, -295.2928646163152280, -317.1675675605621336 ) ) ;
#29912 = DIRECTION ( 'NONE',  ( 0.000000000000000000, -1.000000000000000000, 0.000000000000000000 ) ) ;
#29913 = CARTESIAN_POINT ( 'NONE',  ( 3.216127482886622424, -292.5088930857937726, -333.7081762068345370 ) ) ;
#29914 = CARTESIAN_POINT ( 'NONE',  ( -38.50419039950298838, -300.0377411448425278, -195.3669752758073059 ) ) ;
#29915 = CARTESIAN_POINT ( 'NONE',  ( -110.0215577713507002, -291.3750310829137788, -279.3637143287406843 ) ) ;
#29916 = CARTESIAN_POINT ( 'NONE',  ( -10.47827546018375955, -295.0250189982331221, -338.2613676279515289 ) ) ;
#29917 = CARTESIAN_POINT ( 'NONE',  ( -109.0926182891334690, -280.2342611680612663, -293.5552870345799192 ) ) ;
#29918 = CARTESIAN_POINT ( 'NONE',  ( -56.41740065600621534, -278.4962791015083212, -196.2158807661456876 ) ) ;
#29919 = EDGE_LOOP ( 'NONE', ( #29679, #82295, #69915, #56670 ) ) ;
#29920 = CARTESIAN_POINT ( 'NONE',  ( 30.44928143128743159, -275.3718034325327721, -306.7736058058741264 ) ) ;
#29921 = CARTESIAN_POINT ( 'NONE',  ( 26.78739038945298034, -280.1423610684755090, -308.2620461847151887 ) ) ;
#29922 = CARTESIAN_POINT ( 'NONE',  ( -61.77165505891698416, -278.1398734266709880, -198.1277936867041376 ) ) ;
#29923 = CARTESIAN_POINT ( 'NONE',  ( -81.14922814223729119, -277.4582436486327879, -209.2797876668647348 ) ) ;
#29924 = CARTESIAN_POINT ( 'NONE',  ( -90.39030626128513290, -295.9667943502856247, -219.4248735958797454 ) ) ;
#29925 = CARTESIAN_POINT ( 'NONE',  ( 29.54807319997954451, -278.0019850777950978, -304.3971766632907361 ) ) ;
#29926 = CARTESIAN_POINT ( 'NONE',  ( 195.0179948445400271, 25.07543301046760931, 13.58130950507239731 ) ) ;
#29927 = CARTESIAN_POINT ( 'NONE',  ( -97.02963520811226772, -289.1997129887546976, -224.3428877661676495 ) ) ;
#29928 = CARTESIAN_POINT ( 'NONE',  ( -96.39105601114142985, -289.8868828867213097, -319.7999217175851641 ) ) ;
#29929 = CARTESIAN_POINT ( 'NONE',  ( 22.99271303944037825, -276.9416516797861618, -225.5304697936171010 ) ) ;
#29930 = CARTESIAN_POINT ( 'NONE',  ( -34.36391085241772458, -296.0893536768662102, -195.5287939806827637 ) ) ;
#29931 = CARTESIAN_POINT ( 'NONE',  ( -108.8744024482532637, -284.1073652428066225, -242.1588253247516320 ) ) ;
#29932 = CARTESIAN_POINT ( 'NONE',  ( 197.4836817735085219, 24.47698789593438917, 11.66666666666666785 ) ) ;
#29933 = CARTESIAN_POINT ( 'NONE',  ( -20.12043501171388016, -280.8308371697673351, -343.4099304285018093 ) ) ;
#29934 = FACE_OUTER_BOUND ( 'NONE', #77397, .T. ) ;
#29935 = CARTESIAN_POINT ( 'NONE',  ( 19.66384094117455561, -291.6963196589528025, -224.1081426606676530 ) ) ;
#29936 = CARTESIAN_POINT ( 'NONE',  ( -77.70106369195956120, -283.6439682641382092, -207.9945426840557730 ) ) ;
#29937 = DIRECTION ( 'NONE',  ( 0.1455045995357758803, 0.000000000000000000, -0.9893575751536618501 ) ) ;
#29938 = CARTESIAN_POINT ( 'NONE',  ( 0.000000000000000000, 0.000000000000000000, 9.000000000000001776 ) ) ;
#29939 = CARTESIAN_POINT ( 'NONE',  ( -14.20589505014096865, -290.3520520576256558, -199.0187380789768952 ) ) ;
#29940 = CARTESIAN_POINT ( 'NONE',  ( -45.98175064150800040, -278.7635263870486710, -343.7047937132116431 ) ) ;
#29941 = CARTESIAN_POINT ( 'NONE',  ( -4.321026238989570167, -283.8316289799137166, -339.4960361997546556 ) ) ;
#29943 = CARTESIAN_POINT ( 'NONE',  ( -74.72010898547075897, -285.5395231114922581, -207.6566161402693638 ) ) ;
#29942 = CARTESIAN_POINT ( 'NONE',  ( 18.97918180914302155, -272.9351792204907952, -219.9128512809309086 ) ) ;
#29944 = CARTESIAN_POINT ( 'NONE',  ( 31.66460719816356573, -276.6392655624655958, -244.7973845798202319 ) ) ;
#29945 = CARTESIAN_POINT ( 'NONE',  ( -26.98858078803188221, -277.7199761807559639, -342.7863528566958280 ) ) ;
#29946 = CARTESIAN_POINT ( 'NONE',  ( -112.2100460062138154, -286.4849981602699245, -275.6040226308801948 ) ) ;
#29947 = CIRCLE ( 'NONE', #90396, 1.000000000000000888 ) ;
#29948 = ORIENTED_EDGE ( 'NONE', *, *, #85740, .F. ) ;
#29949 = DIRECTION ( 'NONE',  ( -1.000000000000000000, 0.000000000000000000, 0.000000000000000000 ) ) ;
#29950 = CARTESIAN_POINT ( 'NONE',  ( -101.6294381441484944, -295.8271253558790477, -312.8378140282363233 ) ) ;
#29951 = CARTESIAN_POINT ( 'NONE',  ( 35.59798520561974300, -289.3273886906071084, -254.4976659571739219 ) ) ;
#29952 = LINE ( 'NONE', #13430, #47299 ) ;
#29953 = CARTESIAN_POINT ( 'NONE',  ( -99.90806341382572953, -275.6948066931273047, -220.5068182859052968 ) ) ;
#29954 = CARTESIAN_POINT ( 'NONE',  ( -112.0973290108608609, -277.6874567816421404, -253.2412914115491560 ) ) ;
#29955 = CARTESIAN_POINT ( 'NONE',  ( -79.13840184732436001, -289.8987236365313152, -206.5840362964534336 ) ) ;
#29956 = CARTESIAN_POINT ( 'NONE',  ( -25.04500570273807014, -287.7317941831717576, -197.6491729531099679 ) ) ;
#29957 = CARTESIAN_POINT ( 'NONE',  ( -109.4687845484847060, -280.0955420808243161, -287.0201548553062025 ) ) ;
#29958 = CARTESIAN_POINT ( 'NONE',  ( 37.53455404474896540, -289.1694423256822688, -285.5976811034396405 ) ) ;
#29959 = CARTESIAN_POINT ( 'NONE',  ( -48.60455954803998679, -285.1957341592250259, -344.5106199646174332 ) ) ;
#29960 = CARTESIAN_POINT ( 'NONE',  ( -97.05304629950505557, -278.0662367969564457, -318.9981729088901261 ) ) ;
#29961 = CARTESIAN_POINT ( 'NONE',  ( -110.3172003782366062, -270.7652409192697291, -253.7899142056186292 ) ) ;
#29962 = CARTESIAN_POINT ( 'NONE',  ( -112.9957817693692732, -278.5656195732849483, -255.9567391137153152 ) ) ;
#29963 = CARTESIAN_POINT ( 'NONE',  ( -111.5769001271281269, -274.4122687124617528, -270.3847510867740311 ) ) ;
#29964 = CARTESIAN_POINT ( 'NONE',  ( 156.0793278192250284, 19.12150670425092258, 12.12861874973152609 ) ) ;
#29965 = EDGE_CURVE ( 'NONE', #45777, #90307, #63972, .T. ) ;
#29966 = CARTESIAN_POINT ( 'NONE',  ( 21.31550574532285580, -290.6948066931273615, -317.0979686699210447 ) ) ;
#29967 = CARTESIAN_POINT ( 'NONE',  ( -27.11047220429551174, -272.4202254892947508, -195.0136625216094615 ) ) ;
#29968 = CYLINDRICAL_SURFACE ( 'NONE', #72727, 25.00000000000000355 ) ;
#29969 = CARTESIAN_POINT ( 'NONE',  ( -96.45180268998970519, -278.6602774360619605, -227.4194806487598157 ) ) ;
#29970 = CARTESIAN_POINT ( 'NONE',  ( 38.09837004603772215, -276.5891256373307669, -256.9894630542547134 ) ) ;
#29971 = CARTESIAN_POINT ( 'NONE',  ( -58.08813825178550161, -299.2040577398817049, -199.7568672537821044 ) ) ;
#29972 = CARTESIAN_POINT ( 'NONE',  ( -41.56820766288251434, -282.1627741289096889, -347.0615513430716419 ) ) ;
#29973 = CARTESIAN_POINT ( 'NONE',  ( 35.76360814735154747, -289.4637323633321557, -282.0000611686700722 ) ) ;
#29974 = CARTESIAN_POINT ( 'NONE',  ( -67.91758684803448887, -299.1782786398678127, -200.3918572842549963 ) ) ;
#29975 = CARTESIAN_POINT ( 'NONE',  ( -30.54390017808885105, -299.3405499070659062, -193.7568310456069014 ) ) ;
#29976 = CARTESIAN_POINT ( 'NONE',  ( -31.43280527507423017, -296.9776604949606167, -345.0121771037880762 ) ) ;
#29977 = CARTESIAN_POINT ( 'NONE',  ( 21.12393328062062636, -278.9083044070519009, -223.6513958520252743 ) ) ;
#29978 = CARTESIAN_POINT ( 'NONE',  ( -29.79914699245145471, -272.1682200242870522, -196.0983635609978819 ) ) ;
#29979 = CARTESIAN_POINT ( 'NONE',  ( -12.97897202332027433, -287.9636950450033623, -198.1607170584861706 ) ) ;
#29980 = CARTESIAN_POINT ( 'NONE',  ( -56.15814081689888582, -288.2204752797404694, -341.2670414578177542 ) ) ;
#29981 = CARTESIAN_POINT ( 'NONE',  ( 186.8782473919017946, 262.4247097882764592, -153.1099460133960974 ) ) ;
#29982 = ORIENTED_EDGE ( 'NONE', *, *, #84181, .T. ) ;
#29983 = CARTESIAN_POINT ( 'NONE',  ( -15.14092496997311876, -287.3450151944473419, -343.5309504060106178 ) ) ;
#29984 = CARTESIAN_POINT ( 'NONE',  ( -71.18632843777302810, -289.1785425819629722, -335.0794072839310047 ) ) ;
#29985 = ORIENTED_EDGE ( 'NONE', *, *, #47895, .T. ) ;
#29986 = CARTESIAN_POINT ( 'NONE',  ( -99.10351695446293263, -286.2392355891583975, -224.8097733468155184 ) ) ;
#29987 = CARTESIAN_POINT ( 'NONE',  ( -51.28076609988519152, -277.5685932409912766, -342.0394963578903003 ) ) ;
#29988 = EDGE_CURVE ( 'NONE', #72022, #70265, #89445, .T. ) ;
#29989 = CARTESIAN_POINT ( 'NONE',  ( 30.62203016183847382, -292.9327422715573448, -305.8917227337423128 ) ) ;
#29990 = CARTESIAN_POINT ( 'NONE',  ( 9.153773371139244830, -283.0837082272484508, -331.6104749617016978 ) ) ;
#29991 = CARTESIAN_POINT ( 'NONE',  ( 20.52753454325547366, -282.3945893470113333, -220.6033485129433700 ) ) ;
#29992 = CARTESIAN_POINT ( 'NONE',  ( -92.41564587003446718, -284.1474507654099853, -324.1440594408492188 ) ) ;
#29993 = CARTESIAN_POINT ( 'NONE',  ( 31.08863166773339515, -281.5439148762067134, -244.7331965685933142 ) ) ;
#29994 = CARTESIAN_POINT ( 'NONE',  ( -39.40415736724759910, -139.7686915660002001, -364.8644887815387392 ) ) ;
#29995 = CARTESIAN_POINT ( 'NONE',  ( -97.55334013989948971, -279.9444796973232314, -314.8189110281763874 ) ) ;
#29996 = CARTESIAN_POINT ( 'NONE',  ( -78.88083861134452945, -207.7982064915168223, -356.3615181246614725 ) ) ;
#29997 = CARTESIAN_POINT ( 'NONE',  ( -112.4673293132808567, -270.3863210923503289, -283.6829518252387743 ) ) ;
#29998 = CARTESIAN_POINT ( 'NONE',  ( -109.7410405708451862, -271.8925054879165373, -259.4825570268374690 ) ) ;
#29999 = CARTESIAN_POINT ( 'NONE',  ( 33.35754084228669569, -293.4482082417355286, -300.8459974687801832 ) ) ;
#30000 = CARTESIAN_POINT ( 'NONE',  ( 139.4533679669662263, 178.0281513006911212, -238.5041391399041402 ) ) ;
#30002 = CARTESIAN_POINT ( 'NONE',  ( -72.76051505210691062, -287.9294662818647339, -335.1063723694215923 ) ) ;
#30001 = CARTESIAN_POINT ( 'NONE',  ( 13.64836042249343784, -273.4334447296446342, -213.2524958372876824 ) ) ;
#30003 = CARTESIAN_POINT ( 'NONE',  ( -56.09280974463298008, -297.1565140623127945, -342.2423811376186222 ) ) ;
#30004 = CARTESIAN_POINT ( 'NONE',  ( -34.54255373928891260, -290.3315618426191804, -343.8508612348118163 ) ) ;
#30005 = EDGE_LOOP ( 'NONE', ( #20468, #40087 ) ) ;
#30006 = CARTESIAN_POINT ( 'NONE',  ( -98.08091297443648671, -296.8648691639485264, -317.3032977012418883 ) ) ;
#30007 = CARTESIAN_POINT ( 'NONE',  ( -67.57888449906954520, -286.1367378164160300, -203.8502081770367340 ) ) ;
#30008 = CARTESIAN_POINT ( 'NONE',  ( 75.67381866370362786, -298.2323840635743295, -193.7806729451839942 ) ) ;
#30009 = CARTESIAN_POINT ( 'NONE',  ( -33.55756416519896845, -292.9014776589032181, -193.6158305978021588 ) ) ;
#30010 = CARTESIAN_POINT ( 'NONE',  ( 38.54662636682888177, -294.2040597308703127, -283.1094011584139594 ) ) ;
#30011 = EDGE_CURVE ( 'NONE', #44324, #69962, #2345, .T. ) ;
#30012 = CARTESIAN_POINT ( 'NONE',  ( -33.51055871306127187, -292.2683635459865172, -197.4492268861841069 ) ) ;
#30013 = EDGE_LOOP ( 'NONE', ( #39926, #76600, #28267, #82621 ) ) ;
#30014 = CARTESIAN_POINT ( 'NONE',  ( -108.7491497465764496, -274.7896804215772590, -245.6570629309408105 ) ) ;
#30015 = CARTESIAN_POINT ( 'NONE',  ( 35.67946665432231157, -274.6395634983861669, -293.5110190674261617 ) ) ;
#30016 = VERTEX_POINT ( 'NONE', #84149 ) ;
#30017 = CARTESIAN_POINT ( 'NONE',  ( -70.28036672877185254, -276.9822713270783083, -339.9066247533874616 ) ) ;
#30018 = AXIS2_PLACEMENT_3D ( 'NONE', #70813, #18266, #69864 ) ;
#30019 = CARTESIAN_POINT ( 'NONE',  ( -74.66052174613601267, -271.9469144356937136, -206.6328940859135059 ) ) ;
#30020 = CARTESIAN_POINT ( 'NONE',  ( 20.97838420434981899, -274.3291137859762330, -316.3123259680433534 ) ) ;
#30021 = CARTESIAN_POINT ( 'NONE',  ( -110.6513237473105562, -273.6675820552150640, -267.6394394776495460 ) ) ;
#30022 = CARTESIAN_POINT ( 'NONE',  ( -108.1707341681382246, -273.7407859269225696, -251.5478278179002984 ) ) ;
#30023 = CARTESIAN_POINT ( 'NONE',  ( -110.0738327710919719, -274.5941884866206237, -248.1808289681541453 ) ) ;
#30024 = CARTESIAN_POINT ( 'NONE',  ( -8.537194773463797404, -274.6971543346402314, -340.0077547523985118 ) ) ;
#30025 = CARTESIAN_POINT ( 'NONE',  ( -96.48600631320077525, -296.6028735124316995, -313.3457638829561347 ) ) ;
#30026 = CARTESIAN_POINT ( 'NONE',  ( 34.89937600890105784, -292.3103621829958456, -284.3825956873396308 ) ) ;
#30027 = CARTESIAN_POINT ( 'NONE',  ( 29.33919985515026596, -212.1443419142231051, 22.50000000000000000 ) ) ;
#30028 = CARTESIAN_POINT ( 'NONE',  ( -9.228462278270455954, -277.1866261001693488, -341.9793611950705667 ) ) ;
#30029 = CARTESIAN_POINT ( 'NONE',  ( 32.85943054869840552, -275.4519780082069360, -250.1604922053381586 ) ) ;
#30030 = SHAPE_REPRESENTATION ( 'Heavy-Duty Plastic Foot Pedal', ( #18940 ), #47644 ) ;
#30031 = CARTESIAN_POINT ( 'NONE',  ( -113.8475389179158554, -283.2419334603202969, -269.9675414550841879 ) ) ;
#30032 = CARTESIAN_POINT ( 'NONE',  ( -68.73837105258257907, -297.4640084042130184, -338.6707206451707748 ) ) ;
#30033 = LINE ( 'NONE', #220, #92848 ) ;
#30034 =( BOUNDED_SURFACE ( )  B_SPLINE_SURFACE ( 3, 2, ( 
 ( #61704, #40351, #32814 ),
 ( #11967, #25696, #34225 ),
 ( #69268, #91960, #40815 ),
 ( #25243, #69732, #55062 ),
 ( #76840, #19537, #82990 ),
 ( #27115, #54117, #4397 ) ),
 .UNSPECIFIED., .F., .F., .F. ) 
 B_SPLINE_SURFACE_WITH_KNOTS ( ( 4, 2, 4 ),
 ( 3, 3 ),
 ( 2.168404344971008868E-19, 0.001011634320662447954, 0.002023268641324895908 ),
 ( 0.000000000000000000, 1.000000000000000000 ),
 .UNSPECIFIED. ) 
 GEOMETRIC_REPRESENTATION_ITEM ( )  RATIONAL_B_SPLINE_SURFACE ( (
 ( 1.000000000000000000, 0.5021841165015733521, 1.000000000000000000),
 ( 1.000000000000000000, 0.5023663462998690932, 1.000000000000000000),
 ( 1.000000000000000000, 0.5117996075019977109, 1.000000000000000000),
 ( 1.000000000000000000, 0.5521543867336666800, 1.000000000000000000),
 ( 1.000000000000000000, 0.5833157748965640543, 1.000000000000000000),
 ( 1.000000000000000000, 0.6287211027133851049, 1.000000000000000000) ) ) 
 REPRESENTATION_ITEM ( '' )  SURFACE ( )  );
#30035 = CARTESIAN_POINT ( 'NONE',  ( -4.512958728645550366, -285.6934359570981883, -204.9785861745966713 ) ) ;
#30036 = CARTESIAN_POINT ( 'NONE',  ( -89.81991322911061104, -276.0447080517561744, -322.6259787593550072 ) ) ;
#30037 = CARTESIAN_POINT ( 'NONE',  ( -110.8696145703247851, -277.0875692513499189, -273.3645682251929543 ) ) ;
#30038 = CARTESIAN_POINT ( 'NONE',  ( -104.0484609425845832, -286.0974965998791504, -304.7544469944687080 ) ) ;
#30039 = CARTESIAN_POINT ( 'NONE',  ( -11.36396509403575550, -275.6032351762364101, -201.6606773979221430 ) ) ;
#30040 = DIRECTION ( 'NONE',  ( 1.000000000000000000, 0.000000000000000000, 0.000000000000000000 ) ) ;
#30041 = CARTESIAN_POINT ( 'NONE',  ( 25.39650288484879326, -274.5300512640397983, -313.7000507973789922 ) ) ;
#30042 = CARTESIAN_POINT ( 'NONE',  ( -35.40931205529849990, -282.0764801125492340, -195.2064657382867097 ) ) ;
#30043 = CARTESIAN_POINT ( 'NONE',  ( 193.9646936176702070, 20.00000000000000000, 15.00000000000000000 ) ) ;
#30044 = CARTESIAN_POINT ( 'NONE',  ( 31.39176801577343312, -289.0619864328721178, -238.8501517250077200 ) ) ;
#30045 = CARTESIAN_POINT ( 'NONE',  ( 155.7883889513935856, 17.75303870060648848, -10.69672886740455198 ) ) ;
#30046 = CARTESIAN_POINT ( 'NONE',  ( 28.50831549217935290, -291.0737347051569941, -234.3548185962341677 ) ) ;
#30047 = CARTESIAN_POINT ( 'NONE',  ( 82.16780035446942065, -298.0667158113331539, -196.7127616594630979 ) ) ;
#30048 = CARTESIAN_POINT ( 'NONE',  ( -37.13315689824700883, -296.8497504458034655, -196.9612216088964090 ) ) ;
#30049 = CARTESIAN_POINT ( 'NONE',  ( -97.75296974734445143, -289.2855391032036891, -227.1309089878609768 ) ) ;
#30050 = CARTESIAN_POINT ( 'NONE',  ( -90.99921415893403775, -226.8295888252787904, -341.9546587472784154 ) ) ;
#30051 = CARTESIAN_POINT ( 'NONE',  ( -37.11877477909561662, -296.0547944529405981, -195.3582583741226131 ) ) ;
#30052 = CARTESIAN_POINT ( 'NONE',  ( 36.02998097164891789, -285.7647676252742599, -249.2137420695398760 ) ) ;
#30053 = CARTESIAN_POINT ( 'NONE',  ( -112.4819032575698117, -282.9397404332834753, -258.7044807618646587 ) ) ;
#30054 = CARTESIAN_POINT ( 'NONE',  ( -80.96091704444086190, -285.0824722826523043, -329.6928690095891170 ) ) ;
#30055 = CARTESIAN_POINT ( 'NONE',  ( -32.12400417514923845, -283.7874863284671960, -343.3363012714660272 ) ) ;
#30056 = CARTESIAN_POINT ( 'NONE',  ( -94.20030341461031753, -291.8489665307449741, -319.8131759508264622 ) ) ;
#30057 = CARTESIAN_POINT ( 'NONE',  ( 16.00932649370802352, -275.1172660779564580, -214.8686657942969020 ) ) ;
#30058 = CARTESIAN_POINT ( 'NONE',  ( -2.487126102765745195, -286.6745662429819390, -337.4019478571352124 ) ) ;
#30059 = CARTESIAN_POINT ( 'NONE',  ( 20.03586956164628674, -274.8550232325782758, -218.9328398031620964 ) ) ;
#30060 = CARTESIAN_POINT ( 'NONE',  ( 30.21667873787950498, -295.1112435826379397, -238.4947318829150618 ) ) ;
#30061 = CARTESIAN_POINT ( 'NONE',  ( -48.18343439339133027, -271.5660680172725847, -437.8871425252946210 ) ) ;
#30062 = CARTESIAN_POINT ( 'NONE',  ( 31.98288692825981272, -290.4805209788416391, -303.7098442033569654 ) ) ;
#30063 = CARTESIAN_POINT ( 'NONE',  ( -33.48699578476516336, -281.6874736373272867, -343.7657692059435135 ) ) ;
#30064 = CARTESIAN_POINT ( 'NONE',  ( -110.0604580777789891, -276.3074393655558083, -289.4383380576616673 ) ) ;
#30065 = CARTESIAN_POINT ( 'NONE',  ( -113.6476476313650039, -271.0681364600990264, -267.5001605809566172 ) ) ;
#30066 = CARTESIAN_POINT ( 'NONE',  ( 17.50622294442265314, -275.5900778153945794, -318.7080247415787539 ) ) ;
#30067 = CARTESIAN_POINT ( 'NONE',  ( 34.89229081766575291, -294.8815809324760266, -255.7680269389747139 ) ) ;
#30068 = CARTESIAN_POINT ( 'NONE',  ( -3.538274810502163081, -293.4511511784415916, -205.3939194473625207 ) ) ;
#30069 = CARTESIAN_POINT ( 'NONE',  ( -107.4999556749206420, -286.6230525061420735, -246.6252257697056791 ) ) ;
#30070 = CARTESIAN_POINT ( 'NONE',  ( 38.63817475728407658, -294.8691996773992514, -261.7739678749244376 ) ) ;
#30071 = CARTESIAN_POINT ( 'NONE',  ( 36.22532197238260920, -294.6017784424034858, -249.3088597534250539 ) ) ;
#30072 = CARTESIAN_POINT ( 'NONE',  ( -95.60561350151522220, -295.7674127605293393, -314.3625748173021748 ) ) ;
#30073 = CARTESIAN_POINT ( 'NONE',  ( -98.16607978952185931, -291.9549833876038178, -314.2404467087722537 ) ) ;
#30074 = CARTESIAN_POINT ( 'NONE',  ( -31.63417057372542374, -283.1486881293692477, -347.1625628321319255 ) ) ;
#30075 = CARTESIAN_POINT ( 'NONE',  ( -105.7181357150988390, -271.1169341839197386, -237.7272623386999442 ) ) ;
#30076 = CARTESIAN_POINT ( 'NONE',  ( -111.7206598785377736, -284.6371440577562453, -250.2416453859408421 ) ) ;
#30077 = CARTESIAN_POINT ( 'NONE',  ( -40.55182215883634456, -279.0725820021370964, -344.9496096060988748 ) ) ;
#30078 = EDGE_CURVE ( 'NONE', #52100, #15639, #19297, .T. ) ;
#30079 = CARTESIAN_POINT ( 'NONE',  ( -109.5811216921551647, -283.5183593570602625, -257.3060235623159429 ) ) ;
#30080 = VECTOR ( 'NONE', #79666, 1000.000000000000000 ) ;
#30081 = CARTESIAN_POINT ( 'NONE',  ( 20.83714860548262848, -286.2041736574634569, -317.7123064628988800 ) ) ;
#30082 = CARTESIAN_POINT ( 'NONE',  ( -102.3395509548886793, -277.2088415202943565, -231.3286469396649068 ) ) ;
#30083 = CARTESIAN_POINT ( 'NONE',  ( 20.69763459394507876, -20.92298310053570987, -343.0354172471594438 ) ) ;
#30084 = CARTESIAN_POINT ( 'NONE',  ( -62.57824881752455326, -285.2224795249605904, -201.7425614640241918 ) ) ;
#30085 = CARTESIAN_POINT ( 'NONE',  ( -3.845167379837290955, -281.6892877888157045, -201.4555229861685746 ) ) ;
#30086 = CARTESIAN_POINT ( 'NONE',  ( -103.6014096522708456, -289.1036897349030710, -309.2280077320278338 ) ) ;
#30087 = CARTESIAN_POINT ( 'NONE',  ( -41.32206616372621966, -278.7015733503956767, -346.4701626419461604 ) ) ;
#30088 = CARTESIAN_POINT ( 'NONE',  ( -54.00740367314978130, -278.5768304575398702, -345.0850289331229988 ) ) ;
#30089 = CARTESIAN_POINT ( 'NONE',  ( -79.05312907520827537, -279.3051648116177148, -210.4515469635940690 ) ) ;
#30090 = CARTESIAN_POINT ( 'NONE',  ( -5.857653699906765432, -276.4480281633591403, -202.6809759385448331 ) ) ;
#30091 = CARTESIAN_POINT ( 'NONE',  ( 39.23706863851335669, -293.6588784897912205, -278.8948681107987113 ) ) ;
#30092 = CARTESIAN_POINT ( 'NONE',  ( -12.76968975586291144, -286.7512578224150843, -340.8456064029622894 ) ) ;
#30093 = CARTESIAN_POINT ( 'NONE',  ( 6.024049977756507523, -294.2299127158751730, -207.7044971708718037 ) ) ;
#30094 = CARTESIAN_POINT ( 'NONE',  ( 3.979331734179064828, -293.4011930418107568, -330.9152127969904313 ) ) ;
#30095 = CARTESIAN_POINT ( 'NONE',  ( -9.226661275993837563, -294.3409088006461616, -337.7663594828489977 ) ) ;
#30096 = CARTESIAN_POINT ( 'NONE',  ( -96.34987631706967193, -292.2933245109340987, -221.3558453921922080 ) ) ;
#30097 = CARTESIAN_POINT ( 'NONE',  ( 26.94863035827613373, -282.6776424858046539, -305.1554576634643468 ) ) ;
#30098 = EDGE_CURVE ( 'NONE', #11198, #90976, #28995, .T. ) ;
#30099 = ADVANCED_FACE ( 'NONE', ( #41032 ), #72854, .T. ) ;
#30100 = CARTESIAN_POINT ( 'NONE',  ( -110.8084256622462220, -271.8932312149723884, -247.9205677568280350 ) ) ;
#30101 = CARTESIAN_POINT ( 'NONE',  ( 34.97944124457312398, -288.5357862830449562, -296.6496934112837494 ) ) ;
#30102 = CARTESIAN_POINT ( 'NONE',  ( 3.853887760259127937, -280.6439027716538135, -334.0095040467646186 ) ) ;
#30103 = CARTESIAN_POINT ( 'NONE',  ( -54.49277334157021357, -289.5998441888542629, -345.4597011814711323 ) ) ;
#30104 = CARTESIAN_POINT ( 'NONE',  ( -39.97893106012885767, -286.3513873727571308, -197.3876125175493712 ) ) ;
#30105 = CARTESIAN_POINT ( 'NONE',  ( 175.2296996224750103, 20.99999999999998934, 0.000000000000000000 ) ) ;
#30106 = CARTESIAN_POINT ( 'NONE',  ( 43.52240465396816660, 12.61540204620569661, -329.8876815671075065 ) ) ;
#30107 = CARTESIAN_POINT ( 'NONE',  ( -76.97335133370192750, -207.9390729104919444, -353.3932181474779668 ) ) ;
#30108 = CARTESIAN_POINT ( 'NONE',  ( -104.4235273460602116, -277.3560603860048559, -299.6879357763577900 ) ) ;
#30109 = CARTESIAN_POINT ( 'NONE',  ( -83.21083283242153072, -276.6175152124334886, -327.6125498659733921 ) ) ;
#30110 = CARTESIAN_POINT ( 'NONE',  ( -76.41832785919542914, -273.2116073542446202, -203.9763683654935846 ) ) ;
#30111 = CARTESIAN_POINT ( 'NONE',  ( 194.7859659566919106, 275.7971500590870733, -124.4546405686035797 ) ) ;
#30112 = CARTESIAN_POINT ( 'NONE',  ( -79.56991505802331233, -278.0688319646793047, -206.6157588735346451 ) ) ;
#30113 = CARTESIAN_POINT ( 'NONE',  ( 6.053921781341184527, -296.2328380008998465, -332.8014734866216600 ) ) ;
#30114 = CARTESIAN_POINT ( 'NONE',  ( -70.25404820465854527, -292.0985273036471881, -205.1325522621764605 ) ) ;
#30115 = CARTESIAN_POINT ( 'NONE',  ( -7.792268875157949637, -275.3711503760661685, -199.4552005377946102 ) ) ;
#30116 = CARTESIAN_POINT ( 'NONE',  ( -94.49831384166250814, -288.5879388392519331, -316.5603061620244603 ) ) ;
#30117 = CARTESIAN_POINT ( 'NONE',  ( -71.36517467702078932, -274.2660347085600847, -201.3994187086739771 ) ) ;
#30118 = CARTESIAN_POINT ( 'NONE',  ( -94.45264787283750252, -297.3609209418207229, -224.8931110739979147 ) ) ;
#30119 = EDGE_LOOP ( 'NONE', ( #85209, #12735, #25616, #60863 ) ) ;
#30120 = CYLINDRICAL_SURFACE ( 'NONE', #71966, 7.500000000000013323 ) ;
#30121 = CARTESIAN_POINT ( 'NONE',  ( -112.3338901535364300, -280.3492042132492656, -280.0201395498779107 ) ) ;
#30122 = B_SPLINE_CURVE_WITH_KNOTS ( 'NONE', 3,
 ( #27358, #86965, #56246, #85575 ),
 .UNSPECIFIED., .F., .F.,
 ( 4, 4 ),
 ( 6.938893903907228378E-18, 0.001032852107770759233 ),
 .UNSPECIFIED. ) ;
#30123 = CARTESIAN_POINT ( 'NONE',  ( -109.1929490945742174, -279.8237491719950185, -255.7507178831741612 ) ) ;
#30124 = CARTESIAN_POINT ( 'NONE',  ( -98.62409087331593582, -280.9171217818589525, -225.4120688187577173 ) ) ;
#30125 = CARTESIAN_POINT ( 'NONE',  ( -46.24351805935556570, -272.4170462749300441, -197.2074072826019631 ) ) ;
#30126 = CARTESIAN_POINT ( 'NONE',  ( 180.7287904564219332, 276.0000000000000568, -24.90000000000003411 ) ) ;
#30127 = DIRECTION ( 'NONE',  ( 0.8043439146810367202, -0.5941640067486294585, 0.000000000000000000 ) ) ;
#30128 = CARTESIAN_POINT ( 'NONE',  ( -89.47506570765176548, -279.4591624156437888, -219.1904344299709919 ) ) ;
#30129 = CARTESIAN_POINT ( 'NONE',  ( 39.22047409388549966, -276.4365822727612567, -276.8720548231434009 ) ) ;
#30130 = CARTESIAN_POINT ( 'NONE',  ( 37.15421243576869159, -277.6693848272579430, -279.4788039863135509 ) ) ;
#30131 = CARTESIAN_POINT ( 'NONE',  ( -108.1175415534468129, -276.7583173844070643, -299.1601902256080052 ) ) ;
#30132 = VERTEX_POINT ( 'NONE', #90305 ) ;
#30133 = CARTESIAN_POINT ( 'NONE',  ( 210.7238915819278589, 32.98517505407394168, 12.09245862095555601 ) ) ;
#30134 = CARTESIAN_POINT ( 'NONE',  ( -27.56008033704150151, -284.9085126768122223, -345.1309870343359307 ) ) ;
#30135 = CARTESIAN_POINT ( 'NONE',  ( -79.61569437200199673, -290.6619683924230912, -210.5871261692188909 ) ) ;
#30136 = CARTESIAN_POINT ( 'NONE',  ( 38.19162196685588384, -286.7201203067720030, -255.9378714625147779 ) ) ;
#30137 = CARTESIAN_POINT ( 'NONE',  ( -48.50331597433281416, -281.4360380136679396, -343.5279980811232576 ) ) ;
#30138 = CARTESIAN_POINT ( 'NONE',  ( 18.03639702554986002, -280.8128498098408841, -318.8239003397196711 ) ) ;
#30139 = AXIS2_PLACEMENT_3D ( 'NONE', #81494, #37478, #1504 ) ;
#30140 = CARTESIAN_POINT ( 'NONE',  ( 21.63894991998256145, -282.1477639851155459, -226.6545790307598054 ) ) ;
#30141 = CARTESIAN_POINT ( 'NONE',  ( -86.70047571675702613, -271.3662507222570639, -213.8234097619546219 ) ) ;
#30142 = CARTESIAN_POINT ( 'NONE',  ( -67.58279608179554998, -281.8422218276042486, -340.3033550954222051 ) ) ;
#30143 = CARTESIAN_POINT ( 'NONE',  ( 7.725231197364196056, -296.4369795947166608, -330.3108664946351496 ) ) ;
#30144 = CARTESIAN_POINT ( 'NONE',  ( -109.3851267025530092, -279.0393106004819970, -282.8301124329083223 ) ) ;
#30145 = CARTESIAN_POINT ( 'NONE',  ( -33.83886628530915175, -288.0962950638214579, -195.2761089353646469 ) ) ;
#30146 = CARTESIAN_POINT ( 'NONE',  ( 152.6876711748310242, 19.85946110189832581, 8.896468494892323164 ) ) ;
#30147 = CARTESIAN_POINT ( 'NONE',  ( -71.54276086448386707, -293.5241592926616363, -202.9702239270277175 ) ) ;
#30148 = CARTESIAN_POINT ( 'NONE',  ( 32.12099931849648016, -273.9223669930391338, -298.7822961012818723 ) ) ;
#30149 = CARTESIAN_POINT ( 'NONE',  ( 23.15398890556640055, -287.3841174119747848, -317.7577206832503407 ) ) ;
#30150 = CARTESIAN_POINT ( 'NONE',  ( 35.27396229666292271, -291.7792723841939733, -257.1223715479595171 ) ) ;
#30151 = CARTESIAN_POINT ( 'NONE',  ( -93.11172295067521532, -276.5601329371263546, -318.2249669027065124 ) ) ;
#30152 = CARTESIAN_POINT ( 'NONE',  ( -97.87648114938544097, -295.2818006853650559, -227.3912940564206053 ) ) ;
#30153 = CARTESIAN_POINT ( 'NONE',  ( -110.7392158005492746, -291.9281324911635807, -265.7210610091478884 ) ) ;
#30154 = DIRECTION ( 'NONE',  ( -0.000000000000000000, -0.000000000000000000, 1.000000000000000000 ) ) ;
#30155 = CARTESIAN_POINT ( 'NONE',  ( 196.0143093133015384, 19.33012701892218743, 12.49999999999999112 ) ) ;
#30156 = CARTESIAN_POINT ( 'NONE',  ( -83.77875105064504169, -294.1561104215476803, -330.9777971006653274 ) ) ;
#30157 = CARTESIAN_POINT ( 'NONE',  ( -6.702765334347680515, -288.0613556947406551, -203.2078647832507556 ) ) ;
#30158 = CARTESIAN_POINT ( 'NONE',  ( -76.62593400905898022, -289.7743471410888105, -205.2564361816217513 ) ) ;
#30159 = ADVANCED_FACE ( 'NONE', ( #69959 ), #32104, .F. ) ;
#30160 = CARTESIAN_POINT ( 'NONE',  ( -61.43089932668555520, -290.7965654293739703, -339.8958963207621764 ) ) ;
#30161 = DIRECTION ( 'NONE',  ( 0.000000000000000000, 0.000000000000000000, 1.000000000000000000 ) ) ;
#30162 = CARTESIAN_POINT ( 'NONE',  ( -106.1810578772126803, -291.0257658261553502, -295.1349863008159105 ) ) ;
#30163 = CARTESIAN_POINT ( 'NONE',  ( 82.70991478241074901, -294.7622393454342955, -192.9651424135201978 ) ) ;
#30164 = CARTESIAN_POINT ( 'NONE',  ( 22.10675684709861244, -289.4088910859131829, -318.6921149016038726 ) ) ;
#30165 = CARTESIAN_POINT ( 'NONE',  ( -42.29618563562885214, -278.0100698489151227, -195.1689649544283327 ) ) ;
#30166 = CARTESIAN_POINT ( 'NONE',  ( -110.5309065621770799, -279.1875282015388393, -246.3364178433875793 ) ) ;
#30167 = CARTESIAN_POINT ( 'NONE',  ( -53.75183047952486959, -279.5139571177062408, -195.0971774618754182 ) ) ;
#30168 = CARTESIAN_POINT ( 'NONE',  ( -24.78250194733549350, -284.2120783827820674, -196.3674413647481458 ) ) ;
#30169 = CARTESIAN_POINT ( 'NONE',  ( 196.7510731661265595, -143.7221692137691775, -21.50000000000000000 ) ) ;
#30170 = CARTESIAN_POINT ( 'NONE',  ( -41.09025825814673993, -278.1440525598329145, -196.2206176219276870 ) ) ;
#30171 = CARTESIAN_POINT ( 'NONE',  ( -93.84520406591781239, -281.8672429109765858, -319.6800260566835163 ) ) ;
#30172 = LINE ( 'NONE', #44826, #47208 ) ;
#30173 = CARTESIAN_POINT ( 'NONE',  ( -92.55855033101936158, -277.7593677169328998, -217.6186982404646244 ) ) ;
#30174 = CARTESIAN_POINT ( 'NONE',  ( -97.45945384162361336, -298.6617925869351211, -227.7399560822100000 ) ) ;
#30175 = CARTESIAN_POINT ( 'NONE',  ( -113.5110258901397344, -283.5846025298166069, -261.4321582250794904 ) ) ;
#30176 = CARTESIAN_POINT ( 'NONE',  ( -104.5320494842226111, -273.7446695103117236, -241.2834475317601459 ) ) ;
#30177 = CARTESIAN_POINT ( 'NONE',  ( -69.89734441942776755, -275.0570847431282004, -201.2184090894064070 ) ) ;
#30178 = CARTESIAN_POINT ( 'NONE',  ( 13.74308875761833626, -275.9788964967798393, -322.6084621437045143 ) ) ;
#30179 = CARTESIAN_POINT ( 'NONE',  ( -25.87723045760135676, -296.9062861080032576, -344.4797160644679366 ) ) ;
#30180 = CARTESIAN_POINT ( 'NONE',  ( -71.90456699023603448, -289.6631102814326937, -339.1681542419446487 ) ) ;
#30181 = CARTESIAN_POINT ( 'NONE',  ( -28.37122901962571220, -278.2448237657351910, -195.2828666228588474 ) ) ;
#30182 = CARTESIAN_POINT ( 'NONE',  ( -98.16091188482273822, -289.7548223246985231, -317.5842424643398658 ) ) ;
#30183 = CARTESIAN_POINT ( 'NONE',  ( -109.4125984186034941, -289.4398581837099300, -283.3685800013030871 ) ) ;
#30184 = CARTESIAN_POINT ( 'NONE',  ( 14.08579696907419176, -290.7735027733177731, -215.6984578696483936 ) ) ;
#30185 = ORIENTED_EDGE ( 'NONE', *, *, #50609, .T. ) ;
#30186 = CARTESIAN_POINT ( 'NONE',  ( 151.4851178187871312, 21.00000000000000000, 3.492110388858666870 ) ) ;
#30187 = CARTESIAN_POINT ( 'NONE',  ( -84.72970518872624268, -289.2334503304113582, -326.0369406580814484 ) ) ;
#30188 = DIRECTION ( 'NONE',  ( -1.000000000000000000, 0.000000000000000000, 0.000000000000000000 ) ) ;
#30189 = CARTESIAN_POINT ( 'NONE',  ( -64.47527094818114790, -286.6477594083775671, -198.5375953359388745 ) ) ;
#30190 = CARTESIAN_POINT ( 'NONE',  ( -82.13390479932378696, -293.9090924074131408, -214.2458315076590907 ) ) ;
#30191 = CARTESIAN_POINT ( 'NONE',  ( -50.43920591083087146, -294.2740786875986601, -346.0540131091070748 ) ) ;
#30192 = CARTESIAN_POINT ( 'NONE',  ( -47.17627517790656100, -284.4897857653093070, -346.2332433351776899 ) ) ;
#30193 = CARTESIAN_POINT ( 'NONE',  ( -71.17633621112906894, -285.4256853905133084, -205.6755909641199196 ) ) ;
#30194 = CARTESIAN_POINT ( 'NONE',  ( -0.3121701844103375589, -275.8707821412817225, -206.8636972637348777 ) ) ;
#30195 = CARTESIAN_POINT ( 'NONE',  ( 22.63331556080247964, -292.1816536754992626, -314.8003382543167845 ) ) ;
#30196 = CARTESIAN_POINT ( 'NONE',  ( -74.46101864683414817, -272.3419033558187721, -206.9833213208681002 ) ) ;
#30197 = EDGE_LOOP ( 'NONE', ( #651, #59016, #54294, #23827, #43680, #48630, #47382, #8540, #20080, #57259, #51084, #10971, #68501, #39872, #27777, #12663, #6827, #35334 ) ) ;
#30198 = CARTESIAN_POINT ( 'NONE',  ( 207.5863589332323329, 29.28491128719180026, 13.57731244650625513 ) ) ;
#30199 = CARTESIAN_POINT ( 'NONE',  ( -1.980971705058676147, -294.2634876193852733, -338.7377454001368733 ) ) ;
#30200 = CARTESIAN_POINT ( 'NONE',  ( 7.780754051210105438, -288.5934833683622855, -211.0906157817430540 ) ) ;
#30201 = CARTESIAN_POINT ( 'NONE',  ( -113.9242464031971167, -297.5693897968903343, -275.3330899628325028 ) ) ;
#30202 = CARTESIAN_POINT ( 'NONE',  ( 34.66634369526079951, -288.0338391656661088, -257.4767836045377294 ) ) ;
#30203 = CARTESIAN_POINT ( 'NONE',  ( -112.7627509267349666, -277.7911728209131752, -255.9910392694391135 ) ) ;
#30204 = CARTESIAN_POINT ( 'NONE',  ( -36.26754100742733300, -295.6904630566978653, -347.2647691543587030 ) ) ;
#30205 = CARTESIAN_POINT ( 'NONE',  ( 22.30021413210127434, -286.3267052447318406, -317.1061646440770119 ) ) ;
#30206 = AXIS2_PLACEMENT_3D ( 'NONE', #3858, #83369, #89533 ) ;
#30207 = CARTESIAN_POINT ( 'NONE',  ( 38.04033725231291641, -293.6894974325553562, -254.6986855815668207 ) ) ;
#30208 = DIRECTION ( 'NONE',  ( 0.000000000000000000, 1.000000000000000000, 0.000000000000000000 ) ) ;
#30209 = CARTESIAN_POINT ( 'NONE',  ( -83.63170945779077670, -373.0521521680024648, -421.1172536214571096 ) ) ;
#30210 = AXIS2_PLACEMENT_3D ( 'NONE', #11982, #40365, #31898 ) ;
#30211 = CARTESIAN_POINT ( 'NONE',  ( 13.76800080992791209, -288.2730208979230611, -213.6289157487942134 ) ) ;
#30212 = CARTESIAN_POINT ( 'NONE',  ( -37.30987171927208834, -283.5523547857346784, -190.3611179825600175 ) ) ;
#30213 = VERTEX_POINT ( 'NONE', #33980 ) ;
#30214 = CARTESIAN_POINT ( 'NONE',  ( -72.45286105436480284, -278.9484061160697479, -201.9321668036308779 ) ) ;
#30215 = CARTESIAN_POINT ( 'NONE',  ( 36.84695773332270363, -283.4212380202399117, -260.1752286230858999 ) ) ;
#30216 = CARTESIAN_POINT ( 'NONE',  ( -109.5359067363892649, -271.2847351524787882, -295.9514105794971215 ) ) ;
#30217 = CARTESIAN_POINT ( 'NONE',  ( -111.6504275734346692, -282.9018657936875343, -288.2159785687240401 ) ) ;
#30218 = CARTESIAN_POINT ( 'NONE',  ( 35.69229606948139377, -285.8191291156263105, -284.8265420699412971 ) ) ;
#30219 = CARTESIAN_POINT ( 'NONE',  ( 27.43400751626292333, -276.8900371757659400, -230.9618491059271435 ) ) ;
#30220 = CARTESIAN_POINT ( 'NONE',  ( -109.3375671564939324, -297.2083773113723737, -257.9279537597230387 ) ) ;
#30221 = ADVANCED_FACE ( 'NONE', ( #62883 ), #65320, .T. ) ;
#30222 = CARTESIAN_POINT ( 'NONE',  ( -31.58029224352640441, -293.6628608937987792, -343.6785451164006417 ) ) ;
#30223 = CARTESIAN_POINT ( 'NONE',  ( -111.3401656600164813, -278.9410550708571463, -291.2785720742067497 ) ) ;
#30224 = CARTESIAN_POINT ( 'NONE',  ( 20.83691996384193601, -276.1717946529852270, -314.4547475020229967 ) ) ;
#30225 = CARTESIAN_POINT ( 'NONE',  ( -83.40544964237400904, -274.5173070286849679, -208.9788751809859377 ) ) ;
#30226 = CARTESIAN_POINT ( 'NONE',  ( -99.40772545839395491, -276.8721704488895625, -315.4312170439667966 ) ) ;
#30227 = CARTESIAN_POINT ( 'NONE',  ( 5.216678999390555127, -58.13084686240627263, -354.5881712518564655 ) ) ;
#30228 = CARTESIAN_POINT ( 'NONE',  ( 36.53642750459122368, -273.3851100515191206, -257.3639452198239610 ) ) ;
#30229 = ADVANCED_FACE ( 'NONE', ( #12679 ), #10777, .T. ) ;
#30230 = CARTESIAN_POINT ( 'NONE',  ( -99.51837872833381482, -297.3835110046858858, -314.8649253165854702 ) ) ;
#30231 = CARTESIAN_POINT ( 'NONE',  ( 156.9186804554042283, 250.2122328390418602, 16.89624193607524205 ) ) ;
#30232 = DIRECTION ( 'NONE',  ( 0.3024135303179485423, 0.9531768234071972268, 0.000000000000000000 ) ) ;
#30233 = CARTESIAN_POINT ( 'NONE',  ( -95.20949855451260646, -286.2634741874908286, -225.3346861841081648 ) ) ;
#30234 = CARTESIAN_POINT ( 'NONE',  ( -67.45883343092104667, -285.2019483794857138, -340.1245202582179559 ) ) ;
#30235 = CARTESIAN_POINT ( 'NONE',  ( 22.07927720021442042, -286.3054152180918663, -227.6959539942548076 ) ) ;
#30236 = CARTESIAN_POINT ( 'NONE',  ( -111.1925598651727825, -276.9486279954259658, -270.6207518743560740 ) ) ;
#30237 = CARTESIAN_POINT ( 'NONE',  ( -111.2262055364654003, -286.5126709601237849, -262.6448169906840917 ) ) ;
#30238 = CARTESIAN_POINT ( 'NONE',  ( -32.90208420742211359, -278.5889754397038018, -196.8016348164179021 ) ) ;
#30239 = CARTESIAN_POINT ( 'NONE',  ( -48.64197946262460448, -278.2789591126079358, -342.8456560869590817 ) ) ;
#30240 = DIRECTION ( 'NONE',  ( -1.000000000000000000, 0.000000000000000000, 0.000000000000000000 ) ) ;
#30241 = CARTESIAN_POINT ( 'NONE',  ( 51.81736995740534013, -299.8487276833988631, -197.2490443897613375 ) ) ;
#30242 = CARTESIAN_POINT ( 'NONE',  ( 37.17215754845398834, -282.1197936335277063, -251.6036172092029233 ) ) ;
#30243 = CARTESIAN_POINT ( 'NONE',  ( 25.06105409695339858, -282.6419452536333097, -315.3881858004331207 ) ) ;
#30244 = VERTEX_POINT ( 'NONE', #83211 ) ;
#30245 = VERTEX_POINT ( 'NONE', #18358 ) ;
#30246 = CARTESIAN_POINT ( 'NONE',  ( 201.2104617360081704, 15.00000000000001243, -10.00000000000000178 ) ) ;
#30247 = CARTESIAN_POINT ( 'NONE',  ( 17.44171303467886602, -288.6844726397104637, -217.9492308230940978 ) ) ;
#30248 = CARTESIAN_POINT ( 'NONE',  ( -112.3875668390121092, -289.0488516162957353, -285.3076532172833026 ) ) ;
#30249 = CARTESIAN_POINT ( 'NONE',  ( -52.65894066684864327, -297.0481588155813597, -198.7690334284515075 ) ) ;
#30250 = CARTESIAN_POINT ( 'NONE',  ( 4.093605395896895871, -291.9429946030872998, -205.5181527295502804 ) ) ;
#30251 = CARTESIAN_POINT ( 'NONE',  ( -0.6630064052688882104, -287.0356768691353295, -334.3368343582113198 ) ) ;
#30252 = CARTESIAN_POINT ( 'NONE',  ( -45.44521468341863368, -287.7315611833651019, -343.5028158608826629 ) ) ;
#30253 = CARTESIAN_POINT ( 'NONE',  ( -42.71844824893391745, -287.1879180690430076, -197.1485528861257990 ) ) ;
#30254 = CARTESIAN_POINT ( 'NONE',  ( -110.1383538744669579, -276.7843817836933340, -252.2627859587048249 ) ) ;
#30255 = CARTESIAN_POINT ( 'NONE',  ( 37.10853860683869954, -289.6740782642317527, -279.8443553187082102 ) ) ;
#30256 = CARTESIAN_POINT ( 'NONE',  ( -0.2090916398011355148, -286.5597075687548454, -335.7743283815552786 ) ) ;
#30257 = CARTESIAN_POINT ( 'NONE',  ( -99.81628277745228672, -286.0194206094087122, -232.0501431294695465 ) ) ;
#30258 = CARTESIAN_POINT ( 'NONE',  ( -111.3709646190213221, -292.7192025155866304, -257.3343598552531262 ) ) ;
#30259 = CARTESIAN_POINT ( 'NONE',  ( 196.8208173705680224, 214.5799893323897152, -12.60277379099805195 ) ) ;
#30260 = CARTESIAN_POINT ( 'NONE',  ( 201.2104617360081704, 250.0000000000000568, 15.00000000000000000 ) ) ;
#30261 = CARTESIAN_POINT ( 'NONE',  ( -36.58377548792454803, -299.9817177801803609, -194.8008643405604232 ) ) ;
#30262 = CARTESIAN_POINT ( 'NONE',  ( -38.34581969193056494, -279.2364166948810862, -197.1941039448001334 ) ) ;
#30263 = CARTESIAN_POINT ( 'NONE',  ( 15.31110376582103783, -280.3087349713057392, -323.8447278044608311 ) ) ;
#30264 = CARTESIAN_POINT ( 'NONE',  ( 38.69363438383049214, -292.6059706856769935, -258.9228752454965274 ) ) ;
#30265 = CARTESIAN_POINT ( 'NONE',  ( -33.74297281102408874, -296.4978057387346553, -196.5621124728592122 ) ) ;
#30266 = CARTESIAN_POINT ( 'NONE',  ( -24.09694663086387223, -274.9616789924215254, -343.6658215369304230 ) ) ;
#30267 = CARTESIAN_POINT ( 'NONE',  ( -90.41350849308709314, -298.5967181987629715, -219.4490461642845673 ) ) ;
#30268 = CYLINDRICAL_SURFACE ( 'NONE', #92709, 0.5000000000000004441 ) ;
#30269 = CARTESIAN_POINT ( 'NONE',  ( -60.67379830528999918, -272.3301244463054900, -197.5445312275051037 ) ) ;
#30270 = CARTESIAN_POINT ( 'NONE',  ( -110.2495387628530779, -294.5193444744269300, -291.8178300790127651 ) ) ;
#30271 = CARTESIAN_POINT ( 'NONE',  ( 33.32101971620121361, -295.2475691219497094, -290.9528583762774474 ) ) ;
#30272 = FACE_OUTER_BOUND ( 'NONE', #74574, .T. ) ;
#30273 = CARTESIAN_POINT ( 'NONE',  ( -7.913995945544356481, -295.4592964853624153, -337.3569028352923738 ) ) ;
#30274 = CIRCLE ( 'NONE', #24236, 7.999999999999992895 ) ;
#30275 = DIRECTION ( 'NONE',  ( -0.000000000000000000, -0.000000000000000000, -1.000000000000000000 ) ) ;
#30277 = CARTESIAN_POINT ( 'NONE',  ( -93.61357235408382849, -297.2115686369666037, -223.8392375785866477 ) ) ;
#30276 = CARTESIAN_POINT ( 'NONE',  ( -63.94246463210787113, -283.7270864277783744, -199.8433109332171682 ) ) ;
#30278 = CARTESIAN_POINT ( 'NONE',  ( -83.88320362439178268, -283.6712409306389304, -331.7704834050782665 ) ) ;
#30279 = CARTESIAN_POINT ( 'NONE',  ( 38.09326361532798444, -283.5382781509355823, -275.5374234817456909 ) ) ;
#30280 = AXIS2_PLACEMENT_3D ( 'NONE', #48260, #40210, #84714 ) ;
#30281 = CARTESIAN_POINT ( 'NONE',  ( -76.09240538327740921, -285.2162828544068134, -203.7856241204926562 ) ) ;
#30282 = CARTESIAN_POINT ( 'NONE',  ( 14.18346396892100891, -290.7778141388332642, -216.0915511023330851 ) ) ;
#30283 = ADVANCED_FACE ( 'NONE', ( #47217 ), #44106, .T. ) ;
#30284 = CARTESIAN_POINT ( 'NONE',  ( -112.9668995883443046, -277.7253469392597935, -284.3669904164597142 ) ) ;
#30285 = EDGE_CURVE ( 'NONE', #77294, #26019, #62313, .T. ) ;
#30286 = CARTESIAN_POINT ( 'NONE',  ( 31.98288692825982693, -278.6237833571633473, -237.0123917617630980 ) ) ;
#30287 = CARTESIAN_POINT ( 'NONE',  ( -48.18343439338453749, -278.5340725472075860, -507.3671153682459476 ) ) ;
#30288 = CARTESIAN_POINT ( 'NONE',  ( 11.40919638131766334, -285.5406086466460351, -215.4249723980004774 ) ) ;
#30289 = CARTESIAN_POINT ( 'NONE',  ( -103.5385905743978299, -288.9652926162976883, -309.1891042702944219 ) ) ;
#30290 = DIRECTION ( 'NONE',  ( -1.000000000000000000, 0.000000000000000000, 0.000000000000000000 ) ) ;
#30291 = CARTESIAN_POINT ( 'NONE',  ( -113.4586770934678981, -280.0690816424614695, -263.0882024961543380 ) ) ;
#30293 = CARTESIAN_POINT ( 'NONE',  ( 31.37305291535080798, -281.5495801154356172, -295.2162674044034247 ) ) ;
#30292 = CARTESIAN_POINT ( 'NONE',  ( 20.99690167611707992, -292.2267308071288880, -318.0784761412790544 ) ) ;
#30294 = CARTESIAN_POINT ( 'NONE',  ( -27.74572995558257205, -295.1003075988508044, -346.8141314721231083 ) ) ;
#30295 = CARTESIAN_POINT ( 'NONE',  ( -0.3984978190463963066, -284.6190928866167269, -204.4334220869432386 ) ) ;
#30296 = CARTESIAN_POINT ( 'NONE',  ( -81.09334692990802296, -281.4579206211412838, -209.4448307667076392 ) ) ;
#30297 = EDGE_CURVE ( 'NONE', #12355, #5766, #71369, .T. ) ;
#30298 = CARTESIAN_POINT ( 'NONE',  ( -84.63917256563671287, -294.7810418449220151, -326.3415515476017958 ) ) ;
#30299 = CARTESIAN_POINT ( 'NONE',  ( -21.02729779183863457, -296.2562167332568492, -195.3666715009129291 ) ) ;
#30300 = ORIENTED_EDGE ( 'NONE', *, *, #80845, .T. ) ;
#30301 = CARTESIAN_POINT ( 'NONE',  ( 200.5815643859949944, 65.97596549932491428, -9.780880230328994784 ) ) ;
#30302 = CARTESIAN_POINT ( 'NONE',  ( 20.08572133293977302, -282.8704095424396883, -222.6554623309425835 ) ) ;
#30303 = CARTESIAN_POINT ( 'NONE',  ( -82.40268784573207483, -295.1938603393234075, -327.9364573860551673 ) ) ;
#30304 = CARTESIAN_POINT ( 'NONE',  ( -4.771743288812454686, -277.9809262143061233, -202.8022627189028810 ) ) ;
#30305 = CARTESIAN_POINT ( 'NONE',  ( 15.92247725145063164, -273.9813353613054687, -214.9798374967508039 ) ) ;
#30306 = CARTESIAN_POINT ( 'NONE',  ( -94.95187638088701476, -289.7535825356361556, -315.2150918889023501 ) ) ;
#30307 = CARTESIAN_POINT ( 'NONE',  ( -35.66626166038895462, -281.5936407158752104, -196.6743094552464584 ) ) ;
#30308 = CARTESIAN_POINT ( 'NONE',  ( -36.74990220974716948, -275.6598393021289439, -196.5509373181357944 ) ) ;
#30309 = CARTESIAN_POINT ( 'NONE',  ( -63.61684283494066250, -284.9891515630255867, -341.8877374373977887 ) ) ;
#30310 = CARTESIAN_POINT ( 'NONE',  ( -46.49082093992373643, -278.7285195091731680, -197.4851269918347327 ) ) ;
#30311 = CARTESIAN_POINT ( 'NONE',  ( -2.927673812715636537, -278.5974601240934021, -336.9995111557383893 ) ) ;
#30312 = EDGE_LOOP ( 'NONE', ( #42417, #79238, #20796, #16453 ) ) ;
#30313 = CARTESIAN_POINT ( 'NONE',  ( -92.16757407084827491, -273.1281190401284107, -216.2951994116943979 ) ) ;
#30314 = CARTESIAN_POINT ( 'NONE',  ( -103.7041911062083415, -292.9227972320578033, -236.5225566655315959 ) ) ;
#30315 = DIRECTION ( 'NONE',  ( -1.000000000000000000, -0.000000000000000000, -0.000000000000000000 ) ) ;
#30316 = CARTESIAN_POINT ( 'NONE',  ( 196.8803347170859865, 250.0000000000000568, 12.49999999999999289 ) ) ;
#30317 = CARTESIAN_POINT ( 'NONE',  ( 20.41049706642102635, -292.3636173436287322, -319.4018072343007475 ) ) ;
#30318 = CARTESIAN_POINT ( 'NONE',  ( -29.97743445099836990, -273.6555251594185734, -197.6716687297717669 ) ) ;
#30319 = CARTESIAN_POINT ( 'NONE',  ( 195.4781563537916043, 32.98517505407394168, 13.99999999999999822 ) ) ;
#30320 = CARTESIAN_POINT ( 'NONE',  ( -3.645126016569865346, -294.0088408306101542, -201.8832293386361982 ) ) ;
#30322 = CARTESIAN_POINT ( 'NONE',  ( -39.21743087396442462, -293.2342056103323671, -193.7681896800372954 ) ) ;
#30321 = CARTESIAN_POINT ( 'NONE',  ( 31.95455697924148097, -277.6233781216988064, -236.9535640164627637 ) ) ;
#30323 = CARTESIAN_POINT ( 'NONE',  ( -10.10587582712289390, -288.4086670888771096, -200.6461907207715001 ) ) ;
#30324 = CARTESIAN_POINT ( 'NONE',  ( 36.17933434339929732, -273.3724385954732270, -256.4081283615719826 ) ) ;
#30325 = CARTESIAN_POINT ( 'NONE',  ( 32.62343200360369622, -277.8062046725396499, -295.9314017754524002 ) ) ;
#30326 = CARTESIAN_POINT ( 'NONE',  ( -31.51353581329227538, -293.0579784533805423, -344.6237197267218448 ) ) ;
#30327 = CARTESIAN_POINT ( 'NONE',  ( -106.3048038756326434, -280.8215654241241737, -238.8596333688762741 ) ) ;
#30328 = VERTEX_POINT ( 'NONE', #58098 ) ;
#30329 = CARTESIAN_POINT ( 'NONE',  ( -48.33605347603156588, -282.8626682788591324, -342.5498406556216082 ) ) ;
#30330 = CARTESIAN_POINT ( 'NONE',  ( -42.42335529951948558, -281.0691395003895536, -193.8387729409524525 ) ) ;
#30331 = CARTESIAN_POINT ( 'NONE',  ( -63.78939666134351683, -282.1843998303464218, -342.2535937109928454 ) ) ;
#30332 = CARTESIAN_POINT ( 'NONE',  ( -22.97115700840193497, -277.8140107069497731, -345.8227490489386469 ) ) ;
#30333 = CARTESIAN_POINT ( 'NONE',  ( 35.83413559433095230, -277.3466603205235970, -292.0406781009871793 ) ) ;
#30334 = CIRCLE ( 'NONE', #83245, 6.654241149514406040 ) ;
#30335 = CARTESIAN_POINT ( 'NONE',  ( -21.39648532958013050, -288.7662352645559167, -200.3538533559491555 ) ) ;
#30336 = ORIENTED_EDGE ( 'NONE', *, *, #1737, .T. ) ;
#30337 = CARTESIAN_POINT ( 'NONE',  ( -111.0149742419033601, -298.7335213469509085, -256.2480504441812172 ) ) ;
#30338 = AXIS2_PLACEMENT_3D ( 'NONE', #81171, #66519, #53703 ) ;
#30339 = CARTESIAN_POINT ( 'NONE',  ( -55.10048773536283306, -292.8980161745895998, -199.2355140457789844 ) ) ;
#30340 = CARTESIAN_POINT ( 'NONE',  ( -81.81920467862833846, -275.6815405491170736, -330.3077474851269812 ) ) ;
#30341 = CARTESIAN_POINT ( 'NONE',  ( -31.87697628902859392, -290.7443628320071980, -346.2028942339384230 ) ) ;
#30342 = CARTESIAN_POINT ( 'NONE',  ( -70.25919855877152997, -290.9549519717219823, -205.0899071343594073 ) ) ;
#30343 = CARTESIAN_POINT ( 'NONE',  ( 39.54250020041620672, -287.1106828574784231, -274.4259407631919885 ) ) ;
#30344 = CARTESIAN_POINT ( 'NONE',  ( 175.2296996224750103, 249.5000000000000568, 0.000000000000000000 ) ) ;
#30345 = CARTESIAN_POINT ( 'NONE',  ( -107.7551894163143942, -282.6622909905218535, -292.4604605435873736 ) ) ;
#30346 = CARTESIAN_POINT ( 'NONE',  ( -102.7199382873946831, -291.9397190867373411, -305.6346748019720962 ) ) ;
#30347 = CARTESIAN_POINT ( 'NONE',  ( -105.8657154033121230, -282.6711072155442821, -297.6140826549684562 ) ) ;
#30348 = CARTESIAN_POINT ( 'NONE',  ( -37.02288509367984659, -281.3714029382598483, -196.8686568953267226 ) ) ;
#30349 = ORIENTED_EDGE ( 'NONE', *, *, #76250, .F. ) ;
#30350 = CARTESIAN_POINT ( 'NONE',  ( -41.73507411098987063, -290.0474468415446267, -347.0131833871716367 ) ) ;
#30351 = CARTESIAN_POINT ( 'NONE',  ( -104.5010969102864209, -279.4306298667779060, -241.5930129818785588 ) ) ;
#30352 = CARTESIAN_POINT ( 'NONE',  ( -56.07674356019526130, -290.6111059782531925, -196.0298997386839517 ) ) ;
#30353 = CARTESIAN_POINT ( 'NONE',  ( -4.851538190235796577, -287.2720583852579921, -200.7296007040601751 ) ) ;
#30354 = CARTESIAN_POINT ( 'NONE',  ( 31.36402371041186043, -287.5985563649752521, -235.7338106242785614 ) ) ;
#30355 = CARTESIAN_POINT ( 'NONE',  ( -73.55747563525513044, -285.7238955599361816, -206.9635197812090155 ) ) ;
#30356 = ORIENTED_EDGE ( 'NONE', *, *, #22221, .F. ) ;
#30357 = DIRECTION ( 'NONE',  ( 0.000000000000000000, 1.000000000000000000, 0.000000000000000000 ) ) ;
#30358 = CARTESIAN_POINT ( 'NONE',  ( -2.642990226368007178, -294.3663695353113212, -202.9944820103840470 ) ) ;
#30359 = CARTESIAN_POINT ( 'NONE',  ( -19.41916274868404457, -293.5112345375185896, -344.7936092943125459 ) ) ;
#30360 = CARTESIAN_POINT ( 'NONE',  ( 0.9843800942212024285, -275.5861474456087876, -332.8267897707962675 ) ) ;
#30361 = CARTESIAN_POINT ( 'NONE',  ( -29.06492020340282778, -297.5018191483918599, -193.4639370183433016 ) ) ;
#30362 = CARTESIAN_POINT ( 'NONE',  ( 35.40143388415661718, -291.8768489228952490, -258.4861426334520047 ) ) ;
#30363 = CARTESIAN_POINT ( 'NONE',  ( -82.54553853620640780, -295.6652607265676806, -211.6908282022216952 ) ) ;
#30364 = CARTESIAN_POINT ( 'NONE',  ( -103.9229279011404117, -292.1719071713685594, -239.4730845091687002 ) ) ;
#30365 = CARTESIAN_POINT ( 'NONE',  ( 35.21170535592063544, -294.4939126146782087, -259.8620977229191453 ) ) ;
#30366 = PLANE ( 'NONE',  #82258 ) ;
#30367 = CARTESIAN_POINT ( 'NONE',  ( 29.26571745237979982, -292.0124013390278037, -305.1961627919250759 ) ) ;
#30368 = CARTESIAN_POINT ( 'NONE',  ( -111.4943479972778277, -298.7009193367680382, -258.7873342821916935 ) ) ;
#30369 = CARTESIAN_POINT ( 'NONE',  ( -109.5107109708226574, -291.6609480034854300, -257.6197056666317735 ) ) ;
#30370 = CARTESIAN_POINT ( 'NONE',  ( -39.68546534238544865, -295.4156426965833475, -343.3570724978961266 ) ) ;
#30371 = CARTESIAN_POINT ( 'NONE',  ( -96.61908903814438077, -279.8964643142735440, -316.8863581359638033 ) ) ;
#30372 = CARTESIAN_POINT ( 'NONE',  ( -105.7272149595642077, -277.6824318132854614, -235.9398308455830318 ) ) ;
#30373 = ORIENTED_EDGE ( 'NONE', *, *, #47352, .F. ) ;
#30374 = CARTESIAN_POINT ( 'NONE',  ( -55.30175408553317595, -273.1755397483860861, -195.5898049800782417 ) ) ;
#30375 = CARTESIAN_POINT ( 'NONE',  ( 19.07149728193752836, -278.9535283398895444, -221.7733912578554225 ) ) ;
#30376 = CARTESIAN_POINT ( 'NONE',  ( -113.2836809559127715, -276.8651125563465598, -277.2383869981181306 ) ) ;
#30377 = CARTESIAN_POINT ( 'NONE',  ( -109.9532474719436692, -276.8018089361800094, -250.8797735318345019 ) ) ;
#30378 = CARTESIAN_POINT ( 'NONE',  ( -36.45929366230426893, -296.7482493882942549, -196.8681658811741215 ) ) ;
#30379 = CARTESIAN_POINT ( 'NONE',  ( 195.5881128153457098, 15.36528803885690664, 22.50000000000000000 ) ) ;
#30380 = DIRECTION ( 'NONE',  ( 1.000000000000000000, 0.000000000000000000, 0.000000000000000000 ) ) ;
#30381 = CARTESIAN_POINT ( 'NONE',  ( -78.67078869881135006, -289.5190210015192065, -207.2883347966385941 ) ) ;
#30382 = CARTESIAN_POINT ( 'NONE',  ( -100.6805982995358590, -289.9739069087532357, -314.1467774891395379 ) ) ;
#30383 = CARTESIAN_POINT ( 'NONE',  ( -34.20579486126489144, -276.0916655262454356, -195.2598894506807596 ) ) ;
#30384 = CARTESIAN_POINT ( 'NONE',  ( -86.60518985941068593, -271.3678742410480709, -213.7400918087003276 ) ) ;
#30385 = EDGE_CURVE ( 'NONE', #80198, #57275, #48641, .T. ) ;
#30386 = CARTESIAN_POINT ( 'NONE',  ( -47.24569550462377521, -282.3721204272555383, -346.5586881259623055 ) ) ;
#30387 = EDGE_CURVE ( 'NONE', #1567, #84679, #60972, .T. ) ;
#30388 = DIRECTION ( 'NONE',  ( 0.000000000000000000, 0.000000000000000000, -1.000000000000000000 ) ) ;
#30389 = CARTESIAN_POINT ( 'NONE',  ( -68.76226250186361710, -281.4649774995575626, -338.4759357310989003 ) ) ;
#30390 = DIRECTION ( 'NONE',  ( -1.000000000000000000, -0.000000000000000000, 0.000000000000000000 ) ) ;
#30391 = CARTESIAN_POINT ( 'NONE',  ( 34.03750243871256487, -292.1221611069201458, -253.2152750703466211 ) ) ;
#30392 = CARTESIAN_POINT ( 'NONE',  ( -103.3256569276116608, -283.1464602072390448, -236.3466663095536830 ) ) ;
#30393 = CARTESIAN_POINT ( 'NONE',  ( 160.5350683151633291, 250.0000000000000568, 15.22542485937381329 ) ) ;
#30394 = DIRECTION ( 'NONE',  ( 0.000000000000000000, 0.000000000000000000, -1.000000000000000000 ) ) ;
#30395 = CARTESIAN_POINT ( 'NONE',  ( 35.04037714199228759, -291.8051198903942236, -290.0525820121833362 ) ) ;
#30396 = CARTESIAN_POINT ( 'NONE',  ( -102.5544251687881285, -279.6867336996780864, -304.9116737804314425 ) ) ;
#30397 = CARTESIAN_POINT ( 'NONE',  ( 6.709278043402101765, -283.6731277203155628, -333.0959205434032242 ) ) ;
#30399 = CARTESIAN_POINT ( 'NONE',  ( -30.53128379256239811, -286.1405258354367902, -197.6286971215307915 ) ) ;
#30398 = CARTESIAN_POINT ( 'NONE',  ( -89.15725053474784545, -271.4104081430577935, -215.2945728974029862 ) ) ;
#30400 = CARTESIAN_POINT ( 'NONE',  ( 33.81656149352531315, -277.2231388504179108, -289.1194953492233140 ) ) ;
#30401 = CARTESIAN_POINT ( 'NONE',  ( -6.198624515589422401, -277.4349988267793492, -336.5769615598744053 ) ) ;
#30402 = CARTESIAN_POINT ( 'NONE',  ( -84.28153266069087124, -287.4065314959399302, -211.8662227571742847 ) ) ;
#30403 = ORIENTED_EDGE ( 'NONE', *, *, #48446, .F. ) ;
#30404 = LINE ( 'NONE', #16202, #63432 ) ;
#30405 = CARTESIAN_POINT ( 'NONE',  ( -104.6039383322747511, -295.8983334081426619, -307.9506680985916773 ) ) ;
#30407 = CARTESIAN_POINT ( 'NONE',  ( 34.97595073988657077, -289.2927182412562388, -251.8162419054780798 ) ) ;
#30406 = CIRCLE ( 'NONE', #54592, 6.286090667950827715 ) ;
#30408 = DIRECTION ( 'NONE',  ( 1.000000000000000000, 0.000000000000000000, 0.000000000000000000 ) ) ;
#30409 = CARTESIAN_POINT ( 'NONE',  ( 13.84574458161073807, -290.1952119285918457, -206.2264541496106460 ) ) ;
#30410 = CARTESIAN_POINT ( 'NONE',  ( -112.4121188193232967, -277.6701916319069596, -254.6158561427491236 ) ) ;
#30411 = CARTESIAN_POINT ( 'NONE',  ( -44.79826888974096732, -290.3592740396309750, -194.4744527159748486 ) ) ;
#30412 = CARTESIAN_POINT ( 'NONE',  ( -107.6415148815863745, -285.7820378585417416, -292.4664069034336649 ) ) ;
#30413 = CARTESIAN_POINT ( 'NONE',  ( -62.67659069883896450, -281.4781417358979638, -200.7648144946293769 ) ) ;
#30414 = CARTESIAN_POINT ( 'NONE',  ( 38.76222251870924396, -289.0636382209721660, -277.2021156870180789 ) ) ;
#30415 = CARTESIAN_POINT ( 'NONE',  ( -6.405871439189798622, -284.6460189565929682, -338.6977914707035779 ) ) ;
#30416 = CARTESIAN_POINT ( 'NONE',  ( 5.873036110653372610, -276.6503655297937598, -334.0909114570975476 ) ) ;
#30417 = CARTESIAN_POINT ( 'NONE',  ( -112.0163699347023254, -270.6241775036895660, -264.7512697947053653 ) ) ;
#30418 = CARTESIAN_POINT ( 'NONE',  ( -31.07164192017774695, -279.9624873919271408, -193.5641351461285069 ) ) ;
#30419 = CARTESIAN_POINT ( 'NONE',  ( -110.4647240449685768, -298.6535278541505818, -256.3526129439659371 ) ) ;
#30420 = CARTESIAN_POINT ( 'NONE',  ( 158.3977298502311157, 17.52828139914342032, 10.67961748034988823 ) ) ;
#30421 = FACE_OUTER_BOUND ( 'NONE', #34325, .T. ) ;
#30422 = CARTESIAN_POINT ( 'NONE',  ( -101.8468313567045271, -271.3244763921799745, -230.1981741443804026 ) ) ;
#30423 = CARTESIAN_POINT ( 'NONE',  ( 160.5350683151633291, 275.5000000000000568, 12.00000000000000000 ) ) ;
#30424 = CARTESIAN_POINT ( 'NONE',  ( -24.85971845886106379, -279.7233467573310008, -198.3736984212217749 ) ) ;
#30425 = CARTESIAN_POINT ( 'NONE',  ( -1.639118197081272932, -277.7946757131378490, -338.1352602714663931 ) ) ;
#30426 = CARTESIAN_POINT ( 'NONE',  ( -88.17472866643004181, -282.8018551907403548, -327.9544767035242785 ) ) ;
#30427 = CARTESIAN_POINT ( 'NONE',  ( -80.98723948211757317, -291.4137133836126168, -330.1997979591640728 ) ) ;
#30428 = CARTESIAN_POINT ( 'NONE',  ( 75.09555894462938852, -300.9558628955291510, -194.0259358155473137 ) ) ;
#30429 = CARTESIAN_POINT ( 'NONE',  ( -84.98152943331974996, -298.6163183540284649, -210.3739911866694854 ) ) ;
#30430 = CARTESIAN_POINT ( 'NONE',  ( -9.057584995526280380, -294.4228991617147813, -201.0236906152386211 ) ) ;
#30431 = CARTESIAN_POINT ( 'NONE',  ( 29.78460333268899163, -279.9906237201117278, -303.5556337500761970 ) ) ;
#30432 = CARTESIAN_POINT ( 'NONE',  ( -45.77886591144952888, -285.0799528569187373, -344.3734333045267704 ) ) ;
#30433 = CARTESIAN_POINT ( 'NONE',  ( 6.155220129386226091, -272.6653827330829927, -209.6353294603123345 ) ) ;
#30434 = CARTESIAN_POINT ( 'NONE',  ( -92.83481871751310166, -285.4318179921757519, -322.6004883283499680 ) ) ;
#30435 = CARTESIAN_POINT ( 'NONE',  ( -99.10958497953167523, -288.9286563528490888, -309.8447155189901991 ) ) ;
#30436 = CARTESIAN_POINT ( 'NONE',  ( -82.85074041547900947, -220.2000674996521354, -352.4970221947974665 ) ) ;
#30437 = ORIENTED_EDGE ( 'NONE', *, *, #73694, .F. ) ;
#30438 = CARTESIAN_POINT ( 'NONE',  ( -26.24817011758402785, -287.4883069314020076, -345.9623076794937333 ) ) ;
#30439 = CARTESIAN_POINT ( 'NONE',  ( 33.10117376977922277, -287.4751140013740951, -289.7812115690613268 ) ) ;
#30440 = ORIENTED_EDGE ( 'NONE', *, *, #1762, .F. ) ;
#30441 = CARTESIAN_POINT ( 'NONE',  ( -89.68535264957019137, -286.4144764689514773, -214.2385915595882011 ) ) ;
#30442 = CARTESIAN_POINT ( 'NONE',  ( 32.91936102392261176, -276.1488043543715207, -290.2933326828679128 ) ) ;
#30443 = CARTESIAN_POINT ( 'NONE',  ( 38.92812623901128433, -292.5793810875981080, -278.8742696593846517 ) ) ;
#30444 = CARTESIAN_POINT ( 'NONE',  ( -13.44572669270460352, -283.4012094180182544, -343.4521245425622169 ) ) ;
#30445 = CARTESIAN_POINT ( 'NONE',  ( 23.18541798193011161, -282.4465372654044586, -223.8728473738814273 ) ) ;
#30446 = CARTESIAN_POINT ( 'NONE',  ( -38.72790996317126400, -283.4023727350203785, -347.3274918995299458 ) ) ;
#30447 = CARTESIAN_POINT ( 'NONE',  ( 17.97777056028917642, -281.2065993437755083, -222.6780642741602492 ) ) ;
#30448 = CARTESIAN_POINT ( 'NONE',  ( 31.95455697924147032, -273.4809262143061233, -303.7686719486574702 ) ) ;
#30449 = CARTESIAN_POINT ( 'NONE',  ( 203.9605228849236482, 295.7236489450776276, -54.00000000003888800 ) ) ;
#30450 = ORIENTED_EDGE ( 'NONE', *, *, #56743, .T. ) ;
#30451 = CARTESIAN_POINT ( 'NONE',  ( -111.7234250678460654, -280.4408017313708115, -279.0267913573229634 ) ) ;
#30452 = CARTESIAN_POINT ( 'NONE',  ( -100.4790452129269056, -247.5007079388412308, -333.8973734642195836 ) ) ;
#30453 = CARTESIAN_POINT ( 'NONE',  ( -110.2015576158204340, -295.8145898646614569, -276.9005189072779558 ) ) ;
#30454 = CARTESIAN_POINT ( 'NONE',  ( 34.39185194042086380, -293.4125140408897323, -298.1788175771407055 ) ) ;
#30455 = CARTESIAN_POINT ( 'NONE',  ( 45.91229879770529010, 10.79500447405072805, -328.5722265923597547 ) ) ;
#30457 = CARTESIAN_POINT ( 'NONE',  ( -109.9698033400114667, -288.7810882537460770, -283.4606996652667590 ) ) ;
#30456 = CARTESIAN_POINT ( 'NONE',  ( 30.15906987437215747, -297.4563395728868613, -193.9663099215189277 ) ) ;
#30458 = CARTESIAN_POINT ( 'NONE',  ( -17.87414766398960353, -296.6588708410381514, -341.9982583410604775 ) ) ;
#30459 = CARTESIAN_POINT ( 'NONE',  ( -35.94074817589108051, -287.3852644276557271, -196.8813193094359519 ) ) ;
#30460 = ORIENTED_EDGE ( 'NONE', *, *, #91412, .F. ) ;
#30461 = CARTESIAN_POINT ( 'NONE',  ( -81.72585949647205439, -296.5811827581291595, -333.0588267331919496 ) ) ;
#30462 = CARTESIAN_POINT ( 'NONE',  ( -83.69174465666141316, -285.8886752022341398, -213.8182881602106420 ) ) ;
#30463 = CARTESIAN_POINT ( 'NONE',  ( -101.2101093160071628, -295.9065951526369531, -228.0426177672065933 ) ) ;
#30464 = CARTESIAN_POINT ( 'NONE',  ( 30.75107741266623407, -293.8933821237206416, -234.6441807233576071 ) ) ;
#30465 = CARTESIAN_POINT ( 'NONE',  ( 38.75660446740547371, -294.1864219334160566, -281.7002070524073361 ) ) ;
#30466 = CARTESIAN_POINT ( 'NONE',  ( -38.89970730370525587, -292.1987465311190704, -197.3777457792164398 ) ) ;
#30467 = ORIENTED_EDGE ( 'NONE', *, *, #4102, .F. ) ;
#30468 = CARTESIAN_POINT ( 'NONE',  ( 157.4642333713238429, 15.57755555264427372, 7.027845929950953696 ) ) ;
#30469 = CARTESIAN_POINT ( 'NONE',  ( -82.73489902193460921, -275.3576544430699187, -209.8905535330964369 ) ) ;
#30470 = CARTESIAN_POINT ( 'NONE',  ( 34.35553623104942744, -274.0040781353523585, -243.3886316995457832 ) ) ;
#30471 = ORIENTED_EDGE ( 'NONE', *, *, #57376, .T. ) ;
#30472 = CARTESIAN_POINT ( 'NONE',  ( -56.91443260001816640, -276.8055402548901043, -344.8233523562348637 ) ) ;
#30473 = CARTESIAN_POINT ( 'NONE',  ( -76.97689540850997503, -271.9112837363510380, -208.1076706127692262 ) ) ;
#30474 = CARTESIAN_POINT ( 'NONE',  ( -100.5313930023285423, -280.9419870073729157, -231.3024050871305803 ) ) ;
#30475 = CARTESIAN_POINT ( 'NONE',  ( 1.497822823686025151, -274.6671316817748334, -333.6856919576097198 ) ) ;
#30476 = CARTESIAN_POINT ( 'NONE',  ( -32.68507366591525454, -275.1918596435633049, -197.1874703555207589 ) ) ;
#30477 = CARTESIAN_POINT ( 'NONE',  ( -27.26964137307360403, -275.1244160056850774, -197.7706730866786415 ) ) ;
#30478 = CARTESIAN_POINT ( 'NONE',  ( -68.44999301935921210, -275.4091918870223594, -201.0198003886684432 ) ) ;
#30479 = CIRCLE ( 'NONE', #39499, 25.00000000000000355 ) ;
#30480 = CARTESIAN_POINT ( 'NONE',  ( -4.519241728081113685, -272.5025538490259009, -202.5155593285977602 ) ) ;
#30481 = CARTESIAN_POINT ( 'NONE',  ( -31.58606522462891064, -295.6291308313591912, -343.2862990823888936 ) ) ;
#30482 = CARTESIAN_POINT ( 'NONE',  ( 23.40924315264309996, -292.7012009180888299, -311.9796788935318546 ) ) ;
#30483 = DIRECTION ( 'NONE',  ( 0.000000000000000000, 0.000000000000000000, -1.000000000000000000 ) ) ;
#30484 = CARTESIAN_POINT ( 'NONE',  ( -7.902378773659134659, -277.1689944546349125, -341.4588164389803069 ) ) ;
#30485 = CARTESIAN_POINT ( 'NONE',  ( 11.54494825625091003, -274.9194325188312291, -216.0796290706797720 ) ) ;
#30486 = AXIS2_PLACEMENT_3D ( 'NONE', #15960, #87891, #37257 ) ;
#30487 = CARTESIAN_POINT ( 'NONE',  ( -73.36590380457026583, -284.2697656324123727, -202.8075956466740593 ) ) ;
#30488 = CARTESIAN_POINT ( 'NONE',  ( -101.5363140113149427, -298.0292207621320131, -309.4645701748207784 ) ) ;
#30489 = DIRECTION ( 'NONE',  ( 0.000000000000000000, 0.000000000000000000, 1.000000000000000000 ) ) ;
#30490 = CARTESIAN_POINT ( 'NONE',  ( -35.92010057779749843, -285.2676005305355034, -197.2134537533384844 ) ) ;
#30491 = CARTESIAN_POINT ( 'NONE',  ( -105.3578026010893609, -282.1321585602598248, -302.3585901925954431 ) ) ;
#30492 = EDGE_CURVE ( 'NONE', #51697, #17995, #6033, .T. ) ;
#30493 = CARTESIAN_POINT ( 'NONE',  ( -109.8759070710191708, -276.9843959021232536, -255.5747007600660083 ) ) ;
#30494 = CARTESIAN_POINT ( 'NONE',  ( -89.51628850626474332, -276.3795230077192286, -322.3294240728554314 ) ) ;
#30495 = CARTESIAN_POINT ( 'NONE',  ( -70.86702211693705067, -281.6100788549769049, -203.2572118609458300 ) ) ;
#30496 = CARTESIAN_POINT ( 'NONE',  ( -24.54219316581306387, -275.4240896212223220, -198.0368277259416914 ) ) ;
#30497 = CARTESIAN_POINT ( 'NONE',  ( 154.3120505024572822, 19.86534941647866859, 13.70129228612852046 ) ) ;
#30498 = CARTESIAN_POINT ( 'NONE',  ( 5.405478655831243096, -274.8838416653731542, -333.4413773346328185 ) ) ;
#30499 = CARTESIAN_POINT ( 'NONE',  ( -42.33433592278263546, -281.9894799696330665, -195.3604378836142814 ) ) ;
#30500 = EDGE_CURVE ( 'NONE', #90630, #60346, #84939, .T. ) ;
#30501 = CARTESIAN_POINT ( 'NONE',  ( 25.91854806279937051, -288.9190693780342940, -229.0397530928516687 ) ) ;
#30502 = CARTESIAN_POINT ( 'NONE',  ( -85.62563434231992687, -289.3844032141742559, -212.9036990776084508 ) ) ;
#30503 = CARTESIAN_POINT ( 'NONE',  ( 82.12659874290375228, -301.3026828166021005, -196.3296339295530970 ) ) ;
#30504 = CARTESIAN_POINT ( 'NONE',  ( -63.20509443755166501, -296.5026560326310801, -201.6180862338164559 ) ) ;
#30505 = CARTESIAN_POINT ( 'NONE',  ( -67.03677985120376093, -289.7982920927141208, -202.3238655200340190 ) ) ;
#30506 = CARTESIAN_POINT ( 'NONE',  ( -69.18520112214993389, -196.4157418647702968, -356.4528236438462159 ) ) ;
#30507 = CARTESIAN_POINT ( 'NONE',  ( -33.66483702006775758, -296.0980222675469236, -195.3623628324206720 ) ) ;
#30508 = CARTESIAN_POINT ( 'NONE',  ( 20.03863762098110612, -286.7189686795621242, -320.6819355527725293 ) ) ;
#30509 = CARTESIAN_POINT ( 'NONE',  ( -82.65341198582420645, -283.6826963595871121, -209.2969704488729690 ) ) ;
#30510 = CARTESIAN_POINT ( 'NONE',  ( -93.43983699933268383, -291.2150775458806038, -223.6297309859413076 ) ) ;
#30511 = CARTESIAN_POINT ( 'NONE',  ( -1.696433660081715589, -281.9596978592288679, -205.9810752961918467 ) ) ;
#30512 = CARTESIAN_POINT ( 'NONE',  ( 24.27194010876372232, -282.9006366957029854, -309.9050119520894100 ) ) ;
#30513 = CARTESIAN_POINT ( 'NONE',  ( -23.58687808666093133, -290.8572269395274361, -344.5032935005667127 ) ) ;
#30514 = CARTESIAN_POINT ( 'NONE',  ( -20.51205453730430506, -298.4240907695532883, -193.3606552284116447 ) ) ;
#30515 = ORIENTED_EDGE ( 'NONE', *, *, #5090, .T. ) ;
#30516 = CARTESIAN_POINT ( 'NONE',  ( -37.52314650251574335, -287.1342226138090723, -345.9337310671166961 ) ) ;
#30517 = CARTESIAN_POINT ( 'NONE',  ( 18.08959704142943536, -274.8196701557970982, -216.8395478004464394 ) ) ;
#30518 = CARTESIAN_POINT ( 'NONE',  ( -55.43490633500003639, -293.7980920746240372, -197.9423173243462202 ) ) ;
#30519 = CARTESIAN_POINT ( 'NONE',  ( 31.95455697924148097, -283.6233781216988064, -236.9535640164627637 ) ) ;
#30520 = CARTESIAN_POINT ( 'NONE',  ( -109.6831941416651546, -276.2899097184970856, -290.7752472119889831 ) ) ;
#30521 = CARTESIAN_POINT ( 'NONE',  ( 209.2537080094121222, 37.08901624725314150, 12.07126757350762603 ) ) ;
#30522 = CARTESIAN_POINT ( 'NONE',  ( -46.01834168528773006, -296.3437288632409263, -194.6567171476825706 ) ) ;
#30523 = CARTESIAN_POINT ( 'NONE',  ( -7.473583189580038422, -275.9984385935695173, -337.0828405250173319 ) ) ;
#30524 = CARTESIAN_POINT ( 'NONE',  ( -97.33699196483640037, -292.6655310050574030, -227.4814019588066287 ) ) ;
#30525 = CARTESIAN_POINT ( 'NONE',  ( -67.91029542570618105, -292.5820101981540802, -203.7968353009282225 ) ) ;
#30526 = CARTESIAN_POINT ( 'NONE',  ( -98.35515923680057426, -285.7359820032201014, -312.3470846972257391 ) ) ;
#30527 = CARTESIAN_POINT ( 'NONE',  ( -7.437659946947347223, -293.8618978812461933, -200.0308022223674698 ) ) ;
#30528 = CARTESIAN_POINT ( 'NONE',  ( 36.98493142505181197, -295.0962454731146067, -288.5502107766479867 ) ) ;
#30529 = CARTESIAN_POINT ( 'NONE',  ( 33.11614360142508673, -293.6383040233006909, -289.5055582190390737 ) ) ;
#30530 = CARTESIAN_POINT ( 'NONE',  ( 13.53060632349753512, -290.3405140215845108, -325.5407773122331605 ) ) ;
#30531 = CARTESIAN_POINT ( 'NONE',  ( 26.72306369832012862, -282.2810918312300714, -313.0776960333909074 ) ) ;
#30532 = CARTESIAN_POINT ( 'NONE',  ( -35.83875488410073729, -296.1506787407711272, -194.8015972003060483 ) ) ;
#30533 = CARTESIAN_POINT ( 'NONE',  ( -107.9252799729639065, -284.7792795768385758, -239.4551215901402372 ) ) ;
#30534 = CARTESIAN_POINT ( 'NONE',  ( -32.28449278934082400, -278.9680935930981036, -344.8855031816040082 ) ) ;
#30535 = CARTESIAN_POINT ( 'NONE',  ( -67.69798870585597683, -284.4395894940728340, -203.5357766086774802 ) ) ;
#30536 = CARTESIAN_POINT ( 'NONE',  ( 23.10682512407102962, -284.9465971018651089, -225.9654374940808736 ) ) ;
#30537 = CARTESIAN_POINT ( 'NONE',  ( -110.8811787135462765, -276.9241037098828428, -252.0802173014898244 ) ) ;
#30539 = AXIS2_PLACEMENT_3D ( 'NONE', #62399, #33492, #25917 ) ;
#30538 = DIRECTION ( 'NONE',  ( -0.000000000000000000, -1.000000000000000000, -0.000000000000000000 ) ) ;
#30540 = CARTESIAN_POINT ( 'NONE',  ( -110.1576119294400655, -283.9809041161320238, -276.3470540060191638 ) ) ;
#30541 = VECTOR ( 'NONE', #39321, 1000.000000000000000 ) ;
#30542 = CARTESIAN_POINT ( 'NONE',  ( 24.79424682355846343, -283.3545586488428967, -315.1844259333581704 ) ) ;
#30543 = CARTESIAN_POINT ( 'NONE',  ( -31.85559806373210989, -288.0434055663845925, -346.9819331810597873 ) ) ;
#30544 = EDGE_CURVE ( 'NONE', #51410, #47679, #36554, .T. ) ;
#30545 = CARTESIAN_POINT ( 'NONE',  ( -74.92371665531206304, -279.1441543564675953, -336.6486164233569980 ) ) ;
#30546 = CARTESIAN_POINT ( 'NONE',  ( -64.90168910481790476, -278.7197524321436504, -341.7875168366178400 ) ) ;
#30547 = CARTESIAN_POINT ( 'NONE',  ( -22.19233475009214374, -280.0848186213743247, -198.8984997803549675 ) ) ;
#30548 = CARTESIAN_POINT ( 'NONE',  ( 12.62934106623620778, -276.7323527833284516, -214.8411876572591268 ) ) ;
#30549 = CARTESIAN_POINT ( 'NONE',  ( -13.96983070625157630, -284.3557710064802677, -199.2167885196802786 ) ) ;
#30550 = CIRCLE ( 'NONE', #42637, 4.999999999999986677 ) ;
#30551 = CARTESIAN_POINT ( 'NONE',  ( -75.24784836585295977, -291.1488134150631595, -336.4637982716405418 ) ) ;
#30552 = CARTESIAN_POINT ( 'NONE',  ( -10.38909202328236958, -293.6122944820573935, -338.5357686248896698 ) ) ;
#30553 = ORIENTED_EDGE ( 'NONE', *, *, #18204, .T. ) ;
#30554 = CARTESIAN_POINT ( 'NONE',  ( 25.80882305186885972, -293.7217050023043612, -307.0230724968720892 ) ) ;
#30555 = CARTESIAN_POINT ( 'NONE',  ( -113.3616278956509547, -291.7638138179833618, -259.8494096928264412 ) ) ;
#30556 = CARTESIAN_POINT ( 'NONE',  ( 17.13324237519024962, -281.5070903846815895, -221.6130584558946168 ) ) ;
#30557 = CARTESIAN_POINT ( 'NONE',  ( 98.51911204938808453, -298.6359351600565333, -193.6943702404669807 ) ) ;
#30558 = CARTESIAN_POINT ( 'NONE',  ( 25.77280380391643888, -288.7858895839764273, -314.3828684735831303 ) ) ;
#30559 = CARTESIAN_POINT ( 'NONE',  ( -34.66330532307965484, -289.3526358162238239, -347.2933641012310773 ) ) ;
#30560 = CARTESIAN_POINT ( 'NONE',  ( -22.45967221883283216, -286.5811219193203669, -198.8206732889066473 ) ) ;
#30561 = CARTESIAN_POINT ( 'NONE',  ( -23.40286736638519471, -134.2391364535880598, 21.50000000000000000 ) ) ;
#30562 = CARTESIAN_POINT ( 'NONE',  ( -96.13039596184697189, -238.4436301958426441, -339.9016185993384056 ) ) ;
#30563 = CARTESIAN_POINT ( 'NONE',  ( -111.1601028361537118, -270.7551610738350973, -283.6484960496011922 ) ) ;
#30564 = CARTESIAN_POINT ( 'NONE',  ( -78.73175922136113059, -276.8225119037208515, -330.7507890222076981 ) ) ;
#30565 = CARTESIAN_POINT ( 'NONE',  ( -102.1365244259444296, -277.0073652384414231, -304.6518866663593599 ) ) ;
#30566 = CARTESIAN_POINT ( 'NONE',  ( -85.79163217217676163, -273.0687217962955629, -210.5418202906136855 ) ) ;
#30567 = CARTESIAN_POINT ( 'NONE',  ( -54.05466194891914000, -170.4008729781827469, -361.7658500053330499 ) ) ;
#30568 = CARTESIAN_POINT ( 'NONE',  ( -51.23957477297972929, -275.9110914645577282, -345.5950687751796409 ) ) ;
#30569 = CARTESIAN_POINT ( 'NONE',  ( 30.01459920551967642, -295.7720977988751656, -305.5335923264745475 ) ) ;
#30570 = ORIENTED_EDGE ( 'NONE', *, *, #17571, .T. ) ;
#30571 = CARTESIAN_POINT ( 'NONE',  ( -30.80770831459367898, -292.6293228255084955, -197.5923376392886155 ) ) ;
#30572 = CARTESIAN_POINT ( 'NONE',  ( -112.1195771238567289, -297.5765158148137743, -252.6854869237473622 ) ) ;
#30573 = CARTESIAN_POINT ( 'NONE',  ( -34.57610967593285523, -287.7016389375725112, -343.8521342775541711 ) ) ;
#30574 = CARTESIAN_POINT ( 'NONE',  ( -29.07414426903120486, -298.6454087753794511, -193.4219860267110391 ) ) ;
#30575 = CARTESIAN_POINT ( 'NONE',  ( -110.3840863323154053, -296.7042681950358087, -271.4652349688109325 ) ) ;
#30576 = ORIENTED_EDGE ( 'NONE', *, *, #79173, .T. ) ;
#30577 = CARTESIAN_POINT ( 'NONE',  ( 197.5379522065467768, 249.5000000000000568, -11.97918851819042807 ) ) ;
#30578 =( BOUNDED_CURVE ( )  B_SPLINE_CURVE ( 3, ( #65014, #36553, #14798, #87198 ),
 .UNSPECIFIED., .F., .F. ) 
 B_SPLINE_CURVE_WITH_KNOTS ( ( 4, 4 ),
 ( 1.570796326794895892, 2.617993877991479312 ),
 .UNSPECIFIED. ) 
 CURVE ( )  GEOMETRIC_REPRESENTATION_ITEM ( )  RATIONAL_B_SPLINE_CURVE ( ( 1.000000000000000000, 0.9106836025229615439, 0.9106836025229615439, 1.000000000000000000 ) ) 
 REPRESENTATION_ITEM ( '' )  );
#30579 = CARTESIAN_POINT ( 'NONE',  ( -39.56976610098377733, -281.9445612293049521, -194.8211647523048384 ) ) ;
#30580 = CARTESIAN_POINT ( 'NONE',  ( -81.48492659777620872, -280.5154970987184129, -211.7687278627689693 ) ) ;
#30581 = CARTESIAN_POINT ( 'NONE',  ( -112.2414876114483349, -280.4745830070029911, -257.5550315501023988 ) ) ;
#30582 = CARTESIAN_POINT ( 'NONE',  ( -76.92044237001688600, -271.9912772614846403, -208.1981795524608003 ) ) ;
#30583 = CARTESIAN_POINT ( 'NONE',  ( 129.9467878515196162, -299.5541904835127980, -200.7046326357662167 ) ) ;
#30584 = CARTESIAN_POINT ( 'NONE',  ( 152.4536156746142410, 275.0000000000000568, -11.50000000000000355 ) ) ;
#30585 = CARTESIAN_POINT ( 'NONE',  ( -3.150971852752717517, -280.6837172330894532, -205.8489241288082212 ) ) ;
#30586 = CARTESIAN_POINT ( 'NONE',  ( 35.91178441532474608, -276.6471478528873718, -293.5577949579000006 ) ) ;
#30587 = CARTESIAN_POINT ( 'NONE',  ( 7.077595747044981955, -278.4478500060455417, -330.8566067148845491 ) ) ;
#30588 = CARTESIAN_POINT ( 'NONE',  ( -35.74218125625489506, -275.6072222886365921, -346.7681714343855219 ) ) ;
#30589 = EDGE_LOOP ( 'NONE', ( #82390, #11465, #45235, #59837 ) ) ;
#30590 = DIRECTION ( 'NONE',  ( -1.000000000000000000, 0.000000000000000000, 0.000000000000000000 ) ) ;
#30591 = CARTESIAN_POINT ( 'NONE',  ( 34.05889703401961555, -283.8439620333300581, -294.6141347269443713 ) ) ;
#30592 = CARTESIAN_POINT ( 'NONE',  ( -93.55736319168633486, -290.4123748477019262, -223.5184825260139689 ) ) ;
#30593 = CARTESIAN_POINT ( 'NONE',  ( 37.27992447637554818, -286.6680819740904553, -251.7889364087348554 ) ) ;
#30594 = EDGE_CURVE ( 'NONE', #24375, #39851, #1533, .T. ) ;
#30595 = CARTESIAN_POINT ( 'NONE',  ( -40.29695153435920929, -281.3296659843946372, -344.3154316117778535 ) ) ;
#30597 = CARTESIAN_POINT ( 'NONE',  ( 31.29889150567325018, -285.2513939124551143, -241.4215632714236790 ) ) ;
#30596 = CARTESIAN_POINT ( 'NONE',  ( -91.18486269218223583, -282.4113280900047016, -320.5237411445754674 ) ) ;
#30598 = CARTESIAN_POINT ( 'NONE',  ( -4.181833166971558491, -281.7044770003787448, -204.8677379663166107 ) ) ;
#30599 = PLANE ( 'NONE',  #41176 ) ;
#30600 = CARTESIAN_POINT ( 'NONE',  ( 0.4536673384999292957, -280.9572038623820163, -336.5422734197180716 ) ) ;
#30601 = CARTESIAN_POINT ( 'NONE',  ( 37.23450167266633315, -295.4439952157991911, -261.9249073331538398 ) ) ;
#30602 = AXIS2_PLACEMENT_3D ( 'NONE', #30637, #59536, #32509 ) ;
#30603 = CARTESIAN_POINT ( 'NONE',  ( -92.79855865534157999, -278.5264022390850300, -317.9891508070831492 ) ) ;
#30604 = CARTESIAN_POINT ( 'NONE',  ( -40.75923848479533262, -288.0095491831267509, -195.2212290370152061 ) ) ;
#30605 = COLOUR_RGB ( '',0.7921568627450980005, 0.8196078431372548767, 0.9333333333333333481 ) ;
#30606 = DIRECTION ( 'NONE',  ( -0.000000000000000000, 1.000000000000000000, -0.000000000000000000 ) ) ;
#30607 = CARTESIAN_POINT ( 'NONE',  ( -3.979611958363965307, -294.4088081039965346, -202.5509459563704695 ) ) ;
#30608 = CIRCLE ( 'NONE', #21561, 2.000000000000000888 ) ;
#30609 = CARTESIAN_POINT ( 'NONE',  ( 37.58648830018066889, -273.4966165233839774, -266.0486861564917263 ) ) ;
#30610 = CARTESIAN_POINT ( 'NONE',  ( -80.45847839062497542, -288.8171745226302392, -334.0265192067412272 ) ) ;
#30611 = CARTESIAN_POINT ( 'NONE',  ( 33.88349486426316304, -292.2050873486961109, -289.7329880104829272 ) ) ;
#30612 = CARTESIAN_POINT ( 'NONE',  ( -43.23650051345222067, -278.5104573893707993, -430.8699914737978816 ) ) ;
#30613 = CARTESIAN_POINT ( 'NONE',  ( -81.12651532718145120, -276.3461517254066280, -329.3876665403880111 ) ) ;
#30614 = CARTESIAN_POINT ( 'NONE',  ( -86.90771506894039078, -295.4931450091982583, -215.0974260968129670 ) ) ;
#30615 = CARTESIAN_POINT ( 'NONE',  ( -72.58070424613561045, -290.8442977220993839, -334.8549631737401455 ) ) ;
#30616 = DIRECTION ( 'NONE',  ( -0.000000000000000000, 1.000000000000000000, -0.000000000000000000 ) ) ;
#30617 = LINE ( 'NONE', #53315, #48856 ) ;
#30618 = CARTESIAN_POINT ( 'NONE',  ( 19.87179139989343568, -291.3419617290406904, -219.8505388229311848 ) ) ;
#30619 = CARTESIAN_POINT ( 'NONE',  ( 36.43062816853321095, -289.1968576723172077, -273.7767548167175278 ) ) ;
#30620 = CARTESIAN_POINT ( 'NONE',  ( -90.06646705202767578, -289.5596800205086083, -215.5699902251751325 ) ) ;
#30621 = EDGE_CURVE ( 'NONE', #33982, #2466, #56225, .T. ) ;
#30622 = CARTESIAN_POINT ( 'NONE',  ( -41.37321168113845715, -287.4257097674345118, -196.8698020162657087 ) ) ;
#30623 = CARTESIAN_POINT ( 'NONE',  ( 123.4306832106270946, -134.2391364535880882, -5.024999999999987921 ) ) ;
#30624 = CARTESIAN_POINT ( 'NONE',  ( 17.00372509066372828, -287.6549784269396355, -221.3610290908781906 ) ) ;
#30625 = CARTESIAN_POINT ( 'NONE',  ( 18.33188221679906249, -296.2381648642396499, -321.2196199662795948 ) ) ;
#30626 = DIRECTION ( 'NONE',  ( -0.9565177946839567014, 2.529868470129570114E-15, 0.2916739763039208899 ) ) ;
#30627 = CARTESIAN_POINT ( 'NONE',  ( 2.984223698884188813, -289.7289947139753394, -335.5526725873778560 ) ) ;
#30628 = CARTESIAN_POINT ( 'NONE',  ( -17.40241850694987846, -278.3283178353904646, -197.6917857409332839 ) ) ;
#30629 = CARTESIAN_POINT ( 'NONE',  ( -100.4457392420967494, -278.3024794396129096, -314.4476753332854173 ) ) ;
#30630 = ADVANCED_FACE ( 'NONE', ( #35839, #36295 ), #86011, .F. ) ;
#30631 = CARTESIAN_POINT ( 'NONE',  ( 3.814254445228949297, -280.2563675923465780, -205.2448528453568599 ) ) ;
#30632 = CARTESIAN_POINT ( 'NONE',  ( -89.28809463189834617, -299.2969937111515719, -216.6846486869660282 ) ) ;
#30633 = CARTESIAN_POINT ( 'NONE',  ( -13.91783132143956081, -284.3557710075663749, -199.0583202572621815 ) ) ;
#30634 = CARTESIAN_POINT ( 'NONE',  ( -110.8437467437025248, -273.8931351520964199, -270.3781919081613978 ) ) ;
#30635 = CARTESIAN_POINT ( 'NONE',  ( 17.99918104428743604, -278.9956669220031813, -220.8813003536822634 ) ) ;
#30636 = CARTESIAN_POINT ( 'NONE',  ( -95.63445920879816242, -281.9020240572296530, -317.5719306624231990 ) ) ;
#30637 = CARTESIAN_POINT ( 'NONE',  ( 129.9467878515196162, -299.5541904835127980, -190.0176033293537898 ) ) ;
#30638 = CARTESIAN_POINT ( 'NONE',  ( -12.11383863348450873, -275.2097445724068052, -342.4322470309236337 ) ) ;
#30639 = CARTESIAN_POINT ( 'NONE',  ( -95.85124850480036685, -298.6968431830242707, -225.5371965432557033 ) ) ;
#30640 = CARTESIAN_POINT ( 'NONE',  ( -114.0315902270491364, -283.4773981730751302, -269.9696266315025923 ) ) ;
#30641 = CARTESIAN_POINT ( 'NONE',  ( -34.48036136891933978, -299.0300895859957109, -197.1253504873549787 ) ) ;
#30642 = CARTESIAN_POINT ( 'NONE',  ( -107.5433937525821193, -274.3662323966685221, -240.0555830563437212 ) ) ;
#30643 = CARTESIAN_POINT ( 'NONE',  ( 18.32177684422274666, -275.8906932691223233, -317.6227812859333426 ) ) ;
#30644 = CARTESIAN_POINT ( 'NONE',  ( -56.28450734845745274, -297.2962361116501597, -342.9833174638788478 ) ) ;
#30645 = CARTESIAN_POINT ( 'NONE',  ( -68.05192736183235525, -289.6110564114273416, -340.9718958268330198 ) ) ;
#30646 = CARTESIAN_POINT ( 'NONE',  ( -8.071796992666712356, -278.5123757827599320, -200.6865678099490253 ) ) ;
#30647 = CARTESIAN_POINT ( 'NONE',  ( -97.46223514609182814, -291.0299029512155471, -222.2516462156972352 ) ) ;
#30648 = CARTESIAN_POINT ( 'NONE',  ( -95.96384920676541697, -288.9964934487360892, -314.2779737561940010 ) ) ;
#30649 = CARTESIAN_POINT ( 'NONE',  ( 9.879838635458678908, -290.7018841847202566, -212.0265643798393853 ) ) ;
#30650 = ORIENTED_EDGE ( 'NONE', *, *, #14576, .T. ) ;
#30651 = LINE ( 'NONE', #72807, #57533 ) ;
#30652 = CARTESIAN_POINT ( 'NONE',  ( -101.7003222097025343, -289.5873346101069501, -305.0509993138333016 ) ) ;
#30653 = CARTESIAN_POINT ( 'NONE',  ( 10.19742947581766401, -229.5268262511776527, 25.50000000000000000 ) ) ;
#30654 = CARTESIAN_POINT ( 'NONE',  ( -67.10891649974158213, -286.6125749206093474, -199.6028460789339078 ) ) ;
#30655 = CARTESIAN_POINT ( 'NONE',  ( -105.5795714935544112, -292.8376638359844719, -285.9686137636504668 ) ) ;
#30656 = CARTESIAN_POINT ( 'NONE',  ( 29.36425339623114183, -293.1069722472940953, -308.4570994373950725 ) ) ;
#30657 = CARTESIAN_POINT ( 'NONE',  ( 31.95288522288795718, -283.2866210507178266, -302.9137357538254491 ) ) ;
#30658 = CARTESIAN_POINT ( 'NONE',  ( -109.1926499096358754, -284.5565872633736717, -257.3896047553525932 ) ) ;
#30659 = CARTESIAN_POINT ( 'NONE',  ( 15.96704342509009145, -277.5916653103729459, -320.9518418246126998 ) ) ;
#30660 = CARTESIAN_POINT ( 'NONE',  ( 27.67942437163184266, -291.0802770493069147, -233.5935451657042279 ) ) ;
#30661 = CARTESIAN_POINT ( 'NONE',  ( -63.43361009054868305, -272.4993633734621312, -201.7447627365557139 ) ) ;
#30662 = ORIENTED_EDGE ( 'NONE', *, *, #48158, .F. ) ;
#30663 = CARTESIAN_POINT ( 'NONE',  ( 84.09003387609358526, 83.72762891241104910, -302.5758382668069544 ) ) ;
#30664 = CARTESIAN_POINT ( 'NONE',  ( 13.37870584045069400, -294.0321486621642748, -328.3384794077394417 ) ) ;
#30665 = CARTESIAN_POINT ( 'NONE',  ( -77.85284232898733592, -287.4239292079402617, -207.8486737744601385 ) ) ;
#30666 = CARTESIAN_POINT ( 'NONE',  ( -113.0864293636219742, -297.7836666561045718, -258.2683156704083558 ) ) ;
#30667 = CARTESIAN_POINT ( 'NONE',  ( -8.221955769621759558, -287.0952873052918903, -203.3093979678432390 ) ) ;
#30668 = CARTESIAN_POINT ( 'NONE',  ( -107.3664055037144180, -277.2065017374494573, -301.9446155322348773 ) ) ;
#30669 = CARTESIAN_POINT ( 'NONE',  ( 37.96039701746756378, -294.0075780040262430, -254.7111408871466267 ) ) ;
#30670 = CARTESIAN_POINT ( 'NONE',  ( 38.12660995884635184, -285.5994405010960691, -263.0995957933824343 ) ) ;
#30671 = CARTESIAN_POINT ( 'NONE',  ( 36.68266203864578046, -293.6200441925374776, -249.1911157424309522 ) ) ;
#30673 = CARTESIAN_POINT ( 'NONE',  ( -89.83446885280095273, -291.6187172169491078, -219.6009296616121276 ) ) ;
#30672 = AXIS2_PLACEMENT_3D ( 'NONE', #83569, #26772, #11619 ) ;
#30674 = DIRECTION ( 'NONE',  ( 0.000000000000000000, 0.000000000000000000, 1.000000000000000000 ) ) ;
#30675 = AXIS2_PLACEMENT_3D ( 'NONE', #59838, #8679, #53650 ) ;
#30676 = DIRECTION ( 'NONE',  ( -1.000000000000000000, 0.000000000000000000, 0.000000000000000000 ) ) ;
#30677 = CARTESIAN_POINT ( 'NONE',  ( 185.2856823004373155, 260.3293175955999459, -151.1391428731211874 ) ) ;
#30678 = CARTESIAN_POINT ( 'NONE',  ( -64.32033406853761903, -287.2265360074954970, -198.9687809053639569 ) ) ;
#30679 = CARTESIAN_POINT ( 'NONE',  ( -20.25526795762938548, -292.3380690714490129, -345.3683826091709648 ) ) ;
#30680 = ORIENTED_EDGE ( 'NONE', *, *, #18534, .F. ) ;
#30681 = CARTESIAN_POINT ( 'NONE',  ( -48.38877429527233431, -282.1163982513141377, -342.8331003294917423 ) ) ;
#30682 = CARTESIAN_POINT ( 'NONE',  ( -108.6384478555322914, -277.8501326739541923, -299.3872795430617657 ) ) ;
#30683 = CARTESIAN_POINT ( 'NONE',  ( 19.00159051718811298, -284.2377290793045859, -319.6100979502661517 ) ) ;
#30684 = CARTESIAN_POINT ( 'NONE',  ( -92.83366527638099797, -240.7103982912584286, -340.5308032049566691 ) ) ;
#30685 = CARTESIAN_POINT ( 'NONE',  ( -68.95934043393330626, -282.0345319544100562, -339.9378496619090697 ) ) ;
#30687 = AXIS2_PLACEMENT_3D ( 'NONE', #8372, #36791, #823 ) ;
#30686 = CARTESIAN_POINT ( 'NONE',  ( -35.87645741426449320, -284.0907313453803908, -195.7306961024721943 ) ) ;
#30688 = CARTESIAN_POINT ( 'NONE',  ( 17.18393258882466412, -276.6797861019121001, -217.6810709008790070 ) ) ;
#30689 = CARTESIAN_POINT ( 'NONE',  ( -86.14604871652491624, -297.8455293533723989, -215.9908687615359497 ) ) ;
#30690 = CARTESIAN_POINT ( 'NONE',  ( -50.57634116159846371, -293.9095417438324489, -342.6528032128883865 ) ) ;
#30691 = CARTESIAN_POINT ( 'NONE',  ( -111.6347024013553408, -279.4529540461732608, -250.4642884469988076 ) ) ;
#30692 = CARTESIAN_POINT ( 'NONE',  ( -16.38086886027196698, -276.7737087032643331, -340.3401131848896171 ) ) ;
#30693 = CARTESIAN_POINT ( 'NONE',  ( -114.0330990441454873, -273.6675114159231157, -267.5188803404774376 ) ) ;
#30694 = CARTESIAN_POINT ( 'NONE',  ( -14.69415164179740252, -275.6858307667873760, -343.6873177583000256 ) ) ;
#30695 = CARTESIAN_POINT ( 'NONE',  ( -104.6885212946842927, -255.7827803519188592, -326.5688778022348515 ) ) ;
#30696 = CARTESIAN_POINT ( 'NONE',  ( -93.00135176084691579, -275.8510104536460403, -320.6493964774192023 ) ) ;
#30697 = AXIS2_PLACEMENT_3D ( 'NONE', #60787, #53678, #50986 ) ;
#30698 = ADVANCED_FACE ( 'NONE', ( #5573 ), #20236, .T. ) ;
#30699 = CARTESIAN_POINT ( 'NONE',  ( -101.0683720381171184, -298.5365188988735099, -228.1766677701635331 ) ) ;
#30700 = FACE_OUTER_BOUND ( 'NONE', #71123, .T. ) ;
#30701 = DIRECTION ( 'NONE',  ( 0.000000000000000000, 0.000000000000000000, -1.000000000000000000 ) ) ;
#30702 = CARTESIAN_POINT ( 'NONE',  ( -48.36163832974614252, -284.2753933237065667, -342.8372315302723905 ) ) ;
#30703 = CARTESIAN_POINT ( 'NONE',  ( -112.1354564836506995, -286.1386677393974765, -284.0610391722537997 ) ) ;
#30704 = CARTESIAN_POINT ( 'NONE',  ( -37.27245837176452881, -285.4015903195714827, -197.2467616316953354 ) ) ;
#30705 = CARTESIAN_POINT ( 'NONE',  ( -110.9551997794928013, -277.0204358685767261, -265.1177333231860302 ) ) ;
#30706 = CARTESIAN_POINT ( 'NONE',  ( -96.07948831425808578, -285.7837963392622100, -315.7772094309784165 ) ) ;
#30707 = CARTESIAN_POINT ( 'NONE',  ( -102.7625571579186214, -277.4903772484469755, -236.3263874081253277 ) ) ;
#30708 = CARTESIAN_POINT ( 'NONE',  ( -51.32644489812637545, -278.3148633365489673, -342.3239763638684963 ) ) ;
#30709 = FACE_OUTER_BOUND ( 'NONE', #71954, .T. ) ;
#30710 = CARTESIAN_POINT ( 'NONE',  ( -16.62921603255674796, -274.8192962103832997, -200.2442429511368687 ) ) ;
#30711 = CARTESIAN_POINT ( 'NONE',  ( 39.11851154794064911, -282.4568750517863123, -278.4912598217030677 ) ) ;
#30712 = VECTOR ( 'NONE', #79226, 1000.000000000000000 ) ;
#30713 = CARTESIAN_POINT ( 'NONE',  ( 21.56694273956899366, -282.7113922162508288, -319.8515079481271073 ) ) ;
#30714 = ORIENTED_EDGE ( 'NONE', *, *, #35942, .F. ) ;
#30715 = VERTEX_POINT ( 'NONE', #34905 ) ;
#30716 = CARTESIAN_POINT ( 'NONE',  ( 198.6639115758706282, 17.12212513345147258, -10.45170682515602323 ) ) ;
#30717 = CARTESIAN_POINT ( 'NONE',  ( 13.40174600858478904, -288.6132600908331369, -214.0287920440416372 ) ) ;
#30718 = CARTESIAN_POINT ( 'NONE',  ( -49.97176851101051653, -297.0840217217794930, -198.2980685109567105 ) ) ;
#30719 = CARTESIAN_POINT ( 'NONE',  ( 20.30777971561858308, -292.2105301521623346, -219.4506501077159442 ) ) ;
#30720 = ADVANCED_FACE ( 'NONE', ( #65212 ), #49113, .F. ) ;
#30721 = CARTESIAN_POINT ( 'NONE',  ( 8.395258187434462727, -286.8926716278811568, -328.1438004621078903 ) ) ;
#30722 = CARTESIAN_POINT ( 'NONE',  ( -66.57970414856659147, -288.0173736524386641, -337.9471555936756886 ) ) ;
#30723 = CARTESIAN_POINT ( 'NONE',  ( 17.17531811845548262, -288.0571566266493733, -221.1994534386860494 ) ) ;
#30724 = CARTESIAN_POINT ( 'NONE',  ( -97.22240257946876341, -275.9343644740023933, -315.5408375941399868 ) ) ;
#30725 = CARTESIAN_POINT ( 'NONE',  ( 5.094724261253341879, -286.8885627266888037, -333.6508509495091630 ) ) ;
#30726 = CARTESIAN_POINT ( 'NONE',  ( -49.05808743230583246, -287.9031698768554293, -196.2295824839782483 ) ) ;
#30727 = CARTESIAN_POINT ( 'NONE',  ( 6.835931173569454344, -286.4529149437168485, -331.2394755736891625 ) ) ;
#30728 = CARTESIAN_POINT ( 'NONE',  ( 33.18927607508316413, -282.7531795207079881, -290.0788725295082600 ) ) ;
#30729 = CARTESIAN_POINT ( 'NONE',  ( -67.61434734465515817, -293.6560919866633412, -201.5459623180830988 ) ) ;
#30730 = CARTESIAN_POINT ( 'NONE',  ( 196.8771864013320680, 214.6606447562234905, -12.54327527393323649 ) ) ;
#30731 = CARTESIAN_POINT ( 'NONE',  ( -47.80257052418233599, -229.5268262511776527, 22.47499999999998721 ) ) ;
#30732 = CARTESIAN_POINT ( 'NONE',  ( -110.1969538447277870, -298.2165402983124523, -290.3967414035506636 ) ) ;
#30733 = CARTESIAN_POINT ( 'NONE',  ( 11.42103552357760066, -279.9463758745067139, -215.8194152378700608 ) ) ;
#30734 = CARTESIAN_POINT ( 'NONE',  ( 30.80017799712559778, -279.1391369788243537, -238.9047102129392499 ) ) ;
#30735 = CARTESIAN_POINT ( 'NONE',  ( 39.28081183249745578, -292.6771637971945097, -264.6035593893051896 ) ) ;
#30736 = CARTESIAN_POINT ( 'NONE',  ( -39.16791977715406858, -296.4287598082912041, -196.5711688138334807 ) ) ;
#30737 = CARTESIAN_POINT ( 'NONE',  ( 36.53205513495402101, -273.7558504733202085, -279.9353271203199256 ) ) ;
#30738 = CARTESIAN_POINT ( 'NONE',  ( -72.34480413197637461, -296.8407151454754285, -334.9976621723017161 ) ) ;
#30739 = CARTESIAN_POINT ( 'NONE',  ( -46.03152702926329454, -296.4237223872028721, -194.5508636611600082 ) ) ;
#30740 = CARTESIAN_POINT ( 'NONE',  ( -107.4489023662299871, -294.4127390446410004, -299.8053167439474578 ) ) ;
#30741 = AXIS2_PLACEMENT_3D ( 'NONE', #48649, #77549, #41540 ) ;
#30742 = EDGE_CURVE ( 'NONE', #63051, #14152, #50968, .T. ) ;
#30743 = CARTESIAN_POINT ( 'NONE',  ( 36.12165325131429938, -294.9106460289418123, -265.2575402751756428 ) ) ;
#30744 = CARTESIAN_POINT ( 'NONE',  ( 183.0442525570908288, 300.2961574867697436, -7.500000000000000000 ) ) ;
#30745 = CARTESIAN_POINT ( 'NONE',  ( -2.371225574760046584, -293.3302217590810415, -206.0844021007544598 ) ) ;
#30746 = CARTESIAN_POINT ( 'NONE',  ( 170.7304434856092143, 276.0000000000000568, -24.91818181818181088 ) ) ;
#30747 = CIRCLE ( 'NONE', #48839, 2.000000000000001776 ) ;
#30749 = CARTESIAN_POINT ( 'NONE',  ( -94.77343848336226984, -295.9167239171960091, -315.4232465329353658 ) ) ;
#30748 = CARTESIAN_POINT ( 'NONE',  ( -84.46430106641275870, -283.4271193461231633, -211.5574847568799441 ) ) ;
#30750 = CIRCLE ( 'NONE', #48842, 2.000000000000000000 ) ;
#30751 = CARTESIAN_POINT ( 'NONE',  ( -114.3548908130070174, -284.5210348520636785, -272.8492333268528682 ) ) ;
#30752 = CARTESIAN_POINT ( 'NONE',  ( -35.39804502326355617, -281.9964866374365897, -194.8132253889213814 ) ) ;
#30753 = CARTESIAN_POINT ( 'NONE',  ( -12.70645810459626368, -286.0305970408420535, -197.4306775484280649 ) ) ;
#30754 = CARTESIAN_POINT ( 'NONE',  ( -110.4975654402052356, -288.7547481693756026, -254.6052365074582440 ) ) ;
#30755 = CARTESIAN_POINT ( 'NONE',  ( -95.95921662488163406, -270.6952119285918457, -223.5744983911110353 ) ) ;
#30756 = CIRCLE ( 'NONE', #70025, 4.999999999999976907 ) ;
#30757 = CARTESIAN_POINT ( 'NONE',  ( -73.78572110730844713, -284.2422806971239879, -206.5258643163653574 ) ) ;
#30758 = CARTESIAN_POINT ( 'NONE',  ( -113.3578563845434246, -289.6048192971995832, -259.8221587332401441 ) ) ;
#30759 = CARTESIAN_POINT ( 'NONE',  ( 201.2104617360081704, 0.000000000000000000, 9.000000000000001776 ) ) ;
#30760 = CARTESIAN_POINT ( 'NONE',  ( 14.89679763691791514, -295.9012026312825014, -322.5634038923562343 ) ) ;
#30761 = CARTESIAN_POINT ( 'NONE',  ( -98.96352418531954243, -280.5823069761846682, -225.1576488086723202 ) ) ;
#30763 = CARTESIAN_POINT ( 'NONE',  ( 9.293302485419381753, -280.3800044079196709, -214.1056646280910343 ) ) ;
#30762 = CARTESIAN_POINT ( 'NONE',  ( -50.21194661902687528, -293.2356056660836430, -344.6618997651258383 ) ) ;
#30764 = CARTESIAN_POINT ( 'NONE',  ( -70.80595324782682098, -295.6480367922205801, -339.7236182855646689 ) ) ;
#30765 = AXIS2_PLACEMENT_3D ( 'NONE', #22805, #51672, #28994 ) ;
#30766 = CARTESIAN_POINT ( 'NONE',  ( -112.1767626617573939, -282.4942027894425109, -281.1731583314693808 ) ) ;
#30767 = EDGE_CURVE ( 'NONE', #22436, #14651, #13150, .T. ) ;
#30768 = CARTESIAN_POINT ( 'NONE',  ( -50.61145333056632012, -281.8828257199812697, -196.5443563635312785 ) ) ;
#30769 = CARTESIAN_POINT ( 'NONE',  ( -39.70861269458068676, -294.1413156074694371, -343.5706249872390003 ) ) ;
#30770 = CARTESIAN_POINT ( 'NONE',  ( 17.58432135626699022, -296.7395371843010707, -195.3798368471506706 ) ) ;
#30771 = ORIENTED_EDGE ( 'NONE', *, *, #68018, .T. ) ;
#30772 = CARTESIAN_POINT ( 'NONE',  ( 202.6531192844442728, 63.25403289341416269, -9.673168394505404777 ) ) ;
#30773 = VECTOR ( 'NONE', #68109, 1000.000000000000000 ) ;
#30774 = CARTESIAN_POINT ( 'NONE',  ( -6.103590747113877057, -282.4445556861036266, -202.5531599629256050 ) ) ;
#30775 = CARTESIAN_POINT ( 'NONE',  ( -80.19593387614979463, -295.1579863652195854, -329.5346178904471799 ) ) ;
#30776 = DIRECTION ( 'NONE',  ( 1.000000000000000000, -0.000000000000000000, 5.880589007913310608E-16 ) ) ;
#30777 = CARTESIAN_POINT ( 'NONE',  ( 10.64812456238590777, -278.1952119285918457, -210.2361428286349110 ) ) ;
#30778 = CARTESIAN_POINT ( 'NONE',  ( -85.69866662021578918, -272.5992459651270678, -210.6471111527235678 ) ) ;
#30779 = CARTESIAN_POINT ( 'NONE',  ( -34.66718048847827305, -290.3343699242483353, -346.8212070397212869 ) ) ;
#30780 = CARTESIAN_POINT ( 'NONE',  ( -102.4086035363959724, -290.8362989218113626, -237.1539389000297149 ) ) ;
#30781 = CARTESIAN_POINT ( 'NONE',  ( -14.10847418865916936, -281.8790414658838586, -200.3720279850016368 ) ) ;
#30782 = CARTESIAN_POINT ( 'NONE',  ( 16.01120344943208451, -276.4240061499760372, -219.2978712780624733 ) ) ;
#30783 = AXIS2_PLACEMENT_3D ( 'NONE', #32164, #40168, #62940 ) ;
#30784 = CARTESIAN_POINT ( 'NONE',  ( -81.51468190424904492, -278.2311176008949474, -211.6809444703450822 ) ) ;
#30785 = CARTESIAN_POINT ( 'NONE',  ( 27.10686732003000898, -278.0655883576399106, -308.7197258924548464 ) ) ;
#30786 = ORIENTED_EDGE ( 'NONE', *, *, #59917, .F. ) ;
#30787 = CARTESIAN_POINT ( 'NONE',  ( 13.96605773749421431, -274.5817538268141789, -212.8745875764777793 ) ) ;
#30788 = CARTESIAN_POINT ( 'NONE',  ( -93.66169169272090755, -293.1524323693145107, -221.6849148624908707 ) ) ;
#30789 = DIRECTION ( 'NONE',  ( -0.000000000000000000, -0.000000000000000000, 1.000000000000000000 ) ) ;
#30790 = CARTESIAN_POINT ( 'NONE',  ( 198.3013281324776926, 65.29263651785086608, 9.735123833055002507 ) ) ;
#30791 = CARTESIAN_POINT ( 'NONE',  ( -19.65180315312841586, -290.4167113165010505, -196.6364640528616121 ) ) ;
#30792 = CARTESIAN_POINT ( 'NONE',  ( -75.21798337578533733, -297.1992919624360070, -207.8727383157991824 ) ) ;
#30793 = DIRECTION ( 'NONE',  ( 0.000000000000000000, 0.000000000000000000, 1.000000000000000000 ) ) ;
#30794 = CARTESIAN_POINT ( 'NONE',  ( -2.390813492799769957, -294.0261305994960139, -202.5147473267676901 ) ) ;
#30795 = CARTESIAN_POINT ( 'NONE',  ( -85.28047601435908120, -286.1948066931273615, -330.5268031993605859 ) ) ;
#30796 = CARTESIAN_POINT ( 'NONE',  ( 37.46379743484509106, -289.5968253763476810, -273.8197834064524159 ) ) ;
#30797 = CARTESIAN_POINT ( 'NONE',  ( -6.781697966510144227, -274.6499094321674193, -338.6700829691203580 ) ) ;
#30798 = CARTESIAN_POINT ( 'NONE',  ( 24.22992037913066099, -276.9014550049094510, -228.5022783285045307 ) ) ;
#30799 = CARTESIAN_POINT ( 'NONE',  ( -58.03218868781078754, -289.8627521962294509, -198.8004353172029539 ) ) ;
#30800 = CARTESIAN_POINT ( 'NONE',  ( -40.97327799142219362, -281.8673538163822059, -194.6704154582403987 ) ) ;
#30801 = ORIENTED_EDGE ( 'NONE', *, *, #57401, .F. ) ;
#30802 = CARTESIAN_POINT ( 'NONE',  ( -42.94900150372097869, -282.4732346736718114, -343.2978358253071178 ) ) ;
#30803 = CARTESIAN_POINT ( 'NONE',  ( -110.3680817387783009, -279.3341855749993670, -293.9550698515365070 ) ) ;
#30804 = AXIS2_PLACEMENT_3D ( 'NONE', #13060, #92088, #49021 ) ;
#30805 = CARTESIAN_POINT ( 'NONE',  ( -52.85229397362792270, -282.0414629774623450, -345.4315308849867279 ) ) ;
#30806 = CARTESIAN_POINT ( 'NONE',  ( -1.566724959004111906, -277.5308946173458935, -338.2799766684636324 ) ) ;
#30807 = DIRECTION ( 'NONE',  ( 1.000000000000000000, 0.000000000000000000, 0.000000000000000000 ) ) ;
#30808 = CARTESIAN_POINT ( 'NONE',  ( 7.846202039818450658, -277.9678887343407041, -331.9144443956383839 ) ) ;
#30809 = CARTESIAN_POINT ( 'NONE',  ( 27.33386217378599881, -283.6233781216987495, -239.1787733560258573 ) ) ;
#30810 = EDGE_LOOP ( 'NONE', ( #87571, #9856, #38318, #70436 ) ) ;
#30811 = ORIENTED_EDGE ( 'NONE', *, *, #35747, .T. ) ;
#30812 = CARTESIAN_POINT ( 'NONE',  ( -101.8747147855665105, -298.0399770324070232, -308.6796865119803783 ) ) ;
#30813 = AXIS2_PLACEMENT_3D ( 'NONE', #49578, #85091, #42463 ) ;
#30814 = CARTESIAN_POINT ( 'NONE',  ( -21.04731783917208787, -289.9177925857937339, -341.8364226580233094 ) ) ;
#30815 = CARTESIAN_POINT ( 'NONE',  ( -64.96475342421375387, -275.4347424554158579, -339.7616297575960402 ) ) ;
#30816 = CARTESIAN_POINT ( 'NONE',  ( -95.59952814923676101, -291.6467394332894401, -319.1665308045383540 ) ) ;
#30817 = CARTESIAN_POINT ( 'NONE',  ( -95.18997482794893017, -290.5291158257365964, -225.6680560737433723 ) ) ;
#30818 = CARTESIAN_POINT ( 'NONE',  ( 12.37128700372701573, -287.8887207784222824, -329.0820325998622593 ) ) ;
#30819 = CARTESIAN_POINT ( 'NONE',  ( 209.1374487190023501, 30.94653725228601715, 12.09245862095555601 ) ) ;
#30820 = CARTESIAN_POINT ( 'NONE',  ( -109.7094852617887994, -283.1408187200852353, -255.8923899166755120 ) ) ;
#30821 = CARTESIAN_POINT ( 'NONE',  ( -66.79771287259356427, -291.3025309230109201, -338.5571333640543799 ) ) ;
#30822 = CARTESIAN_POINT ( 'NONE',  ( -95.49234025866557829, -283.6641016190898767, -225.0724244462670924 ) ) ;
#30823 = CARTESIAN_POINT ( 'NONE',  ( 35.63151381142870378, -282.9871202483654429, -279.5030732748415403 ) ) ;
#30824 = CARTESIAN_POINT ( 'NONE',  ( 25.66546950460050880, -289.0756815752255307, -314.3034804150059927 ) ) ;
#30825 = AXIS2_PLACEMENT_3D ( 'NONE', #37594, #8717, #59878 ) ;
#30826 = CARTESIAN_POINT ( 'NONE',  ( -108.0337153144891005, -279.2885519241328893, -251.8558646779087553 ) ) ;
#30827 = CARTESIAN_POINT ( 'NONE',  ( 1.512008411810999542, -291.3538862561458700, -204.2823279412429827 ) ) ;
#30828 = CARTESIAN_POINT ( 'NONE',  ( 11.96611122471376731, -287.5199487840773713, -211.3603920930030995 ) ) ;
#30829 = CARTESIAN_POINT ( 'NONE',  ( 22.36136238827849354, -288.6962779021726533, -318.9109306136004989 ) ) ;
#30830 = CARTESIAN_POINT ( 'NONE',  ( -108.4248121873693691, -284.4989454371670377, -287.0347275724043925 ) ) ;
#30831 = VERTEX_POINT ( 'NONE', #57623 ) ;
#30832 = CARTESIAN_POINT ( 'NONE',  ( 194.2870706607532441, 27.06158795357650604, 14.58823529798582896 ) ) ;
#30833 = CARTESIAN_POINT ( 'NONE',  ( 22.12362110497789658, -294.7741227646307607, -223.3916887767994979 ) ) ;
#30834 = AXIS2_PLACEMENT_3D ( 'NONE', #75687, #10812, #92218 ) ;
#30835 = CARTESIAN_POINT ( 'NONE',  ( 37.86934828177489720, -292.4143589055810253, -284.4531096408489361 ) ) ;
#30836 = CIRCLE ( 'NONE', #88261, 7.500000000000007105 ) ;
#30837 = CARTESIAN_POINT ( 'NONE',  ( -51.33755177823420013, -276.2942651994949301, -342.2466143222532651 ) ) ;
#30838 = CARTESIAN_POINT ( 'NONE',  ( -110.7133623401958999, -296.1923658369367445, -247.1648483659918440 ) ) ;
#30839 = EDGE_CURVE ( 'NONE', #93354, #8225, #9364, .T. ) ;
#30840 = CARTESIAN_POINT ( 'NONE',  ( 30.50154763801040758, -291.6477892382942514, -241.4554683993791286 ) ) ;
#30841 = CARTESIAN_POINT ( 'NONE',  ( -73.32013459407018274, -295.8078636147137104, -205.6809334755501197 ) ) ;
#30842 = CARTESIAN_POINT ( 'NONE',  ( -77.48509179236710054, -292.7052443709765157, -208.9148926311063690 ) ) ;
#30843 = CARTESIAN_POINT ( 'NONE',  ( 36.01738309023951246, -294.6369107577861541, -270.7478900384898566 ) ) ;
#30844 = DIRECTION ( 'NONE',  ( 0.000000000000000000, 1.000000000000000000, 0.000000000000000000 ) ) ;
#30845 = CIRCLE ( 'NONE', #80705, 1.000000000000003331 ) ;
#30846 = CARTESIAN_POINT ( 'NONE',  ( 18.15839412620846716, -292.2587546078964920, -321.1297799080661548 ) ) ;
#30847 = CARTESIAN_POINT ( 'NONE',  ( -99.40254063079866853, -299.1233527197991293, -228.1588794409857428 ) ) ;
#30848 = CARTESIAN_POINT ( 'NONE',  ( 35.50722417909328499, -288.3946207428232356, -262.8482839552062273 ) ) ;
#30849 = CARTESIAN_POINT ( 'NONE',  ( -4.684356370965116589, -278.6040342858181589, -338.2863156209719477 ) ) ;
#30850 = CARTESIAN_POINT ( 'NONE',  ( -113.2257384258998201, -277.3646709480278787, -260.2165416380571514 ) ) ;
#30851 = AXIS2_PLACEMENT_3D ( 'NONE', #29737, #81298, #65747 ) ;
#30852 = CARTESIAN_POINT ( 'NONE',  ( -112.3420280466402517, -272.1133616190666089, -253.3827906410119226 ) ) ;
#30853 = CARTESIAN_POINT ( 'NONE',  ( 10.82214414349227560, -280.4603475647468258, -327.1876582976967143 ) ) ;
#30854 = CARTESIAN_POINT ( 'NONE',  ( -74.59880919751368822, -277.9648036321973450, -203.8904609995308874 ) ) ;
#30855 = CARTESIAN_POINT ( 'NONE',  ( -109.8521900102618218, -295.0800244483023675, -282.3391117895540106 ) ) ;
#30856 = DIRECTION ( 'NONE',  ( 0.000000000000000000, 0.000000000000000000, 1.000000000000000000 ) ) ;
#30857 = CARTESIAN_POINT ( 'NONE',  ( 34.72474627639046219, -276.0410783374624657, -258.0263121627884857 ) ) ;
#30858 = CARTESIAN_POINT ( 'NONE',  ( 194.5400481336216387, 25.95059276991969099, 14.25215709970754041 ) ) ;
#30859 = CARTESIAN_POINT ( 'NONE',  ( -105.7563170623370326, -288.9866227387603885, -238.6481710770466123 ) ) ;
#30860 = CARTESIAN_POINT ( 'NONE',  ( -97.29007649960774984, -289.9041391513514441, -318.7057374775315566 ) ) ;
#30861 = CARTESIAN_POINT ( 'NONE',  ( -19.02205139238770215, -276.2874411217178476, -197.4073416543744486 ) ) ;
#30862 = CARTESIAN_POINT ( 'NONE',  ( -112.0408566726942183, -294.6096294032310539, -265.8817837155626194 ) ) ;
#30863 = CARTESIAN_POINT ( 'NONE',  ( 0.7793460100420999126, -281.7543709765553785, -337.0917176694905493 ) ) ;
#30864 = DIRECTION ( 'NONE',  ( 1.000000000000000000, 0.000000000000000000, 0.000000000000000000 ) ) ;
#30865 = CARTESIAN_POINT ( 'NONE',  ( 15.69617743849259917, -280.3017984011779618, -323.4610907491652370 ) ) ;
#30866 = FACE_OUTER_BOUND ( 'NONE', #29022, .T. ) ;
#30867 = CARTESIAN_POINT ( 'NONE',  ( -109.6653655975623565, -289.5149669882046624, -257.5645647395224955 ) ) ;
#30868 = CARTESIAN_POINT ( 'NONE',  ( -107.3463383787781993, -282.3666718629504544, -295.2168867701692534 ) ) ;
#30869 = CARTESIAN_POINT ( 'NONE',  ( 198.5293976728803784, 41.98013133710430367, 10.72178272438543445 ) ) ;
#30870 = DIRECTION ( 'NONE',  ( -1.000000000000000000, -0.000000000000000000, -0.000000000000000000 ) ) ;
#30871 = CARTESIAN_POINT ( 'NONE',  ( 21.77464982989269160, -290.9185876728425342, -224.1856021271876216 ) ) ;
#30872 = CARTESIAN_POINT ( 'NONE',  ( -89.63850011275077634, -279.4044360939305989, -322.5055873775744999 ) ) ;
#30873 = CARTESIAN_POINT ( 'NONE',  ( 19.49924152228387442, -283.4588150744407358, -321.7916005121845728 ) ) ;
#30875 = CARTESIAN_POINT ( 'NONE',  ( -37.28087273214584485, -286.0528980263154040, -197.3487048133511053 ) ) ;
#30874 = CARTESIAN_POINT ( 'NONE',  ( 15.04657443394469851, -272.8641938875279607, -215.9112981046183108 ) ) ;
#30876 = CARTESIAN_POINT ( 'NONE',  ( 25.89107511748261814, -277.4907927886520724, -308.0040595643965844 ) ) ;
#30877 = CARTESIAN_POINT ( 'NONE',  ( 9.775828408964978067, -277.1865735196354876, -326.3302186632087114 ) ) ;
#30878 = EDGE_CURVE ( 'NONE', #46575, #25984, #92508, .T. ) ;
#30879 = CARTESIAN_POINT ( 'NONE',  ( -90.50377291779354039, -287.2993055973473702, -217.4574823376597124 ) ) ;
#30880 = EDGE_LOOP ( 'NONE', ( #4119, #57344, #86774 ) ) ;
#30881 = FACE_OUTER_BOUND ( 'NONE', #87287, .T. ) ;
#30882 = CARTESIAN_POINT ( 'NONE',  ( -113.1387418114993437, -296.5550293662739136, -256.8035195019820662 ) ) ;
#30883 = CARTESIAN_POINT ( 'NONE',  ( 10.05590126678781893, -288.6891379060571126, -212.6955807735517681 ) ) ;
#30884 = CARTESIAN_POINT ( 'NONE',  ( 195.4781563537916043, 27.48493576247232895, 15.00000000000000000 ) ) ;
#30885 = CARTESIAN_POINT ( 'NONE',  ( 13.79469577742117181, -285.9094976428776249, -334.5364918783848793 ) ) ;
#30886 = CARTESIAN_POINT ( 'NONE',  ( -112.9294888653194704, -277.6352290505569158, -257.4004581242679137 ) ) ;
#30887 = CARTESIAN_POINT ( 'NONE',  ( -34.96473907088594757, -290.4813829905241960, -194.1851841416402351 ) ) ;
#30888 = AXIS2_PLACEMENT_3D ( 'NONE', #46326, #67665, #82325 ) ;
#30889 = CARTESIAN_POINT ( 'NONE',  ( -109.0445793503759262, -286.2952361977594364, -253.2948059606713969 ) ) ;
#30890 = CARTESIAN_POINT ( 'NONE',  ( -111.3653967849307236, -280.3443673796571716, -267.8965756014687827 ) ) ;
#30891 = CARTESIAN_POINT ( 'NONE',  ( 31.16723846048784807, -289.4169750666260938, -304.3202993333458153 ) ) ;
#30892 = CARTESIAN_POINT ( 'NONE',  ( 36.68151218948661096, -283.7072261756798639, -282.4261371738191997 ) ) ;
#30893 = CARTESIAN_POINT ( 'NONE',  ( 26.06808917318163310, -276.2965745335932297, -314.1363398641886420 ) ) ;
#30894 = CARTESIAN_POINT ( 'NONE',  ( -40.56430231468502257, -296.0315640567754372, -195.7730783687483722 ) ) ;
#30895 = CARTESIAN_POINT ( 'NONE',  ( -72.50491866364795612, -279.4330608981057367, -201.8442911778038820 ) ) ;
#30896 = AXIS2_PLACEMENT_3D ( 'NONE', #43436, #56263, #13186 ) ;
#30897 = CARTESIAN_POINT ( 'NONE',  ( -110.6990019307856983, -298.6359535463627140, -257.7111981572658692 ) ) ;
#30898 = CIRCLE ( 'NONE', #83803, 0.5000000000000004441 ) ;
#30899 = CARTESIAN_POINT ( 'NONE',  ( 156.4697130957886202, 16.02030068022430598, 10.01540472299883788 ) ) ;
#30900 = CARTESIAN_POINT ( 'NONE',  ( 10.59707575819634329, -283.1948066931273047, -210.1954327657594490 ) ) ;
#30901 = CARTESIAN_POINT ( 'NONE',  ( -75.89895036840451326, -271.7849774771071907, -204.8227570746032882 ) ) ;
#30902 = CARTESIAN_POINT ( 'NONE',  ( 219.8344101925596021, 35.72494958537217968, 7.000000000000000000 ) ) ;
#30903 = CARTESIAN_POINT ( 'NONE',  ( -56.62244419163911147, -276.8150031597948555, -340.8852257245467285 ) ) ;
#30904 = CIRCLE ( 'NONE', #83810, 0.5000000000000004441 ) ;
#30905 = CARTESIAN_POINT ( 'NONE',  ( -71.24096313766156641, -274.8196076151936040, -201.6672413429360518 ) ) ;
#30906 = CARTESIAN_POINT ( 'NONE',  ( 24.40962406065657575, -280.0030237770741337, -224.7585503524113619 ) ) ;
#30907 = CARTESIAN_POINT ( 'NONE',  ( -50.91561475274457393, -290.9879667829274581, -343.1714857444937934 ) ) ;
#30908 = CARTESIAN_POINT ( 'NONE',  ( -65.30611237074187159, -299.2134579309066567, -199.3067523476892404 ) ) ;
#30909 = CARTESIAN_POINT ( 'NONE',  ( -46.09978616359826020, -299.1484808340330801, -194.2604961254596105 ) ) ;
#30910 = CARTESIAN_POINT ( 'NONE',  ( -52.77206598574392871, -293.8542785152798160, -197.0826938709160743 ) ) ;
#30911 = CARTESIAN_POINT ( 'NONE',  ( 2.045116585425529099, -280.5238692333006725, -334.0510667200915691 ) ) ;
#30912 = CARTESIAN_POINT ( 'NONE',  ( 19.03950347069537585, -282.7932157371956805, -221.7362703742093402 ) ) ;
#30913 = CARTESIAN_POINT ( 'NONE',  ( 0.3045703254873016741, -272.5762476158075742, -205.8899693141657963 ) ) ;
#30914 = CARTESIAN_POINT ( 'NONE',  ( -113.4083212519305448, -286.0850304614825745, -275.6824285141259452 ) ) ;
#30915 = AXIS2_PLACEMENT_3D ( 'NONE', #13794, #42646, #6218 ) ;
#30916 = CARTESIAN_POINT ( 'NONE',  ( -82.74845060867620816, -288.6102892066414256, -327.9150325620414037 ) ) ;
#30917 = CARTESIAN_POINT ( 'NONE',  ( 198.8200449370011995, 284.3224334190195464, -111.7342436523391029 ) ) ;
#30918 = ORIENTED_EDGE ( 'NONE', *, *, #86831, .T. ) ;
#30919 = CARTESIAN_POINT ( 'NONE',  ( 17.83872032041365685, -287.9009263383961184, -318.2615888902410575 ) ) ;
#30920 = ORIENTED_EDGE ( 'NONE', *, *, #30385, .T. ) ;
#30921 = CARTESIAN_POINT ( 'NONE',  ( -67.74610994585918888, -284.5215885327106662, -340.7675408007664828 ) ) ;
#30922 = CARTESIAN_POINT ( 'NONE',  ( 34.14117166887788812, -275.6880084067138910, -255.3908159382060603 ) ) ;
#30923 = CARTESIAN_POINT ( 'NONE',  ( -104.3332548732852700, -289.9584105575837043, -233.0298428661952244 ) ) ;
#30924 = CARTESIAN_POINT ( 'NONE',  ( 22.44925252602147481, -282.8530277955014185, -318.7384346170857157 ) ) ;
#30925 = CARTESIAN_POINT ( 'NONE',  ( 16.71812759666127590, -282.3241927860921692, -216.4331443942766953 ) ) ;
#30926 = CARTESIAN_POINT ( 'NONE',  ( -79.14468289328844719, -283.9329756154883171, -335.0005403454044313 ) ) ;
#30927 = CARTESIAN_POINT ( 'NONE',  ( -83.43773839673744419, -279.3999851422124721, -213.6904333508806531 ) ) ;
#30928 = CARTESIAN_POINT ( 'NONE',  ( -4.771743288812454686, -271.9809262143061233, -202.8022627189028810 ) ) ;
#30929 = CARTESIAN_POINT ( 'NONE',  ( 174.5893627881048928, 243.1951182970949503, -179.8094511266240829 ) ) ;
#30930 = VERTEX_POINT ( 'NONE', #36758 ) ;
#30931 = CARTESIAN_POINT ( 'NONE',  ( -10.57508152806877355, -278.7023282806881639, -340.2437092007280626 ) ) ;
#30932 = CARTESIAN_POINT ( 'NONE',  ( 64.01848135404819118, 48.19560674472151618, -318.4631135849222119 ) ) ;
#30933 = CARTESIAN_POINT ( 'NONE',  ( -96.17743270066428352, -296.5081959115459540, -226.9550913852802125 ) ) ;
#30934 = CARTESIAN_POINT ( 'NONE',  ( 20.33671706934794798, -292.3695704743377064, -219.4223832503387825 ) ) ;
#30935 = CARTESIAN_POINT ( 'NONE',  ( 168.2916594723880905, 229.6308326061414391, -190.1149449454625824 ) ) ;
#30936 = EDGE_CURVE ( 'NONE', #69284, #47807, #1813, .T. ) ;
#30938 = CARTESIAN_POINT ( 'NONE',  ( -61.53631049351803028, -287.7716523653417653, -340.0824292416541539 ) ) ;
#30937 = CARTESIAN_POINT ( 'NONE',  ( -112.5801950777285185, -271.4151616006713539, -256.2053483126125570 ) ) ;
#30939 = CARTESIAN_POINT ( 'NONE',  ( -89.35060544490218604, -297.6538926294820726, -323.4044528949978030 ) ) ;
#30940 = ADVANCED_FACE ( 'NONE', ( #81233, #23007 ), #51420, .T. ) ;
#30941 = CARTESIAN_POINT ( 'NONE',  ( -17.05169117012472668, -287.6347035934186920, -199.6711062099155356 ) ) ;
#30942 = VERTEX_POINT ( 'NONE', #16380 ) ;
#30943 = CARTESIAN_POINT ( 'NONE',  ( 23.84869874287717195, -295.1128094497666439, -316.7136292387993421 ) ) ;
#30944 = CARTESIAN_POINT ( 'NONE',  ( -76.15450780505386774, -284.0781456425465876, -332.3204980065190171 ) ) ;
#30945 = CARTESIAN_POINT ( 'NONE',  ( -113.5539487023561094, -271.5799049758838919, -261.8062552366379805 ) ) ;
#30946 = CARTESIAN_POINT ( 'NONE',  ( 26.35330516716049942, -293.7864222017060456, -227.2895773231536225 ) ) ;
#30947 = CARTESIAN_POINT ( 'NONE',  ( 22.24296058536637943, -294.6985700973331745, -319.0561808675521434 ) ) ;
#30948 = CARTESIAN_POINT ( 'NONE',  ( -85.93061022477877486, -291.5235007570179278, -215.8126428492608966 ) ) ;
#30949 = ORIENTED_EDGE ( 'NONE', *, *, #58839, .T. ) ;
#30950 = CARTESIAN_POINT ( 'NONE',  ( 159.4851178187817879, 15.28877977928774357, 9.000000000000001776 ) ) ;
#30951 = CARTESIAN_POINT ( 'NONE',  ( -34.83466128549527241, -299.9436287636900147, -194.5955260062804939 ) ) ;
#30952 = CARTESIAN_POINT ( 'NONE',  ( 15.76287283857926269, -273.5791570138986231, -215.1532105064771656 ) ) ;
#30953 = ORIENTED_EDGE ( 'NONE', *, *, #16095, .T. ) ;
#30954 = VERTEX_POINT ( 'NONE', #44318 ) ;
#30955 = CARTESIAN_POINT ( 'NONE',  ( -35.71909818086986377, -276.5399964837521338, -347.2955810091828539 ) ) ;
#30956 = CARTESIAN_POINT ( 'NONE',  ( -67.36449829597728467, -272.0515927815287114, -202.9301278194689075 ) ) ;
#30957 = CARTESIAN_POINT ( 'NONE',  ( -105.5867528592758191, -280.7984783900357115, -241.1467678195408553 ) ) ;
#30958 = CARTESIAN_POINT ( 'NONE',  ( -26.87030663151578480, -275.0571566278396745, -343.8540795280833322 ) ) ;
#30959 = CARTESIAN_POINT ( 'NONE',  ( -104.0860325928904189, -298.1682404018121133, -239.7047398712782922 ) ) ;
#30960 = CARTESIAN_POINT ( 'NONE',  ( -67.16426205753275269, -274.5925621974017190, -203.4592398691484618 ) ) ;
#30961 = CARTESIAN_POINT ( 'NONE',  ( -80.69093503821387969, -275.2335496103571018, -207.8888690576729914 ) ) ;
#30962 = CARTESIAN_POINT ( 'NONE',  ( -16.21382576296086242, -272.3439297494500124, -197.9742533303364951 ) ) ;
#30963 = CARTESIAN_POINT ( 'NONE',  ( 33.54693810343505334, -294.4388429849327622, -288.2131105377094968 ) ) ;
#30964 = CARTESIAN_POINT ( 'NONE',  ( -33.45934403757850362, -290.6766683638933841, -196.8617764458852832 ) ) ;
#30965 = DIRECTION ( 'NONE',  ( 0.000000000000000000, 0.000000000000000000, -1.000000000000000000 ) ) ;
#30966 = CARTESIAN_POINT ( 'NONE',  ( -28.60179523275668600, -277.4366107036450444, -346.8550915018040541 ) ) ;
#30967 = CARTESIAN_POINT ( 'NONE',  ( -32.69315238843643101, -274.2790156907939831, -197.4967488178583892 ) ) ;
#30968 = CARTESIAN_POINT ( 'NONE',  ( -101.0180605870684900, -282.6741351852214734, -312.8663388961496139 ) ) ;
#30969 = CARTESIAN_POINT ( 'NONE',  ( -36.27430838535670432, -297.0389920590856718, -345.5330013424953108 ) ) ;
#30970 = CARTESIAN_POINT ( 'NONE',  ( 139.6925840978351516, 15.36528803885690664, -21.50000000000000000 ) ) ;
#30971 = CARTESIAN_POINT ( 'NONE',  ( -11.95638942263939875, -285.5883862540134146, -201.7448828240623016 ) ) ;
#30972 = CONICAL_SURFACE ( 'NONE', #65807, 8.500000000000007105, 0.7853981633974591592 ) ;
#30973 = CARTESIAN_POINT ( 'NONE',  ( -31.79754602902082183, -280.9821973046804828, -345.3359988806927845 ) ) ;
#30974 = CARTESIAN_POINT ( 'NONE',  ( -0.9918388780831031148, -274.8028678399028877, -334.8912821822397632 ) ) ;
#30975 = CARTESIAN_POINT ( 'NONE',  ( 7.928702925703531967, -274.9947406118189974, -328.4429786278427628 ) ) ;
#30976 = CARTESIAN_POINT ( 'NONE',  ( 37.62044297025344974, -283.5992433719841301, -274.0158655108357948 ) ) ;
#30977 = CARTESIAN_POINT ( 'NONE',  ( 34.76071216147933995, -276.5771566678704403, -256.6362264438267289 ) ) ;
#30978 = DIRECTION ( 'NONE',  ( -1.124465274301078034E-16, -1.000000000000000000, -0.000000000000000000 ) ) ;
#30979 = CARTESIAN_POINT ( 'NONE',  ( -29.89656310287272234, -272.5447819910657472, -194.5257017870235927 ) ) ;
#30980 = CIRCLE ( 'NONE', #19087, 25.00000000000000355 ) ;
#30981 = CARTESIAN_POINT ( 'NONE',  ( -22.94293154858993589, -282.2359772141625740, -196.5334739464187237 ) ) ;
#30982 = DIRECTION ( 'NONE',  ( 1.000000000000000000, 0.000000000000000000, 0.000000000000000000 ) ) ;
#30983 = CARTESIAN_POINT ( 'NONE',  ( 15.27851364362460274, -288.7085948671503957, -216.1354109878155327 ) ) ;
#30984 = DIRECTION ( 'NONE',  ( -1.000000000000000000, 0.000000000000000000, 0.000000000000000000 ) ) ;
#30985 = CARTESIAN_POINT ( 'NONE',  ( -65.11036602495053671, -287.4146716371830053, -340.0853651668093676 ) ) ;
#30986 = CIRCLE ( 'NONE', #83880, 2.000000000000001776 ) ;
#30987 = CYLINDRICAL_SURFACE ( 'NONE', #89045, 1.000000000000000888 ) ;
#30988 = CARTESIAN_POINT ( 'NONE',  ( -68.20055119649290987, -296.4325544396785403, -203.7526220073208663 ) ) ;
#30989 = CARTESIAN_POINT ( 'NONE',  ( -92.57663154455117649, -289.3899842749509617, -220.7440493597310933 ) ) ;
#30990 = CARTESIAN_POINT ( 'NONE',  ( -75.88346903603265048, -208.4961600436150491, -353.2410745688453062 ) ) ;
#30991 = CARTESIAN_POINT ( 'NONE',  ( -47.51962034187837247, -295.9227495767913751, -196.0023115497991739 ) ) ;
#30992 = CARTESIAN_POINT ( 'NONE',  ( 35.19605352522275155, -285.7294230312164700, -246.5069419418688028 ) ) ;
#30993 = CARTESIAN_POINT ( 'NONE',  ( -6.905125520319645105, -284.2460515452305003, -337.6063407802757297 ) ) ;
#30994 = CARTESIAN_POINT ( 'NONE',  ( 0.3460335736755167368, -280.7972168517744080, -336.3580293811020283 ) ) ;
#30995 = CARTESIAN_POINT ( 'NONE',  ( -109.9728876694250630, -290.6488305719263394, -263.0323666336493034 ) ) ;
#30996 = CARTESIAN_POINT ( 'NONE',  ( 7.487014525540851118, -282.1022584347446127, -211.9377555673985967 ) ) ;
#30997 = CARTESIAN_POINT ( 'NONE',  ( -29.41702354663625485, -283.7521827771386143, -343.1427532545968120 ) ) ;
#30998 = CARTESIAN_POINT ( 'NONE',  ( -56.84045206463820676, -291.2821259691905880, -343.2038134865892403 ) ) ;
#30999 = CARTESIAN_POINT ( 'NONE',  ( -112.4236025583908827, -273.0978965691595022, -253.3772368265154284 ) ) ;
#31000 = VERTEX_POINT ( 'NONE', #30584 ) ;
#31001 = CARTESIAN_POINT ( 'NONE',  ( -73.75522819553066256, -287.6114785624052388, -336.5829098105638195 ) ) ;
#31002 = CARTESIAN_POINT ( 'NONE',  ( 35.72995802030734325, -275.2446097838474088, -245.9127482146673742 ) ) ;
#31003 = CARTESIAN_POINT ( 'NONE',  ( -89.08860771884337737, -293.3005492446556559, -216.4927803500606274 ) ) ;
#31004 = DIRECTION ( 'NONE',  ( 0.000000000000000000, 0.000000000000000000, 1.000000000000000000 ) ) ;
#31005 = CARTESIAN_POINT ( 'NONE',  ( 39.58706461736021254, -278.0519495502701943, -270.3284710469133074 ) ) ;
#31006 = CARTESIAN_POINT ( 'NONE',  ( -112.5430771785299982, -276.5726598176918287, -268.7475629791378537 ) ) ;
#31007 = DIRECTION ( 'NONE',  ( 0.000000000000000000, 0.000000000000000000, 1.000000000000000000 ) ) ;
#31008 = CARTESIAN_POINT ( 'NONE',  ( -80.15848654505538207, -295.8832813941472182, -207.2646544771614003 ) ) ;
#31009 = CARTESIAN_POINT ( 'NONE',  ( -93.85189590183601638, -272.5569400192231342, -223.9681668027124601 ) ) ;
#31010 = CARTESIAN_POINT ( 'NONE',  ( -108.0661060631505421, -292.3441740029152811, -249.6096001975662659 ) ) ;
#31011 = CARTESIAN_POINT ( 'NONE',  ( -107.2297361661133692, -291.7830566190655190, -248.4311625303689652 ) ) ;
#31012 = CARTESIAN_POINT ( 'NONE',  ( -87.60073110271942198, -285.5250884443810833, -324.7635604935977653 ) ) ;
#31013 = CARTESIAN_POINT ( 'NONE',  ( 30.36831092891625516, -294.5157216689004827, -234.8359552624269497 ) ) ;
#31014 = CARTESIAN_POINT ( 'NONE',  ( 8.541702243843536380, -293.9807435108533582, -209.0740018201842076 ) ) ;
#31015 = CARTESIAN_POINT ( 'NONE',  ( -35.65274239336272899, -294.8637293497181986, -343.3540733213288831 ) ) ;
#31016 = CARTESIAN_POINT ( 'NONE',  ( 34.22966173808458734, -289.8434941295461158, -292.9515798301669065 ) ) ;
#31017 = CARTESIAN_POINT ( 'NONE',  ( 37.67701682203558278, -281.5011298769188670, -252.9483071895343755 ) ) ;
#31018 = CARTESIAN_POINT ( 'NONE',  ( -110.6174491953025552, -270.9391015437068972, -250.8999779970192492 ) ) ;
#31019 = CARTESIAN_POINT ( 'NONE',  ( -63.19943619837910376, -285.5577499735842935, -197.8326581214946316 ) ) ;
#31020 = CARTESIAN_POINT ( 'NONE',  ( 23.82788639542939535, -278.1164994543727289, -313.2298977835650362 ) ) ;
#31021 = CARTESIAN_POINT ( 'NONE',  ( -89.93673888223572987, -284.0840889647931817, -219.0935482792116318 ) ) ;
#31022 = CARTESIAN_POINT ( 'NONE',  ( 36.81209533043386983, -285.4066402843414494, -259.0408637420689502 ) ) ;
#31023 = CARTESIAN_POINT ( 'NONE',  ( -25.56386379960523669, -278.3402871659473590, -195.5173603953421662 ) ) ;
#31024 = CARTESIAN_POINT ( 'NONE',  ( 161.2244399300530233, 8.542400036368780647, 10.00000000000000000 ) ) ;
#31025 = CARTESIAN_POINT ( 'NONE',  ( -95.81142413951739911, -284.6742469950197005, -226.5515320925865694 ) ) ;
#31026 = CARTESIAN_POINT ( 'NONE',  ( -17.11169846175850751, -281.5127730607071044, -196.4777250574909999 ) ) ;
#31027 = CARTESIAN_POINT ( 'NONE',  ( 39.12144958106048875, -286.5184563743397916, -262.9918087221679457 ) ) ;
#31028 = CARTESIAN_POINT ( 'NONE',  ( 21.34015577906363603, -295.9385735188422473, -315.4863527194883659 ) ) ;
#31029 = CARTESIAN_POINT ( 'NONE',  ( -12.11164019505260114, -278.3294920447376057, -342.3183787250977730 ) ) ;
#31030 = CARTESIAN_POINT ( 'NONE',  ( -90.97132770574519611, -279.1091573190154804, -324.9986601091004559 ) ) ;
#31031 = CARTESIAN_POINT ( 'NONE',  ( -110.3919405749448828, -278.3818457035766301, -270.6359353346821877 ) ) ;
#31032 = CARTESIAN_POINT ( 'NONE',  ( -37.17036250404844822, -300.0544674658183908, -195.5247971959151698 ) ) ;
#31033 = CARTESIAN_POINT ( 'NONE',  ( 35.79301563801396924, -285.3479802380443857, -254.5073556351011348 ) ) ;
#31034 = CARTESIAN_POINT ( 'NONE',  ( -113.3131159164553310, -292.0695748469799469, -276.9053817887482296 ) ) ;
#31035 = CARTESIAN_POINT ( 'NONE',  ( -9.124555206144174591, -293.5946391394468833, -338.0358384481833696 ) ) ;
#31036 = VERTEX_POINT ( 'NONE', #80778 ) ;
#31037 = CARTESIAN_POINT ( 'NONE',  ( -35.65437969978824384, -294.6971551619258776, -343.3752645657835387 ) ) ;
#31038 = ORIENTED_EDGE ( 'NONE', *, *, #89992, .F. ) ;
#31039 = CARTESIAN_POINT ( 'NONE',  ( -105.7346971997313432, -292.0816390355956855, -235.5468607831030567 ) ) ;
#31040 = CARTESIAN_POINT ( 'NONE',  ( -46.47740995313754553, -280.5847093735756630, -197.7811118939073367 ) ) ;
#31041 = CARTESIAN_POINT ( 'NONE',  ( -94.90208187056848033, -272.3007570314575219, -219.5711320898629424 ) ) ;
#31042 = CARTESIAN_POINT ( 'NONE',  ( 39.25233834771363917, -288.1108650007719234, -262.9588120497893442 ) ) ;
#31043 = CARTESIAN_POINT ( 'NONE',  ( -17.72561874659924186, -289.1391174892108893, -344.7987001751171761 ) ) ;
#31044 = CARTESIAN_POINT ( 'NONE',  ( 18.67525144526882741, -287.2205446943539755, -223.4994722412025681 ) ) ;
#31045 = CARTESIAN_POINT ( 'NONE',  ( 207.7761861081325776, 35.69891260691534285, 14.41714557868295010 ) ) ;
#31046 = CARTESIAN_POINT ( 'NONE',  ( 201.3567329005774127, 295.1815717130147050, -68.48326189999360736 ) ) ;
#31047 = CARTESIAN_POINT ( 'NONE',  ( -89.29193934165813573, -229.1055583197461942, -344.3944809956333302 ) ) ;
#31048 = CARTESIAN_POINT ( 'NONE',  ( -9.937345416836114609, -275.8820881573837482, -338.2098295645109260 ) ) ;
#31049 = CARTESIAN_POINT ( 'NONE',  ( -66.94001918243773730, -276.3697760837334840, -337.4294829807162159 ) ) ;
#31050 = CARTESIAN_POINT ( 'NONE',  ( -71.38962926465048042, -273.2814996947798818, -201.3213988842951494 ) ) ;
#31051 = CARTESIAN_POINT ( 'NONE',  ( -54.13981448090132176, -170.3343158955618435, -361.5216119282826526 ) ) ;
#31052 = EDGE_CURVE ( 'NONE', #36421, #48026, #57731, .T. ) ;
#31053 = CARTESIAN_POINT ( 'NONE',  ( -71.36667737921057153, -276.1769077074770280, -338.8855603213022505 ) ) ;
#31054 = CIRCLE ( 'NONE', #40070, 0.4999999999999983347 ) ;
#31055 = CARTESIAN_POINT ( 'NONE',  ( -78.20364462691486551, -290.1102090505617639, -330.9884301060386633 ) ) ;
#31056 = CARTESIAN_POINT ( 'NONE',  ( -70.66827288754706160, -298.4265770473597286, -201.1260230554900943 ) ) ;
#31057 = CARTESIAN_POINT ( 'NONE',  ( -78.79359665440387062, -274.1605715028558734, -205.5918887082693232 ) ) ;
#31058 = CARTESIAN_POINT ( 'NONE',  ( -75.21245992568800887, -297.6991725676423357, -207.8941330934979703 ) ) ;
#31059 = VERTEX_POINT ( 'NONE', #8793 ) ;
#31060 = CARTESIAN_POINT ( 'NONE',  ( 156.5440870305766055, 249.5000000000000568, 17.21343741151179429 ) ) ;
#31061 = CARTESIAN_POINT ( 'NONE',  ( -95.03358613203458560, -279.8021199260835488, -319.1761667144942294 ) ) ;
#31062 = CARTESIAN_POINT ( 'NONE',  ( -50.08949138887742691, -282.7181737146946148, -346.2899841551241025 ) ) ;
#31063 = CARTESIAN_POINT ( 'NONE',  ( -94.68626719785807211, -278.9893310696669460, -316.0520169221155129 ) ) ;
#31064 = CARTESIAN_POINT ( 'NONE',  ( -112.0649975234610451, -280.1365116622330333, -284.2311474986369717 ) ) ;
#31065 = CARTESIAN_POINT ( 'NONE',  ( -111.0350334602965745, -271.0322748266905251, -270.3418080582339371 ) ) ;
#31066 = CARTESIAN_POINT ( 'NONE',  ( 197.4232166643840856, 67.42327970493053613, -10.33362320210538421 ) ) ;
#31067 = DIRECTION ( 'NONE',  ( -1.000000000000000000, 0.000000000000000000, 0.000000000000000000 ) ) ;
#31068 = CARTESIAN_POINT ( 'NONE',  ( -5.560412548954341005, -280.6489433850561568, -204.6424009808283984 ) ) ;
#31069 = CARTESIAN_POINT ( 'NONE',  ( 38.02598496985002186, -276.5424985299037530, -285.3234327765041485 ) ) ;
#31070 = CARTESIAN_POINT ( 'NONE',  ( 22.78008526482760487, -278.1646343248336279, -315.1982852973474678 ) ) ;
#31071 = CARTESIAN_POINT ( 'NONE',  ( 38.79186051735894836, -274.2088363098354762, -276.8639815984653865 ) ) ;
#31072 = ORIENTED_EDGE ( 'NONE', *, *, #42128, .T. ) ;
#31073 = CARTESIAN_POINT ( 'NONE',  ( 196.7383257810085979, 24.47698789593438917, 11.00000000000000000 ) ) ;
#31074 = CARTESIAN_POINT ( 'NONE',  ( -30.78233733491283530, -291.3343519672021671, -197.4942771925220484 ) ) ;
#31075 = CARTESIAN_POINT ( 'NONE',  ( 22.91719306640145604, -286.2604194844438439, -222.5679743845104497 ) ) ;
#31076 = CARTESIAN_POINT ( 'NONE',  ( -68.22738407053934395, -281.7033387046247412, -337.6221657255593414 ) ) ;
#31078 = CARTESIAN_POINT ( 'NONE',  ( 37.12148549603017500, -285.6052818854415136, -268.2964456424501805 ) ) ;
#31077 = CARTESIAN_POINT ( 'NONE',  ( -65.55827921416104687, -282.0031993396327721, -338.3395216137096213 ) ) ;
#31079 = CARTESIAN_POINT ( 'NONE',  ( 6.088408726772941648, -290.4634891809606643, -331.5697826998103892 ) ) ;
#31080 = CARTESIAN_POINT ( 'NONE',  ( 33.11145527166746660, -282.4864676467091726, -249.7824056915294477 ) ) ;
#31081 = CARTESIAN_POINT ( 'NONE',  ( -95.37195680833850986, -271.2071589840551269, -222.8280344407132532 ) ) ;
#31082 = CARTESIAN_POINT ( 'NONE',  ( -37.33499450532752206, -281.4519118874254673, -346.5740495856546204 ) ) ;
#31083 = CARTESIAN_POINT ( 'NONE',  ( 14.12523251046627593, -296.3295367555321036, -324.9152699007491378 ) ) ;
#31084 = CARTESIAN_POINT ( 'NONE',  ( -64.36077052982544444, -277.9443337727344101, -199.2849078251018966 ) ) ;
#31085 = CARTESIAN_POINT ( 'NONE',  ( -78.68282330291975768, -278.2765235587290249, -330.7120894137035521 ) ) ;
#31086 = CARTESIAN_POINT ( 'NONE',  ( -111.2017541711363577, -286.7345149946154947, -256.1355601458240585 ) ) ;
#31087 = DIRECTION ( 'NONE',  ( -0.000000000000000000, -0.000000000000000000, -1.000000000000000000 ) ) ;
#31088 = CARTESIAN_POINT ( 'NONE',  ( -36.42094875976950163, -293.9837602904037794, -194.7939360289124124 ) ) ;
#31089 = CARTESIAN_POINT ( 'NONE',  ( -4.204748410161117000, -274.6152354737340033, -337.6579485607016409 ) ) ;
#31090 = CARTESIAN_POINT ( 'NONE',  ( 19.49789741447913727, -287.4537028498629070, -322.0858286992382205 ) ) ;
#31091 = CARTESIAN_POINT ( 'NONE',  ( 9.370793387368959060, -291.1060558259313780, -213.1600367166799685 ) ) ;
#31092 = DIRECTION ( 'NONE',  ( 0.000000000000000000, 0.000000000000000000, 1.000000000000000000 ) ) ;
#31093 = CARTESIAN_POINT ( 'NONE',  ( -59.35858162277882144, -276.0280705720673495, -340.4788789733017893 ) ) ;
#31094 = CARTESIAN_POINT ( 'NONE',  ( -97.42180567627605114, -294.0914502449464294, -313.9861081809409598 ) ) ;
#31095 = CARTESIAN_POINT ( 'NONE',  ( -109.9033482112654241, -291.7134588841587401, -282.1042400704192232 ) ) ;
#31096 = CARTESIAN_POINT ( 'NONE',  ( 221.8344101925596306, -44.55766379199612004, -22.50000000000000000 ) ) ;
#31097 = DIRECTION ( 'NONE',  ( 0.000000000000000000, 0.8660254037842823882, 0.5000000000002706724 ) ) ;
#31098 = CARTESIAN_POINT ( 'NONE',  ( 37.38689756574318324, -291.8363941073275214, -254.8585912475083717 ) ) ;
#31099 = CARTESIAN_POINT ( 'NONE',  ( 36.48003702114210967, -289.1249978696617973, -268.2696779565584961 ) ) ;
#31100 = CARTESIAN_POINT ( 'NONE',  ( -108.9186928366016360, -288.4639722891505471, -296.0262226212167320 ) ) ;
#31101 = CARTESIAN_POINT ( 'NONE',  ( -10.55224504863196877, -287.8338716735656817, -201.8077148912684606 ) ) ;
#31102 = CARTESIAN_POINT ( 'NONE',  ( 189.9243309297870610, 275.5000000000000568, 20.22542485937349355 ) ) ;
#31103 = CARTESIAN_POINT ( 'NONE',  ( 5.948384017670295343, -289.2511842730640410, -329.4036667606699211 ) ) ;
#31104 = CARTESIAN_POINT ( 'NONE',  ( -47.38681910095937155, -297.1591099574680470, -345.0437959326230271 ) ) ;
#31105 = PLANE ( 'NONE',  #42859 ) ;
#31106 = CARTESIAN_POINT ( 'NONE',  ( -30.93244985530418489, -287.3364908038143426, -194.0135598770844467 ) ) ;
#31107 = CARTESIAN_POINT ( 'NONE',  ( -71.73315828344635747, -277.6201419977205660, -203.2972893066325923 ) ) ;
#31108 = CARTESIAN_POINT ( 'NONE',  ( -39.95798192828497974, -277.4174277667568731, -347.3085641051430343 ) ) ;
#31109 = CARTESIAN_POINT ( 'NONE',  ( -4.949022481863993406, -280.1338350311138470, -200.5294723872359270 ) ) ;
#31110 = CARTESIAN_POINT ( 'NONE',  ( -109.9446830035449096, -274.6849205963936242, -253.9257573333467803 ) ) ;
#31111 = CARTESIAN_POINT ( 'NONE',  ( -7.434644306230026700, -284.4441421982089651, -201.5819884206332517 ) ) ;
#31112 = CARTESIAN_POINT ( 'NONE',  ( -48.18343439339133027, -276.2959221541210582, -501.8817130775132682 ) ) ;
#31113 = CARTESIAN_POINT ( 'NONE',  ( 3.401376990437325887, -278.7454020324543649, -208.2440689300214558 ) ) ;
#31114 = CARTESIAN_POINT ( 'NONE',  ( -41.48480965851955915, -281.1040366499012180, -345.2975657566988161 ) ) ;
#31115 = CARTESIAN_POINT ( 'NONE',  ( 60.29495240252359878, -249.1689065933675238, 22.50000000000000000 ) ) ;
#31116 = CARTESIAN_POINT ( 'NONE',  ( -67.45299189145065100, -275.9199020261984856, -340.4754379337923069 ) ) ;
#31117=STYLED_ITEM('',(#93752),#90135);
#31118 = CARTESIAN_POINT ( 'NONE',  ( -92.69882106824934453, -297.3843667337218335, -319.0057159843598242 ) ) ;
#31119 = CARTESIAN_POINT ( 'NONE',  ( -3.043468525732636820, -281.5300511094091007, -338.9696164472081250 ) ) ;
#31120 = CARTESIAN_POINT ( 'NONE',  ( -98.92468540723368164, -296.9455227787425997, -310.0891370555709727 ) ) ;
#31121 = CARTESIAN_POINT ( 'NONE',  ( -113.2791241367444428, -274.0844449043332247, -261.8691260446893239 ) ) ;
#31122 = CARTESIAN_POINT ( 'NONE',  ( -92.03118050562272856, -272.9099756358900208, -221.9757046552343525 ) ) ;
#31123 = CARTESIAN_POINT ( 'NONE',  ( -6.469640349231226217, -294.4577616547124990, -202.0096982667619159 ) ) ;
#31124 = CARTESIAN_POINT ( 'NONE',  ( 39.35446176752952852, -287.6262099187212584, -262.9551506621767203 ) ) ;
#31125 = EDGE_CURVE ( 'NONE', #11101, #83213, #32020, .T. ) ;
#31126 = CARTESIAN_POINT ( 'NONE',  ( -69.33007469440485693, -277.7144762720596987, -201.8922107046597603 ) ) ;
#31127 = CARTESIAN_POINT ( 'NONE',  ( -94.70988830552268212, -291.0821642469255721, -219.0007150465193320 ) ) ;
#31128 = CARTESIAN_POINT ( 'NONE',  ( -78.31595514275134917, -288.6768407134449035, -331.1224128368806419 ) ) ;
#31129 = CARTESIAN_POINT ( 'NONE',  ( 36.87663642770926486, -291.4088359904366712, -259.2118925189142828 ) ) ;
#31130 = VERTEX_POINT ( 'NONE', #45230 ) ;
#31131 = LINE ( 'NONE', #377, #15201 ) ;
#31132 = CARTESIAN_POINT ( 'NONE',  ( -96.61220654691716447, -289.4628784095506830, -313.0810841650403518 ) ) ;
#31133 = CARTESIAN_POINT ( 'NONE',  ( 113.5000000000000568, -296.0521521680024080, -400.5374811273811702 ) ) ;
#31134 = CARTESIAN_POINT ( 'NONE',  ( -29.49893008541301853, -287.0904414250848617, -193.9980957088475293 ) ) ;
#31135 = CARTESIAN_POINT ( 'NONE',  ( -21.33282851196159058, -285.3376638359844719, -340.3538533559490702 ) ) ;
#31136 = CARTESIAN_POINT ( 'NONE',  ( -53.25221955996107681, -294.3099916530228484, -345.5132698308053136 ) ) ;
#31137 = CARTESIAN_POINT ( 'NONE',  ( 8.923979335357861586, -283.7473621979519294, -331.2937461487116479 ) ) ;
#31138 = CARTESIAN_POINT ( 'NONE',  ( -82.79638025751717123, -283.5267814159249156, -327.5475390881124440 ) ) ;
#31139 = CARTESIAN_POINT ( 'NONE',  ( -92.17055285695741418, -273.4614253745668293, -216.2982202343365827 ) ) ;
#31140 = CARTESIAN_POINT ( 'NONE',  ( 23.45090834968755900, -276.2965725833308852, -229.0408253517988726 ) ) ;
#31141 = CARTESIAN_POINT ( 'NONE',  ( -11.67140004799853514, -290.4080372402483476, -200.2140613158329643 ) ) ;
#31142 = CARTESIAN_POINT ( 'NONE',  ( 3.161782837225202147, -273.4041933492162570, -209.0909061564801448 ) ) ;
#31143 = ORIENTED_EDGE ( 'NONE', *, *, #13746, .T. ) ;
#31144 = DIRECTION ( 'NONE',  ( 0.7071067811864494290, 0.000000000000000000, 0.7071067811866457165 ) ) ;
#31145 = CARTESIAN_POINT ( 'NONE',  ( -68.16586294432359239, -287.5643137180773010, -202.6028329715966549 ) ) ;
#31146 = CARTESIAN_POINT ( 'NONE',  ( -104.3261903770420815, -297.1444842018564145, -307.8135951936343986 ) ) ;
#31147 = CARTESIAN_POINT ( 'NONE',  ( -108.4666152091295714, -285.4266680623216530, -253.4211180973144337 ) ) ;
#31148 = EDGE_CURVE ( 'NONE', #26188, #50286, #72748, .T. ) ;
#31149 = CARTESIAN_POINT ( 'NONE',  ( -99.46642073409125828, -277.0105674942417409, -315.4760379398939563 ) ) ;
#31150 = CARTESIAN_POINT ( 'NONE',  ( 36.18708073237117162, -293.9205021860741454, -247.8482067582093293 ) ) ;
#31151 = CARTESIAN_POINT ( 'NONE',  ( 11.30295960121781640, -284.8571288396806267, -212.2064757025541439 ) ) ;
#31152 = CARTESIAN_POINT ( 'NONE',  ( -4.507698627687532600, -294.9645524544523028, -340.0008142084745373 ) ) ;
#31153 = CARTESIAN_POINT ( 'NONE',  ( -52.37826750909458440, -292.1876674294911709, -198.8529971689560512 ) ) ;
#31154 = LINE ( 'NONE', #1326, #59420 ) ;
#31155 = LINE ( 'NONE', #88878, #83872 ) ;
#31156 = CARTESIAN_POINT ( 'NONE',  ( -11.83151317026870863, -92.77902702734904494, -356.4673753602164084 ) ) ;
#31157 = CARTESIAN_POINT ( 'NONE',  ( -113.1332553958814060, -286.1839767811628121, -261.5096829539981513 ) ) ;
#31158 = CARTESIAN_POINT ( 'NONE',  ( -85.33152481854864391, -293.1952119285920162, -330.4860931364850671 ) ) ;
#31159 = VERTEX_POINT ( 'NONE', #25238 ) ;
#31160 = CARTESIAN_POINT ( 'NONE',  ( -67.92580901613808919, -282.3836984344101211, -336.9857257343207948 ) ) ;
#31161 = CARTESIAN_POINT ( 'NONE',  ( -111.8080682624107709, -277.9740491756704728, -289.9194430079709832 ) ) ;
#31162 = CARTESIAN_POINT ( 'NONE',  ( 33.70943723173035522, -283.2462194378555864, -246.7083055832999605 ) ) ;
#31163 = CARTESIAN_POINT ( 'NONE',  ( 203.5065358818463039, 290.8197351118913616, -82.79791085622774460 ) ) ;
#31164 = CARTESIAN_POINT ( 'NONE',  ( -10.92292360015097863, -281.2892216431121142, -342.1156832415301778 ) ) ;
#31165 = CARTESIAN_POINT ( 'NONE',  ( 35.60872053726603070, -285.3682452542266788, -254.5471073751929225 ) ) ;
#31166 = CARTESIAN_POINT ( 'NONE',  ( -32.78101520179771455, -275.9694312606602011, -194.7207649540964951 ) ) ;
#31167 = CARTESIAN_POINT ( 'NONE',  ( -110.4359676837275117, -297.0658990923544138, -268.7377798556076414 ) ) ;
#31168 = CARTESIAN_POINT ( 'NONE',  ( 34.97139959636359663, -292.0641807090532325, -257.1739236609606678 ) ) ;
#31169 = CARTESIAN_POINT ( 'NONE',  ( -77.75426505457394910, -278.2307938404647984, -335.8457519960007858 ) ) ;
#31170 = CARTESIAN_POINT ( 'NONE',  ( -59.19499859944602349, -277.3430327698906126, -340.0133494322519141 ) ) ;
#31171 = CARTESIAN_POINT ( 'NONE',  ( -89.96081201947748696, -274.4097504971363151, -214.4968149782511375 ) ) ;
#31172 = CARTESIAN_POINT ( 'NONE',  ( -89.01402651425053136, -276.6789528308228796, -327.0308911854293115 ) ) ;
#31173 = CARTESIAN_POINT ( 'NONE',  ( 138.5464852710080379, 180.7133914993734436, -241.3450704664923023 ) ) ;
#31174 = CARTESIAN_POINT ( 'NONE',  ( 25.34202474789456616, -274.1087936162026040, -311.6327664301645655 ) ) ;
#31175 = ADVANCED_FACE ( 'NONE', ( #74135 ), #6362, .T. ) ;
#31176 = CARTESIAN_POINT ( 'NONE',  ( -30.62453176540203614, -296.3940587629892889, -346.4760701393184377 ) ) ;
#31177 = CARTESIAN_POINT ( 'NONE',  ( 152.6524812969444724, 129.6175404775655409, 12.50000000000000000 ) ) ;
#31178 = DIRECTION ( 'NONE',  ( 0.9531768234071974488, -0.3024135303179478762, 6.994718006607575617E-16 ) ) ;
#31179 = CARTESIAN_POINT ( 'NONE',  ( -93.65071082920812273, -284.9685253581998836, -317.3027986978677291 ) ) ;
#31180 = CARTESIAN_POINT ( 'NONE',  ( -109.2583027693600428, -285.9990202902943111, -294.8963228410667625 ) ) ;
#31181 = CARTESIAN_POINT ( 'NONE',  ( -60.00236293355126804, -285.0991491072461486, -200.8601321678202112 ) ) ;
#31182 = CARTESIAN_POINT ( 'NONE',  ( -109.5517186309650697, -276.7532046744018999, -285.5977070091549308 ) ) ;
#31183 = CARTESIAN_POINT ( 'NONE',  ( -111.0971906121151136, -286.2975372072384062, -279.2290373385666271 ) ) ;
#31184 = CARTESIAN_POINT ( 'NONE',  ( -85.92690563530614156, -277.8442349794473785, -214.9518628300086220 ) ) ;
#31185 = CARTESIAN_POINT ( 'NONE',  ( -18.92607358121420091, -277.8891153793734361, -341.3194914952528052 ) ) ;
#31186 = DIRECTION ( 'NONE',  ( 1.000000000000000000, -0.000000000000000000, -0.000000000000000000 ) ) ;
#31187 = CARTESIAN_POINT ( 'NONE',  ( -35.39496626076196151, -274.5695560508064546, -197.3130034089043363 ) ) ;
#31188 = AXIS2_PLACEMENT_3D ( 'NONE', #53852, #60966, #4131 ) ;
#31189 = CARTESIAN_POINT ( 'NONE',  ( 8.442107870269278891, -281.4637397830929331, -208.5859754575935199 ) ) ;
#31190 = CARTESIAN_POINT ( 'NONE',  ( -28.23851193312138363, -280.6569362847545790, -193.9095071544167865 ) ) ;
#31191 = ORIENTED_EDGE ( 'NONE', *, *, #18859, .T. ) ;
#31192 = ORIENTED_EDGE ( 'NONE', *, *, #60666, .T. ) ;
#31193 = CARTESIAN_POINT ( 'NONE',  ( 197.3663942936547073, 19.61288093082362138, -11.77299963048799825 ) ) ;
#31194 = CARTESIAN_POINT ( 'NONE',  ( 35.20954916508422627, -289.6915559102340580, -292.2378930924705287 ) ) ;
#31195 = CARTESIAN_POINT ( 'NONE',  ( -98.57713424454352946, -296.3040376577786219, -230.2341828547328646 ) ) ;
#31196 = CARTESIAN_POINT ( 'NONE',  ( -88.57538942831727979, -290.7040064570267646, -213.0163547779379769 ) ) ;
#31197 = CARTESIAN_POINT ( 'NONE',  ( 35.96606130279737812, -285.9336434222134358, -262.8325148160609501 ) ) ;
#31198 = CARTESIAN_POINT ( 'NONE',  ( -3.108310395638296697, -287.1656985107426863, -335.5593133010006568 ) ) ;
#31199 = CARTESIAN_POINT ( 'NONE',  ( -49.50234660859983649, -287.0988731822736213, -197.9266796547319132 ) ) ;
#31200 = CARTESIAN_POINT ( 'NONE',  ( -69.46805234446085819, -275.4747023220432993, -338.1461062446286974 ) ) ;
#31201 = CARTESIAN_POINT ( 'NONE',  ( 29.64955561954562313, -286.4279818388127410, -306.7841156911260896 ) ) ;
#31202 = CARTESIAN_POINT ( 'NONE',  ( 8.565927474749594595, -288.6812277543717187, -211.0526837296688996 ) ) ;
#31203 = CARTESIAN_POINT ( 'NONE',  ( -77.18670593061705176, -287.5843468117639645, -334.1588359666959605 ) ) ;
#31204 = CARTESIAN_POINT ( 'NONE',  ( -45.65430985022116062, -284.1012085413401564, -343.1742780628101741 ) ) ;
#31205 = CARTESIAN_POINT ( 'NONE',  ( -112.2824234709824083, -292.4695425225361305, -276.8219813907830940 ) ) ;
#31206 = DIRECTION ( 'NONE',  ( 0.000000000000000000, 0.000000000000000000, 1.000000000000000000 ) ) ;
#31207 = CARTESIAN_POINT ( 'NONE',  ( -74.94434090351494149, -280.8906705383787994, 22.50000000000000000 ) ) ;
#31208 = CARTESIAN_POINT ( 'NONE',  ( -37.27978344253750009, -299.9730717146126153, -194.8003405251599816 ) ) ;
#31209 = CARTESIAN_POINT ( 'NONE',  ( 33.27211649700328167, -280.4964862288603058, -251.1744415036023952 ) ) ;
#31210 = CARTESIAN_POINT ( 'NONE',  ( 35.71418299237766547, -279.3341532064007993, -253.3953113404013777 ) ) ;
#31211 = CARTESIAN_POINT ( 'NONE',  ( 23.03842418190843588, -293.3864071452224493, -317.9048447339581003 ) ) ;
#31212 = CARTESIAN_POINT ( 'NONE',  ( -85.95915093221232439, -271.6078548603810532, -214.4867573899274760 ) ) ;
#31213 = CARTESIAN_POINT ( 'NONE',  ( 37.13922741289556484, -273.6484516620014915, -271.6335103043355161 ) ) ;
#31214 = CARTESIAN_POINT ( 'NONE',  ( -105.4124117120327071, -297.4986762830105818, -298.0671047246954686 ) ) ;
#31215 = CARTESIAN_POINT ( 'NONE',  ( -113.5000000000000568, -298.0521521680024080, -397.9547385950631337 ) ) ;
#31216 = CARTESIAN_POINT ( 'NONE',  ( -85.42327959076786215, -271.9769064233275344, -210.9745201034476736 ) ) ;
#31217 = CARTESIAN_POINT ( 'NONE',  ( -104.3493041490805808, -295.2625406826643939, -234.4172416969004189 ) ) ;
#31218 = CARTESIAN_POINT ( 'NONE',  ( 23.82096670782933856, -294.4136692671864921, -229.4404251394196592 ) ) ;
#31219 = CARTESIAN_POINT ( 'NONE',  ( 104.2209783822911646, -299.5541904835127980, -193.4627128438320938 ) ) ;
#31220 = CARTESIAN_POINT ( 'NONE',  ( 27.30553509052749916, -294.8218637758599243, -304.7234052940085007 ) ) ;
#31221 = PLANE ( 'NONE',  #71676 ) ;
#31223 = CARTESIAN_POINT ( 'NONE',  ( 28.39455219974218636, -293.9831561068069163, -302.2226944999908937 ) ) ;
#31222 = CARTESIAN_POINT ( 'NONE',  ( -49.06345900759774281, -283.9237579926843296, -195.8705901125350124 ) ) ;
#31224 = CARTESIAN_POINT ( 'NONE',  ( -24.53358155959462295, -282.8931503969599817, -346.3425155850067654 ) ) ;
#31225 = CARTESIAN_POINT ( 'NONE',  ( 20.84585023827576578, -282.8119220947845065, -222.1581804790805279 ) ) ;
#31226 = CARTESIAN_POINT ( 'NONE',  ( -99.32468945516025371, -284.8265113520943714, -224.6241757582789376 ) ) ;
#31227 = CARTESIAN_POINT ( 'NONE',  ( -89.18272769446753045, -289.3211376649276190, -216.3216111355461635 ) ) ;
#31228 = CARTESIAN_POINT ( 'NONE',  ( 36.51581113150614044, -280.2742441802406006, -289.5385991784507382 ) ) ;
#31229 = CARTESIAN_POINT ( 'NONE',  ( -8.043061220241614961, -285.1290179622242817, -202.9605746822465449 ) ) ;
#31230 = CARTESIAN_POINT ( 'NONE',  ( -5.766373805197273938, -287.5669366634023163, -340.2502536075998592 ) ) ;
#31231 = DIRECTION ( 'NONE',  ( -0.000000000000000000, -1.000000000000000000, -0.000000000000000000 ) ) ;
#31232 = CARTESIAN_POINT ( 'NONE',  ( -90.97476348873112784, -297.4292653437055378, -321.1292158681425235 ) ) ;
#31233 = CARTESIAN_POINT ( 'NONE',  ( -99.97205941160669340, -279.3942942482120202, -314.1337622856285066 ) ) ;
#31235 = CARTESIAN_POINT ( 'NONE',  ( -37.00397014956839570, -279.7232146820932712, -197.3407548956787707 ) ) ;
#31234 = CARTESIAN_POINT ( 'NONE',  ( -44.66149869112747695, -293.1643213388960021, -345.4122336924806405 ) ) ;
#31236 = CARTESIAN_POINT ( 'NONE',  ( -40.63454460683927039, -292.1785230287092077, -193.4183759349064644 ) ) ;
#31237 = CARTESIAN_POINT ( 'NONE',  ( -92.84503817647167523, -283.3441119471802949, -219.0136775605955393 ) ) ;
#31238 = CARTESIAN_POINT ( 'NONE',  ( -53.67034497485278166, -279.2617067203428292, -343.6152644030746046 ) ) ;
#31239 = CARTESIAN_POINT ( 'NONE',  ( -26.18334357592893724, -293.9653473019334342, -342.7413606365951750 ) ) ;
#31240 = CARTESIAN_POINT ( 'NONE',  ( -96.35744694540538546, -271.1898637039643631, -223.8082441841174841 ) ) ;
#31241 = ORIENTED_EDGE ( 'NONE', *, *, #89572, .T. ) ;
#31242 = CARTESIAN_POINT ( 'NONE',  ( 186.6539576904058890, 293.9636489450775230, 0.000000000000000000 ) ) ;
#31243 = CARTESIAN_POINT ( 'NONE',  ( 35.84830915361725800, -283.7220711181074080, -285.0907916521785523 ) ) ;
#31244 = CARTESIAN_POINT ( 'NONE',  ( -96.46189878924629113, -295.4592979281346743, -313.3102106603600987 ) ) ;
#31245 = PLANE ( 'NONE',  #14179 ) ;
#31246 = CARTESIAN_POINT ( 'NONE',  ( 35.78497577281001440, -272.8380690714490129, -253.7030783399848985 ) ) ;
#31247 = CARTESIAN_POINT ( 'NONE',  ( 9.420182046173946944, -273.8739431225682210, -209.3899346618975983 ) ) ;
#31248 = CARTESIAN_POINT ( 'NONE',  ( -17.83380835474038051, -290.1208522788536470, -344.3390905827596953 ) ) ;
#31249 = CARTESIAN_POINT ( 'NONE',  ( -97.35011842549882033, -289.8060457459617396, -311.9521759493230775 ) ) ;
#31250 = CARTESIAN_POINT ( 'NONE',  ( -68.83701028284195900, -281.1504719300153283, -203.7371493759753491 ) ) ;
#31251 = CARTESIAN_POINT ( 'NONE',  ( -34.45244230781214867, -299.8489447999542108, -196.3468973494859995 ) ) ;
#31252 = CARTESIAN_POINT ( 'NONE',  ( 0.6183820539838543739, -279.3649575833840117, -207.4837887910809116 ) ) ;
#31253 = ORIENTED_EDGE ( 'NONE', *, *, #87350, .F. ) ;
#31254 = CARTESIAN_POINT ( 'NONE',  ( 7.236718122286518451, -274.4741414487317002, -207.5122079605968679 ) ) ;
#31255 = CARTESIAN_POINT ( 'NONE',  ( -68.42432604560799803, -293.5607539032566820, -202.7069995643404354 ) ) ;
#31256 = DIRECTION ( 'NONE',  ( -0.000000000000000000, -1.000000000000000000, -0.000000000000000000 ) ) ;
#31257 = CARTESIAN_POINT ( 'NONE',  ( -107.8218623798989739, -290.9453473960938368, -289.9496252828471938 ) ) ;
#31258 = DIRECTION ( 'NONE',  ( -0.000000000000000000, -1.000000000000000000, -0.000000000000000000 ) ) ;
#31259 = EDGE_CURVE ( 'NONE', #40445, #42785, #14755, .T. ) ;
#31260 = CARTESIAN_POINT ( 'NONE',  ( -41.95470197703103565, -290.1341792296234416, -194.7368778520182104 ) ) ;
#31261 = CARTESIAN_POINT ( 'NONE',  ( -47.27142345842409554, -297.5893604061282076, -197.9670419624538908 ) ) ;
#31262 = DIRECTION ( 'NONE',  ( 1.000000000000000000, -0.000000000000000000, -0.000000000000000000 ) ) ;
#31263 = CARTESIAN_POINT ( 'NONE',  ( -104.0136727477975427, -292.5577853298449895, -233.2456789020233714 ) ) ;
#31264 = CARTESIAN_POINT ( 'NONE',  ( 36.57525178469696669, -295.6233781216987495, -234.7283546768995564 ) ) ;
#31265 = CARTESIAN_POINT ( 'NONE',  ( 8.018469824741391250, -288.6734769092363990, -210.7768981873759628 ) ) ;
#31266 = CARTESIAN_POINT ( 'NONE',  ( 17.86692047987866516, -274.2591556020927328, -320.8979091396874423 ) ) ;
#31267 = CARTESIAN_POINT ( 'NONE',  ( 32.46028268355424728, -277.1340675933158195, -244.4961340879069951 ) ) ;
#31268 = CARTESIAN_POINT ( 'NONE',  ( -14.37942983481254977, -290.4320455851233191, -199.5511727832560496 ) ) ;
#31269 = CARTESIAN_POINT ( 'NONE',  ( -58.97252696514448900, -281.6356091029114737, -197.7497358952096533 ) ) ;
#31270 = ORIENTED_EDGE ( 'NONE', *, *, #32042, .T. ) ;
#31271 = CARTESIAN_POINT ( 'NONE',  ( -16.11080883092867566, -282.1188305920303492, -340.3121145634739264 ) ) ;
#31272 = CARTESIAN_POINT ( 'NONE',  ( -56.83214239136744084, -278.3773058576832113, -344.5888202230518687 ) ) ;
#31273 = CARTESIAN_POINT ( 'NONE',  ( 27.95844798005542486, -280.8742149126379672, -310.5103224392374273 ) ) ;
#31274 = CARTESIAN_POINT ( 'NONE',  ( -99.45230775254184152, -278.8927673148161261, -315.4954661341138831 ) ) ;
#31275 = EDGE_CURVE ( 'NONE', #3784, #73161, #87399, .T. ) ;
#31277 = EDGE_CURVE ( 'NONE', #78077, #59807, #16883, .T. ) ;
#31276 = APPLICATION_PROTOCOL_DEFINITION ( 'draft international standard', 'automotive_design', 1998, #89796 ) ;
#31278 = CARTESIAN_POINT ( 'NONE',  ( -10.60881529658629496, -275.9146046465056656, -198.8342137008324073 ) ) ;
#31279 = CARTESIAN_POINT ( 'NONE',  ( -21.39648532958013050, -282.7662352645559167, -200.3538533559491555 ) ) ;
#31280 = ORIENTED_EDGE ( 'NONE', *, *, #10209, .T. ) ;
#31281 = CARTESIAN_POINT ( 'NONE',  ( -101.6237757677808986, -299.0709051315496936, -231.6230966172172430 ) ) ;
#31282 = CARTESIAN_POINT ( 'NONE',  ( -80.57877697352100199, -290.7333530767123193, -329.6254709182156262 ) ) ;
#31283 = CARTESIAN_POINT ( 'NONE',  ( -9.395449196819786408, -274.7052185775245903, -339.5909813700837390 ) ) ;
#31284 = CARTESIAN_POINT ( 'NONE',  ( -68.91552868352297878, -291.2217299888569642, -339.4916815754901336 ) ) ;
#31285 = CARTESIAN_POINT ( 'NONE',  ( -83.88756866074173502, -290.7414634574321894, -213.9929107166604467 ) ) ;
#31286 = CARTESIAN_POINT ( 'NONE',  ( 7.893261822244963533, -287.9604855583655194, -332.6628565060133838 ) ) ;
#31287 = CARTESIAN_POINT ( 'NONE',  ( 200.8419735307467420, 26.78103457774644269, 8.999999999999998224 ) ) ;
#31288 = CARTESIAN_POINT ( 'NONE',  ( -111.0256223141635701, -283.0168666224920457, -265.3912475153069863 ) ) ;
#31289 = CARTESIAN_POINT ( 'NONE',  ( -101.3573071612549228, -291.9038145931454551, -308.0504411687865627 ) ) ;
#31290 = CARTESIAN_POINT ( 'NONE',  ( -72.68973029123750962, -284.0549842843161628, -205.6843793963161886 ) ) ;
#31291 = CARTESIAN_POINT ( 'NONE',  ( 34.81525019566386447, -282.6836656551529359, -256.3443409853006187 ) ) ;
#31292 = CARTESIAN_POINT ( 'NONE',  ( 10.09199640086744587, -289.3579276242612082, -330.7848990320379130 ) ) ;
#31293 = CARTESIAN_POINT ( 'NONE',  ( -99.52339878206137769, -279.5741387030121246, -231.9054346753736411 ) ) ;
#31294 = CARTESIAN_POINT ( 'NONE',  ( 20.09121300513437447, -291.6569570679810681, -219.6513636628694428 ) ) ;
#31295 = CARTESIAN_POINT ( 'NONE',  ( 37.55992325945679511, -288.1394652339694744, -253.1590818707464337 ) ) ;
#31296 = CARTESIAN_POINT ( 'NONE',  ( -80.90852564738108299, -285.9706911173383332, -206.8818360392764930 ) ) ;
#31297 = CARTESIAN_POINT ( 'NONE',  ( -109.1934052502100343, -284.8898934772623761, -257.3937898013255108 ) ) ;
#31298 = ORIENTED_EDGE ( 'NONE', *, *, #61840, .T. ) ;
#31299 = FACE_OUTER_BOUND ( 'NONE', #48421, .T. ) ;
#31300 = CARTESIAN_POINT ( 'NONE',  ( 22.97723650387827732, -294.7913752883952725, -224.4929519617171252 ) ) ;
#31301 = CARTESIAN_POINT ( 'NONE',  ( 22.77371527930553796, -292.8741486487296584, -317.7048016249416378 ) ) ;
#31302 = CARTESIAN_POINT ( 'NONE',  ( 13.88738263509119086, -275.3710236332801173, -322.7670890616820998 ) ) ;
#31303 = CARTESIAN_POINT ( 'NONE',  ( -112.1732452021648641, -296.1225054174698812, -252.6537000746140791 ) ) ;
#31304 = CARTESIAN_POINT ( 'NONE',  ( 14.79322916045861369, -292.7814551397851801, -322.5160201341722654 ) ) ;
#31305 = CARTESIAN_POINT ( 'NONE',  ( -103.6863120016833051, -294.3520135529505524, -303.2850293362074012 ) ) ;
#31306 = CARTESIAN_POINT ( 'NONE',  ( -25.35930366297356287, -293.4132292720378814, -197.8969816658561456 ) ) ;
#31307 = CARTESIAN_POINT ( 'NONE',  ( 31.83630369331150334, -294.9550604965350544, -294.7748942167126529 ) ) ;
#31308 = CARTESIAN_POINT ( 'NONE',  ( 209.4803090767392462, 35.69423656899339647, 15.12480380540109870 ) ) ;
#31309 = CARTESIAN_POINT ( 'NONE',  ( -17.02742956347599801, -292.7904386131637011, -342.7846286132735827 ) ) ;
#31310 = CARTESIAN_POINT ( 'NONE',  ( 194.5881128153457098, -26.00396092263537540, 21.50000000000000000 ) ) ;
#31311 = CARTESIAN_POINT ( 'NONE',  ( 16.19112397825171712, -289.2105433594653050, -320.4117799789893297 ) ) ;
#31312 = CARTESIAN_POINT ( 'NONE',  ( -50.98944473884495210, -279.2056272548633160, -344.4701313819831512 ) ) ;
#31313 = CARTESIAN_POINT ( 'NONE',  ( -100.1487843025347644, -276.7643709037999429, -314.2163217372786335 ) ) ;
#31314 = CARTESIAN_POINT ( 'NONE',  ( -24.16889770465336440, -273.5645834375325194, -194.5456202010801405 ) ) ;
#31315 = CARTESIAN_POINT ( 'NONE',  ( 30.61933368207897033, -280.0346027905635538, -300.8621172427498323 ) ) ;
#31316 = CARTESIAN_POINT ( 'NONE',  ( -99.82135192412037838, -276.3693820378550754, -313.9814518576292812 ) ) ;
#31317 = CARTESIAN_POINT ( 'NONE',  ( -108.7823309496259583, -295.0102832051042014, -287.6618377572248733 ) ) ;
#31318 = CARTESIAN_POINT ( 'NONE',  ( -109.9191433715138260, -274.7976242761124013, -251.2551911447443160 ) ) ;
#31319 = CARTESIAN_POINT ( 'NONE',  ( -97.93232411612436294, -273.7723056108166588, -229.3725214794351359 ) ) ;
#31320 = CARTESIAN_POINT ( 'NONE',  ( 194.6773453981025455, 25.62504034132872377, 14.06423177434174399 ) ) ;
#31322 = CARTESIAN_POINT ( 'NONE',  ( -16.63863031486884125, -274.1603750621654854, -200.3056741016278011 ) ) ;
#31321 = CARTESIAN_POINT ( 'NONE',  ( -98.54933269549042052, -287.9767292865842023, -314.3381270416014104 ) ) ;
#31323 = CARTESIAN_POINT ( 'NONE',  ( 24.14220891692059467, -288.1694072093703767, -316.7155021176763512 ) ) ;
#31324 = CARTESIAN_POINT ( 'NONE',  ( -43.18785736984990109, -299.9587091203084697, -195.1809583684856761 ) ) ;
#31325 = CARTESIAN_POINT ( 'NONE',  ( -91.75744731388762432, -293.8295572231668871, -321.8065322391738619 ) ) ;
#31326 = CARTESIAN_POINT ( 'NONE',  ( -18.96693985425484641, -282.0187456948979161, -345.0251203911348057 ) ) ;
#31327 = CARTESIAN_POINT ( 'NONE',  ( 133.0872704186301405, -299.5541904835127980, -201.0153591320744226 ) ) ;
#31328 = CARTESIAN_POINT ( 'NONE',  ( 36.55979728763310987, -279.3868304103137348, -257.4979387412158758 ) ) ;
#31329 = CARTESIAN_POINT ( 'NONE',  ( 193.9646936176702070, 21.00000000000000000, -15.00000000000000000 ) ) ;
#31330 = CARTESIAN_POINT ( 'NONE',  ( -110.0915946498853941, -289.4796095885238287, -260.2593394080383860 ) ) ;
#31331 = CARTESIAN_POINT ( 'NONE',  ( -111.5546622729918340, -282.6488063448979915, -273.6699567034181655 ) ) ;
#31332 = FACE_OUTER_BOUND ( 'NONE', #55099, .T. ) ;
#31333 = LINE ( 'NONE', #44590, #62460 ) ;
#31334 = CARTESIAN_POINT ( 'NONE',  ( -112.3065576144171303, -288.5055117251473575, -273.9807582936405197 ) ) ;
#31335 = CARTESIAN_POINT ( 'NONE',  ( 21.22083368778951140, -276.4488238660761112, -225.6062794130096734 ) ) ;
#31336 = CARTESIAN_POINT ( 'NONE',  ( -41.53198949850408894, -284.3087552535243390, -346.9014108187861893 ) ) ;
#31338 = CARTESIAN_POINT ( 'NONE',  ( -108.0286609912364781, -284.7928116850294487, -252.1305512351773075 ) ) ;
#31337 = CARTESIAN_POINT ( 'NONE',  ( -24.38207594446435067, -272.2960468025480623, -195.8676344309231752 ) ) ;
#31339 = CARTESIAN_POINT ( 'NONE',  ( 27.29290080409853303, -277.4550709852956061, -305.6492667356996549 ) ) ;
#31340 = CARTESIAN_POINT ( 'NONE',  ( -59.23359976853490849, -278.1457360501477751, -340.1704759280403891 ) ) ;
#31341 = ADVANCED_FACE ( 'NONE', ( #44782 ), #15449, .F. ) ;
#31342 = CARTESIAN_POINT ( 'NONE',  ( 3.479076350669284778, -284.5038572347049239, -333.3404328310936648 ) ) ;
#31343 = VERTEX_POINT ( 'NONE', #66581 ) ;
#31344 = CYLINDRICAL_SURFACE ( 'NONE', #58876, 0.5000000000000004441 ) ;
#31345 = CARTESIAN_POINT ( 'NONE',  ( -84.18688560425368905, -295.5093345531158207, -331.5391345022632663 ) ) ;
#31346 = CARTESIAN_POINT ( 'NONE',  ( -5.110769517629338843, -288.4583207594378109, -203.0193643251922992 ) ) ;
#31347 = CARTESIAN_POINT ( 'NONE',  ( 196.9925019505417083, 24.91416401846167261, 12.94510111180389167 ) ) ;
#31348 = CARTESIAN_POINT ( 'NONE',  ( -19.11405058567864046, -286.3380690714489560, -350.3683826091709648 ) ) ;
#31349 = CARTESIAN_POINT ( 'NONE',  ( -113.4611929476531174, -277.3498624389717975, -280.1264454285906140 ) ) ;
#31350 = CARTESIAN_POINT ( 'NONE',  ( -105.2815048512349563, -289.4022704879004095, -235.7394253883467456 ) ) ;
#31351 = CARTESIAN_POINT ( 'NONE',  ( -57.60342536166332650, -287.3060447177883248, -199.4548406257005411 ) ) ;
#31352 = CARTESIAN_POINT ( 'NONE',  ( -98.84803361238770947, -280.8773303680115419, -229.1003657316499869 ) ) ;
#31353 = CARTESIAN_POINT ( 'NONE',  ( -37.99575236323442340, -287.4693738490169608, -193.9531438499307683 ) ) ;
#31354 = CARTESIAN_POINT ( 'NONE',  ( -36.13653011754616529, -285.0371959870591922, -345.3514388110838809 ) ) ;
#31355 = CARTESIAN_POINT ( 'NONE',  ( 38.18278396775849615, -275.9064488567860849, -285.3628614340199192 ) ) ;
#31356 = CARTESIAN_POINT ( 'NONE',  ( 98.17144688861017698, -297.7765669504339598, -195.7623448073262864 ) ) ;
#31357 = CARTESIAN_POINT ( 'NONE',  ( -111.7304775296174739, -278.6349930195842148, -250.4278200547514075 ) ) ;
#31358 = CARTESIAN_POINT ( 'NONE',  ( -111.1675577024199839, -298.6008049307869783, -260.4283685838656766 ) ) ;
#31359 = CARTESIAN_POINT ( 'NONE',  ( 159.4851178187871312, 14.99999999999999645, 10.00000000000000178 ) ) ;
#31360 = CARTESIAN_POINT ( 'NONE',  ( 10.64812456238590066, -278.9090924074130839, -330.4860931364851808 ) ) ;
#31361 = CARTESIAN_POINT ( 'NONE',  ( -111.4499704650455811, -271.0048131427265616, -253.5700999803765967 ) ) ;
#31362 = LINE ( 'NONE', #81526, #57664 ) ;
#31363 = CARTESIAN_POINT ( 'NONE',  ( -66.83324651431099994, -276.9570053283635502, -337.2059916346631212 ) ) ;
#31364 = CARTESIAN_POINT ( 'NONE',  ( 21.53577255653188161, -276.0946615466802427, -221.3565066662580705 ) ) ;
#31365 = CARTESIAN_POINT ( 'NONE',  ( 38.56391707517012435, -280.4629069489377002, -258.5636069471576093 ) ) ;
#31366 = CARTESIAN_POINT ( 'NONE',  ( 30.36094334646875481, -289.7107298007793474, -300.3936460072927161 ) ) ;
#31367 = CARTESIAN_POINT ( 'NONE',  ( -113.6448539439465151, -298.0815165947082050, -269.6286777872169864 ) ) ;
#31368 = CARTESIAN_POINT ( 'NONE',  ( -110.8300958887223260, -297.4840826714466289, -292.0282776306052597 ) ) ;
#31369 = CARTESIAN_POINT ( 'NONE',  ( 35.42463123688356319, -295.3268785481492387, -252.8396441722057659 ) ) ;
#31370 = CARTESIAN_POINT ( 'NONE',  ( 37.35128208426909424, -279.4930349272282797, -265.7799792356038893 ) ) ;
#31371 = CARTESIAN_POINT ( 'NONE',  ( -34.27806860675843126, -282.0110912056253483, -195.9713925258860172 ) ) ;
#31372 = CARTESIAN_POINT ( 'NONE',  ( -33.69993651244328703, -296.1779303398994898, -195.9223127172270438 ) ) ;
#31373 = CARTESIAN_POINT ( 'NONE',  ( -103.3576731478390798, -286.6533841931981783, -232.1991869681958747 ) ) ;
#31374 = CARTESIAN_POINT ( 'NONE',  ( -37.28150989865982723, -287.9717079146420815, -343.6702064497233664 ) ) ;
#31375 = CARTESIAN_POINT ( 'NONE',  ( -62.00093947437260056, -183.6896612128238928, -362.0872038736079617 ) ) ;
#31376 = ORIENTED_EDGE ( 'NONE', *, *, #54639, .F. ) ;
#31377 = CARTESIAN_POINT ( 'NONE',  ( 21.02709260368700939, -286.7963858990431731, -319.6732902074080584 ) ) ;
#31378 = CARTESIAN_POINT ( 'NONE',  ( -9.481395755719859153, -286.0932452481566202, -202.8502656237699853 ) ) ;
#31379 = ORIENTED_EDGE ( 'NONE', *, *, #14648, .T. ) ;
#31380 = CARTESIAN_POINT ( 'NONE',  ( -93.19694380638489406, -284.9114449797202155, -322.9320957600143629 ) ) ;
#31381 = CARTESIAN_POINT ( 'NONE',  ( -8.966531441369978594, -274.7669419603913639, -203.0246740735224193 ) ) ;
#31382 = CARTESIAN_POINT ( 'NONE',  ( -98.94804093791375976, -290.0823899216254063, -224.6647188990842210 ) ) ;
#31383 = CARTESIAN_POINT ( 'NONE',  ( -5.490159567272129948, -283.2954408411344502, -340.3524899572649929 ) ) ;
#31384 = CARTESIAN_POINT ( 'NONE',  ( -7.823235954678832371, -281.9520960981986377, -199.9809875617134196 ) ) ;
#31385 = CARTESIAN_POINT ( 'NONE',  ( 8.530534332706116274, -280.9942639501025496, -208.4767199512577918 ) ) ;
#31386 = CARTESIAN_POINT ( 'NONE',  ( -49.14190916843124057, -279.8975725031252750, -198.3211633281875095 ) ) ;
#31387 = CARTESIAN_POINT ( 'NONE',  ( -69.91165696735023971, -274.9809262143061233, -337.9199732462171255 ) ) ;
#31388 = CARTESIAN_POINT ( 'NONE',  ( -63.20851169538713066, -183.0927275039082929, -362.5798909104344148 ) ) ;
#31389 = ORIENTED_EDGE ( 'NONE', *, *, #63818, .T. ) ;
#31390 = CARTESIAN_POINT ( 'NONE',  ( 29.48737834821474380, -277.1064677590645147, -236.6876463258043657 ) ) ;
#31391 = CARTESIAN_POINT ( 'NONE',  ( 160.2970747563815053, 220.5528797148367914, -204.9019708605778192 ) ) ;
#31392 = CARTESIAN_POINT ( 'NONE',  ( 22.30946005225842654, -280.1887542401478868, -315.2552285546606754 ) ) ;
#31393 = CARTESIAN_POINT ( 'NONE',  ( -40.51410305601200434, -297.3598283656597800, -197.3154870207346505 ) ) ;
#31394 = CARTESIAN_POINT ( 'NONE',  ( 11.08492328142546057, -292.2094548641217671, -210.5063748351800257 ) ) ;
#31395 = CARTESIAN_POINT ( 'NONE',  ( 174.1105135456895141, 240.3386868887248511, -177.2113801460971558 ) ) ;
#31397 = CARTESIAN_POINT ( 'NONE',  ( -18.28637951969112407, -287.2024918181344901, -341.7117878292757496 ) ) ;
#31396 = CARTESIAN_POINT ( 'NONE',  ( 75.32416697583983023, -298.0113065177353064, -193.9769740307470727 ) ) ;
#31398 = CARTESIAN_POINT ( 'NONE',  ( -105.0537192503782080, -298.0080034793483605, -300.9160769104076394 ) ) ;
#31399 = CARTESIAN_POINT ( 'NONE',  ( -11.86663911566776441, -287.7060512650919009, -201.4244459977876716 ) ) ;
#31400 = ORIENTED_EDGE ( 'NONE', *, *, #80190, .F. ) ;
#31401 = CARTESIAN_POINT ( 'NONE',  ( 36.47459659255399345, -294.2279168117560744, -249.2425444003685868 ) ) ;
#31402 = CARTESIAN_POINT ( 'NONE',  ( -105.6246715811924872, -285.3912006289635883, -244.3721924357102750 ) ) ;
#31403 = CARTESIAN_POINT ( 'NONE',  ( -36.88430695734270159, -296.8526895307199993, -193.7582787832450606 ) ) ;
#31404 = CARTESIAN_POINT ( 'NONE',  ( -5.962255238215237618, -293.2570323792476188, -200.2077897503053521 ) ) ;
#31405 = EDGE_CURVE ( 'NONE', #26494, #44526, #270, .T. ) ;
#31406 = CARTESIAN_POINT ( 'NONE',  ( 36.64325970093131701, -293.7790845188023354, -249.2002724160592209 ) ) ;
#31407 = CARTESIAN_POINT ( 'NONE',  ( -48.05888581371884527, -289.3588382067932798, -342.6211554911231474 ) ) ;
#31408 = VERTEX_POINT ( 'NONE', #11015 ) ;
#31409 = CARTESIAN_POINT ( 'NONE',  ( 158.9078607026168868, 17.25638377771124965, 9.432942837125230184 ) ) ;
#31410 = CARTESIAN_POINT ( 'NONE',  ( -4.110268410051605592, -300.3243722564834002, -194.5859091532147147 ) ) ;
#31411 = CARTESIAN_POINT ( 'NONE',  ( -55.22595221914062336, -272.6219663342944273, -195.8751310816175817 ) ) ;
#31412 = EDGE_CURVE ( 'NONE', #82273, #18551, #27504, .T. ) ;
#31413 = CARTESIAN_POINT ( 'NONE',  ( 7.930036280584154440, -281.4751049847474178, -327.9921712432815184 ) ) ;
#31414 = EDGE_LOOP ( 'NONE', ( #28558, #36122, #87979, #22156 ) ) ;
#31415 = ORIENTED_EDGE ( 'NONE', *, *, #79046, .T. ) ;
#31416 = CARTESIAN_POINT ( 'NONE',  ( -62.39188600105975269, -276.8770022920694487, -343.1636206328474259 ) ) ;
#31417 = CARTESIAN_POINT ( 'NONE',  ( -109.3105731355164210, -271.1652082560592589, -254.0233783641224647 ) ) ;
#31418 = CARTESIAN_POINT ( 'NONE',  ( -110.3511368125342074, -280.5868456490927088, -256.9265492439108698 ) ) ;
#31419 = CARTESIAN_POINT ( 'NONE',  ( -0.8839295421733401881, -274.7026093141018919, -335.0853164081544264 ) ) ;
#31420 = CARTESIAN_POINT ( 'NONE',  ( -86.37690161627159569, -298.5581431460211093, -215.7472047472665793 ) ) ;
#31421 = CARTESIAN_POINT ( 'NONE',  ( -92.20234635300101900, -274.1843029003908896, -221.8459868964510235 ) ) ;
#31422 = CARTESIAN_POINT ( 'NONE',  ( -112.4121267558787594, -297.9833166610093258, -283.7306166818533484 ) ) ;
#31423 = CARTESIAN_POINT ( 'NONE',  ( -62.97341230813007229, -271.7401380474320831, -199.4991244121179648 ) ) ;
#31424 = CARTESIAN_POINT ( 'NONE',  ( 35.39587545370003596, -294.1011036362260711, -262.5828358792764448 ) ) ;
#31425 = CARTESIAN_POINT ( 'NONE',  ( 11.33404425929101045, -291.3168758948906429, -215.1021025869179653 ) ) ;
#31426 = CARTESIAN_POINT ( 'NONE',  ( 193.8296338041434126, 214.9642006536927852, 17.09991073265190309 ) ) ;
#31427 = CARTESIAN_POINT ( 'NONE',  ( 31.80273434438988289, -276.4794517932647864, -304.2252508412464067 ) ) ;
#31428 = CARTESIAN_POINT ( 'NONE',  ( -59.47766265483444670, -273.9242104854262720, -200.7452806851144089 ) ) ;
#31429 = CARTESIAN_POINT ( 'NONE',  ( -68.99779512676353477, -282.1446124273924738, -340.0259254832058105 ) ) ;
#31430 = CARTESIAN_POINT ( 'NONE',  ( 5.588328626319332137, -296.4728186242994639, -332.1257779332538576 ) ) ;
#31431 = CARTESIAN_POINT ( 'NONE',  ( 219.8344101925596021, 3.000000000000000000, -9.000000000000001776 ) ) ;
#31432 = CARTESIAN_POINT ( 'NONE',  ( -91.79204827701150293, -283.0513426822056999, -319.2446967486595781 ) ) ;
#31433 = CARTESIAN_POINT ( 'NONE',  ( -19.38173125664873098, -280.8216104470338337, -343.4042685941485615 ) ) ;
#31434 = CARTESIAN_POINT ( 'NONE',  ( 5.727060680011258675, -275.0307334462215749, -330.0935966042761152 ) ) ;
#31435 = CARTESIAN_POINT ( 'NONE',  ( 36.77616498652003685, -283.4039849914132674, -258.8089732207753855 ) ) ;
#31436 = FACE_OUTER_BOUND ( 'NONE', #3635, .T. ) ;
#31437 = CARTESIAN_POINT ( 'NONE',  ( 175.2296996224750103, 133.0000000000000000, -24.00000000000001066 ) ) ;
#31438 = CARTESIAN_POINT ( 'NONE',  ( -1.657897437980451638, -272.9169497584712190, -203.0327685112679603 ) ) ;
#31439 = CARTESIAN_POINT ( 'NONE',  ( -96.47058215272042503, -279.9167293225235653, -316.7702091354408935 ) ) ;
#31440 = CARTESIAN_POINT ( 'NONE',  ( 154.1415209985679269, 20.37991841447901820, -11.45812909362559040 ) ) ;
#31441 = CARTESIAN_POINT ( 'NONE',  ( -66.65344565458198645, -287.5913188514035710, -200.7182018045904499 ) ) ;
#31442 = CARTESIAN_POINT ( 'NONE',  ( 157.7437329832428077, 18.12362412296337411, -11.08836552221236538 ) ) ;
#31443 = CARTESIAN_POINT ( 'NONE',  ( -71.80289454216593015, -289.5965874161616966, -203.7329695588857987 ) ) ;
#31444 = DIRECTION ( 'NONE',  ( 0.000000000000000000, 0.000000000000000000, -1.000000000000000000 ) ) ;
#31445 = CARTESIAN_POINT ( 'NONE',  ( -109.1645180587833721, -295.5462285602326347, -255.1807846526926085 ) ) ;
#31446 = CARTESIAN_POINT ( 'NONE',  ( -48.26576599665141742, -287.3320686382022586, -343.8400452356967776 ) ) ;
#31447 = CARTESIAN_POINT ( 'NONE',  ( -33.93809357080956346, -124.0300793293349244, -358.8670080828285336 ) ) ;
#31448 = CARTESIAN_POINT ( 'NONE',  ( -50.27442350059632048, -295.8868865789812617, -196.4845634323208685 ) ) ;
#31449 = CARTESIAN_POINT ( 'NONE',  ( 22.72955719232091809, -286.6669441281401305, -317.4369254192948802 ) ) ;
#31450 = CARTESIAN_POINT ( 'NONE',  ( 21.13749052054649624, -282.5253132608652322, -225.3225386360151674 ) ) ;
#31451 = CARTESIAN_POINT ( 'NONE',  ( -80.99794473902790060, -281.8754884775376013, -332.6192447034292741 ) ) ;
#31452 = CARTESIAN_POINT ( 'NONE',  ( -87.93059018348077416, -291.3209759682179651, -217.6627103320107892 ) ) ;
#31453 = CARTESIAN_POINT ( 'NONE',  ( 21.49183279404825697, -283.5933680662857910, -314.5859102448242766 ) ) ;
#31454 = CARTESIAN_POINT ( 'NONE',  ( 12.03317942220703785, -283.1470862150221706, -324.3492925763025596 ) ) ;
#31455 = CARTESIAN_POINT ( 'NONE',  ( -74.82320468229929133, -291.5285159201268925, -335.7334639684534068 ) ) ;
#31456 = CARTESIAN_POINT ( 'NONE',  ( -111.0181294507624870, -273.1675587053790082, -247.8735358820989916 ) ) ;
#31457 = EDGE_LOOP ( 'NONE', ( #8232, #83885, #22381, #81907, #70861 ) ) ;
#31458 = CARTESIAN_POINT ( 'NONE',  ( -59.62635283859822266, -287.4184195001796525, -342.5602069620944121 ) ) ;
#31459 = CARTESIAN_POINT ( 'NONE',  ( 36.88562052154607329, -275.8092279621046714, -290.8872163294952315 ) ) ;
#31460 = CARTESIAN_POINT ( 'NONE',  ( 27.65462333698635078, -295.0394239356660933, -233.5497195466952576 ) ) ;
#31461 = DIRECTION ( 'NONE',  ( 0.000000000000000000, 0.000000000000000000, 1.000000000000000000 ) ) ;
#31462 = CARTESIAN_POINT ( 'NONE',  ( -69.91165696735023971, -288.1233781216987495, -202.8022627189028810 ) ) ;
#31463 = ADVANCED_FACE ( 'NONE', ( #3935 ), #88338, .F. ) ;
#31464 = ADVANCED_FACE ( 'NONE', ( #25691 ), #81887, .F. ) ;
#31465 = DIRECTION ( 'NONE',  ( 0.000000000000000000, 1.000000000000000000, 0.000000000000000000 ) ) ;
#31466 = CARTESIAN_POINT ( 'NONE',  ( -34.06901696572148808, -296.4923565346082910, -194.1619862224283963 ) ) ;
#31467 = CARTESIAN_POINT ( 'NONE',  ( -32.12080932589464055, -293.7192026483698442, -196.7332609505925802 ) ) ;
#31468 = CARTESIAN_POINT ( 'NONE',  ( -14.02508717325673615, -273.7113827915954971, -201.0774386031104086 ) ) ;
#31469 = CARTESIAN_POINT ( 'NONE',  ( -90.32816228578657558, -292.8053666004113325, -219.1444939209810059 ) ) ;
#31470 = CARTESIAN_POINT ( 'NONE',  ( -81.88161658258529485, -292.3697966766944205, -212.1625740438936134 ) ) ;
#31471 = CARTESIAN_POINT ( 'NONE',  ( -84.30796038583113727, -287.1562652393751023, -213.0918503038076892 ) ) ;
#31472 = CARTESIAN_POINT ( 'NONE',  ( -50.48299935605892585, -293.3127650641675359, -195.0888618316279235 ) ) ;
#31473 = CARTESIAN_POINT ( 'NONE',  ( -86.21098281291396859, -292.7060542423684524, -211.4272894462813213 ) ) ;
#31474 = CARTESIAN_POINT ( 'NONE',  ( -20.85023846380252621, -294.6679889053587544, -341.5260319559981781 ) ) ;
#31475 = CARTESIAN_POINT ( 'NONE',  ( 23.60226443846766387, -288.9565606166154339, -226.5605124199157103 ) ) ;
#31476 = CARTESIAN_POINT ( 'NONE',  ( 25.10853272907954192, -282.3163307100768975, -315.4275724825068323 ) ) ;
#31477 = CARTESIAN_POINT ( 'NONE',  ( -90.60283952281481845, -295.3843222647720950, -216.7648006912653500 ) ) ;
#31478 = CARTESIAN_POINT ( 'NONE',  ( -114.3265517440705850, -284.4261035551376153, -267.1122898648237083 ) ) ;
#31479 = CARTESIAN_POINT ( 'NONE',  ( 32.81615884907151326, -277.8659331739482923, -296.0011001146751823 ) ) ;
#31480 = CARTESIAN_POINT ( 'NONE',  ( -94.60438968308704943, -282.7015653039973131, -316.2953292274448245 ) ) ;
#31481 = CARTESIAN_POINT ( 'NONE',  ( 14.92417007275667906, -284.7889119931800792, -216.5719047580091967 ) ) ;
#31482 = CARTESIAN_POINT ( 'NONE',  ( -31.56841561323425793, -275.1197215282965658, -345.9574184079501720 ) ) ;
#31483 = CARTESIAN_POINT ( 'NONE',  ( 208.4306832106270804, -199.2391364535880882, 6.499999999999977796 ) ) ;
#31484 = CARTESIAN_POINT ( 'NONE',  ( -95.97487510789744647, -283.4488949960186233, -313.9517045076565864 ) ) ;
#31485 = CARTESIAN_POINT ( 'NONE',  ( -110.9599172156418234, -280.0240787768369159, -249.1864436785759835 ) ) ;
#31486 = CARTESIAN_POINT ( 'NONE',  ( 22.81500075064044708, -285.9706276463091967, -222.6537746429988545 ) ) ;
#31487 = CARTESIAN_POINT ( 'NONE',  ( 30.42676385983788734, -295.7071143573116956, -300.1169459792799330 ) ) ;
#31488 = CARTESIAN_POINT ( 'NONE',  ( -25.87008381219308717, -278.5084972166658872, -345.6926680327092640 ) ) ;
#31489 = CARTESIAN_POINT ( 'NONE',  ( 39.13128916600017959, -276.9131735701977846, -274.0036748556526618 ) ) ;
#31490 = CARTESIAN_POINT ( 'NONE',  ( -32.42267914001488549, -276.8218678416092757, -343.2451645309615174 ) ) ;
#31491 = CARTESIAN_POINT ( 'NONE',  ( -80.81323830243850637, -299.4608118150424048, -209.4492653379770104 ) ) ;
#31492 = CARTESIAN_POINT ( 'NONE',  ( 35.47938801786849439, -285.7738233037552504, -287.5982161197611049 ) ) ;
#31493 = CARTESIAN_POINT ( 'NONE',  ( -109.6779848185424271, -292.4588604657840847, -246.2395989081465757 ) ) ;
#31494 = CARTESIAN_POINT ( 'NONE',  ( 12.55524525566281824, -293.2576136460835414, -324.1384175559534810 ) ) ;
#31495 = ORIENTED_EDGE ( 'NONE', *, *, #26993, .T. ) ;
#31496 = CARTESIAN_POINT ( 'NONE',  ( 33.66932302133138677, -292.9938145533351417, -253.2923385062885302 ) ) ;
#31497 = ORIENTED_EDGE ( 'NONE', *, *, #17827, .T. ) ;
#31498 = CARTESIAN_POINT ( 'NONE',  ( -17.78981403259718519, -289.8853875712802051, -344.5178186846274571 ) ) ;
#31499 = CARTESIAN_POINT ( 'NONE',  ( -99.55884111655753088, -279.7331790903643878, -231.8858920068892928 ) ) ;
#31500 = CARTESIAN_POINT ( 'NONE',  ( -110.5140328788520208, -295.7641767339590615, -247.2221190868052076 ) ) ;
#31501 = CARTESIAN_POINT ( 'NONE',  ( 16.22223479531319512, -287.4400584448364953, -215.1866885617002083 ) ) ;
#31502 = CARTESIAN_POINT ( 'NONE',  ( -36.08293038156391930, -289.3700871971960851, -347.3427883231039459 ) ) ;
#31504 = CARTESIAN_POINT ( 'NONE',  ( -71.41498665744305185, -283.8485688112849630, -334.9451611505753590 ) ) ;
#31503 = VECTOR ( 'NONE', #14274, 1000.000000000000000 ) ;
#31505 = CARTESIAN_POINT ( 'NONE',  ( 185.1013737608651013, 263.7048346170037689, -153.2992251502632541 ) ) ;
#31506 = CARTESIAN_POINT ( 'NONE',  ( 137.2480117259403585, 180.4972570205891884, -240.1171119101352360 ) ) ;
#31507 = CARTESIAN_POINT ( 'NONE',  ( 198.0687835817796270, 286.2794921413739644, -96.29896154386530327 ) ) ;
#31508 = CARTESIAN_POINT ( 'NONE',  ( -5.003894491223660701, -275.8123695864867955, -336.0017711361109605 ) ) ;
#31509 = CARTESIAN_POINT ( 'NONE',  ( -106.5606084506377158, -277.1508379602009313, -294.6599019257305372 ) ) ;
#31510 = CARTESIAN_POINT ( 'NONE',  ( -96.00881876065979270, -272.8911064653503900, -220.5019487167899683 ) ) ;
#31511 = CARTESIAN_POINT ( 'NONE',  ( -20.25196880903670760, -109.6380444505058875, -360.0496258023737255 ) ) ;
#31512 = CARTESIAN_POINT ( 'NONE',  ( -45.61305577217230933, -275.8395903467039147, -346.4722550337872349 ) ) ;
#31513 = ORIENTED_EDGE ( 'NONE', *, *, #63164, .F. ) ;
#31514 = CARTESIAN_POINT ( 'NONE',  ( -102.8978902630445162, -290.6078008813500446, -302.6159529138357129 ) ) ;
#31515 = CARTESIAN_POINT ( 'NONE',  ( -73.21436098207674092, -298.3920489143060877, -202.3515921096798991 ) ) ;
#31516 = CARTESIAN_POINT ( 'NONE',  ( 35.76666439674846742, -286.1385583460980229, -262.8504246756956491 ) ) ;
#31517 = CARTESIAN_POINT ( 'NONE',  ( -73.90372298529642592, -274.2314020529892673, -202.6518564366450619 ) ) ;
#31518 = CARTESIAN_POINT ( 'NONE',  ( -7.986360240581060310, -294.8232467900217557, -337.2122899830308143 ) ) ;
#31519 = ORIENTED_EDGE ( 'NONE', *, *, #11007, .F. ) ;
#31520 = CARTESIAN_POINT ( 'NONE',  ( -39.88943947318689709, -279.0040441156530164, -345.8909794018489379 ) ) ;
#31521 = CARTESIAN_POINT ( 'NONE',  ( 37.13066177362677678, -281.3018527613390347, -289.6845290741199506 ) ) ;
#31522 = CARTESIAN_POINT ( 'NONE',  ( -104.5492971991351396, -279.2382614340767191, -299.7690583863771394 ) ) ;
#31523 = CARTESIAN_POINT ( 'NONE',  ( -111.1850398229012029, -280.0844894610270899, -288.3357977039410684 ) ) ;
#31524 = CARTESIAN_POINT ( 'NONE',  ( -35.10724925903871707, -296.6553866802951802, -196.7724395101816697 ) ) ;
#31525 = DIRECTION ( 'NONE',  ( -0.000000000000000000, -0.000000000000000000, 1.000000000000000000 ) ) ;
#31526 = CARTESIAN_POINT ( 'NONE',  ( -19.53660966853966130, -280.4541412895488293, -199.5134983381287839 ) ) ;
#31527 = CARTESIAN_POINT ( 'NONE',  ( 9.403993259544019878, -275.4793498521829065, -209.3775220758666080 ) ) ;
#31528 = EDGE_CURVE ( 'NONE', #28948, #8050, #76835, .T. ) ;
#31529 = CARTESIAN_POINT ( 'NONE',  ( -49.42284890972417344, -275.8984366434439721, -196.2881265882443245 ) ) ;
#31530 = CARTESIAN_POINT ( 'NONE',  ( -9.443979966876431931, -275.2693160853962695, -341.4970688285294500 ) ) ;
#31531 = DIRECTION ( 'NONE',  ( -0.000000000000000000, -0.000000000000000000, -1.000000000000000000 ) ) ;
#31532 = CARTESIAN_POINT ( 'NONE',  ( -109.4340990374851827, -289.9171451653010081, -257.6106457475736420 ) ) ;
#31533 = CARTESIAN_POINT ( 'NONE',  ( -105.3380788153204861, -284.3663475748666656, -234.3332694592615724 ) ) ;
#31534 = CARTESIAN_POINT ( 'NONE',  ( 36.36364369795897034, -279.6971856230323965, -263.0735535312934985 ) ) ;
#31536 = CARTESIAN_POINT ( 'NONE',  ( -102.2348916860821362, -283.1226445814353383, -233.7838005970184554 ) ) ;
#31535 = CARTESIAN_POINT ( 'NONE',  ( 34.64537128652856524, -279.9262687849906115, -255.0289241323234251 ) ) ;
#31537 = CARTESIAN_POINT ( 'NONE',  ( -105.9124871877583587, -292.1528278534239007, -300.8691199131528151 ) ) ;
#31538 = CARTESIAN_POINT ( 'NONE',  ( -7.853927069331436250, -281.6524336797021419, -203.1342657585906295 ) ) ;
#31539 = CARTESIAN_POINT ( 'NONE',  ( 189.9243309297870610, 275.5000000000000568, 25.22542485937350065 ) ) ;
#31540 = CARTESIAN_POINT ( 'NONE',  ( 6.448440001255717036, -280.8683752031685117, -332.7863864229117326 ) ) ;
#31541 = CARTESIAN_POINT ( 'NONE',  ( 20.75402089830514640, -296.2061393517508350, -317.8142709803955199 ) ) ;
#31542 = CARTESIAN_POINT ( 'NONE',  ( -110.3572456723334625, -277.0593407210012629, -249.3205827328843895 ) ) ;
#31543 = CARTESIAN_POINT ( 'NONE',  ( -26.90155557060899127, -288.1846429851541984, -195.8707869940245132 ) ) ;
#31544 = DIRECTION ( 'NONE',  ( -0.000000000000000000, -1.000000000000000000, -0.000000000000000000 ) ) ;
#31545 = CARTESIAN_POINT ( 'NONE',  ( -85.61225569124820822, -293.3109369479820430, -212.1616937219453121 ) ) ;
#31546 = CARTESIAN_POINT ( 'NONE',  ( 18.91909998922363201, -274.2415484314500986, -319.9760793501604326 ) ) ;
#31547 = CARTESIAN_POINT ( 'NONE',  ( -15.00897166139726835, -287.9673546918364764, -343.9382301464443685 ) ) ;
#31548 = CARTESIAN_POINT ( 'NONE',  ( -37.53177539934910811, -290.4496402685245471, -196.5487794936665011 ) ) ;
#31549 = CARTESIAN_POINT ( 'NONE',  ( -48.18343439339989942, -264.6857882449573935, -436.0815118164402975 ) ) ;
#31550 = CARTESIAN_POINT ( 'NONE',  ( -7.321431726798665274, -275.3347851384361888, -337.4433582877732647 ) ) ;
#31551 = CARTESIAN_POINT ( 'NONE',  ( -53.43993691015518266, -293.4002685872633833, -342.8826839796104764 ) ) ;
#31552 = CARTESIAN_POINT ( 'NONE',  ( -97.74473777446802103, -291.2876605789508062, -312.2486780554531265 ) ) ;
#31553 = CARTESIAN_POINT ( 'NONE',  ( -23.68628624284178130, -44.55766379199612004, 21.50000000000000000 ) ) ;
#31554 = DIRECTION ( 'NONE',  ( 1.000000000000000000, 0.000000000000000000, 0.000000000000000000 ) ) ;
#31555 = CARTESIAN_POINT ( 'NONE',  ( 8.450459310464765394, -291.1459038160550676, -209.2559432353779414 ) ) ;
#31556 = CARTESIAN_POINT ( 'NONE',  ( 26.39715891917249024, -289.6585161460777726, -307.6616315402754367 ) ) ;
#31557 = CARTESIAN_POINT ( 'NONE',  ( -62.45024806280846263, -287.6141186812323554, -342.1352080013635373 ) ) ;
#31558 = CARTESIAN_POINT ( 'NONE',  ( -19.69197021346174736, -287.7088607427220950, -198.9197997599313226 ) ) ;
#31559 = CARTESIAN_POINT ( 'NONE',  ( 82.64890176555634582, -299.5541904835127980, -195.3611179825600175 ) ) ;
#31560 = CARTESIAN_POINT ( 'NONE',  ( 27.17768217025705368, -288.8254375019553208, -304.9631865892729934 ) ) ;
#31561 = CARTESIAN_POINT ( 'NONE',  ( -68.81741396434107116, -297.4437433937206379, -338.8419199787858247 ) ) ;
#31562 = DIRECTION ( 'NONE',  ( 0.000000000000000000, 0.000000000000000000, 1.000000000000000000 ) ) ;
#31563 = CIRCLE ( 'NONE', #4316, 7.500000000000012434 ) ;
#31564 = CARTESIAN_POINT ( 'NONE',  ( 16.01157806488294355, -287.9936317547674776, -215.3935236749062199 ) ) ;
#31565 = CARTESIAN_POINT ( 'NONE',  ( -73.43100056112321283, -275.6068397501877598, -336.7601514665065565 ) ) ;
#31566 = CARTESIAN_POINT ( 'NONE',  ( -84.84999387199226817, -278.0199904630671313, -330.9986935340729701 ) ) ;
#31567 = ORIENTED_EDGE ( 'NONE', *, *, #7026, .F. ) ;
#31568 = CARTESIAN_POINT ( 'NONE',  ( -62.03682781304478056, -279.4065165195858071, -197.3947179004950669 ) ) ;
#31569 = CARTESIAN_POINT ( 'NONE',  ( -36.48437828106663261, -300.0428251152431471, -195.7160183634054533 ) ) ;
#31570 = CARTESIAN_POINT ( 'NONE',  ( -80.43826238227499914, -283.4684023602599154, -208.9158880382875338 ) ) ;
#31571 = CARTESIAN_POINT ( 'NONE',  ( -48.18343439339133027, -260.4667269299101804, -492.5001339377540717 ) ) ;
#31572 = CARTESIAN_POINT ( 'NONE',  ( -65.25903034396264957, -277.8229345540986515, -201.5753043661879644 ) ) ;
#31573 = EDGE_CURVE ( 'NONE', #45087, #29052, #90993, .T. ) ;
#31574 = CARTESIAN_POINT ( 'NONE',  ( -16.71693364395909498, -280.7856996563839402, -342.5233499504229826 ) ) ;
#31575 = DIRECTION ( 'NONE',  ( -1.000000000000000000, 0.000000000000000000, 0.000000000000000000 ) ) ;
#31576 = CARTESIAN_POINT ( 'NONE',  ( -1.807912934046726150, -275.0699185338702932, -337.8893174391120624 ) ) ;
#31577 = CARTESIAN_POINT ( 'NONE',  ( -82.77216404776073944, -297.2060057020833028, -328.4501323682479210 ) ) ;
#31578 = CARTESIAN_POINT ( 'NONE',  ( -10.82188127496737629, -281.6347668122014056, -342.3771860588033178 ) ) ;
#31579 = CARTESIAN_POINT ( 'NONE',  ( -77.65145518012722903, -298.4379283258955411, -209.1566359537868323 ) ) ;
#31580 = CARTESIAN_POINT ( 'NONE',  ( -73.06536452449314822, -298.9043072148883198, -202.6482391785336006 ) ) ;
#31581 = CARTESIAN_POINT ( 'NONE',  ( -6.516195927483879657, -274.1352291704450863, -204.1653796178599407 ) ) ;
#31582 = CARTESIAN_POINT ( 'NONE',  ( 35.72962495944016581, -295.7699498266229625, -287.3169562006386286 ) ) ;
#31583 = CARTESIAN_POINT ( 'NONE',  ( 39.60443700471466144, -287.7696040085465370, -274.4208188855158710 ) ) ;
#31584 = CARTESIAN_POINT ( 'NONE',  ( -61.56244935526919448, -277.8198993089526994, -198.7331171753913281 ) ) ;
#31585 = CARTESIAN_POINT ( 'NONE',  ( -80.54236993324256844, -289.4532246197836116, -334.1648610695394268 ) ) ;
#31586 = CARTESIAN_POINT ( 'NONE',  ( -99.04644691724929828, -289.0670534464729826, -309.8064303995699333 ) ) ;
#31587 = CARTESIAN_POINT ( 'NONE',  ( -4.182043124565208103, -290.4891287363078618, -203.0755806985293361 ) ) ;
#31588 = ORIENTED_EDGE ( 'NONE', *, *, #52296, .T. ) ;
#31589 = CARTESIAN_POINT ( 'NONE',  ( -111.8441652935849646, -278.1196860901031300, -270.4320060261264871 ) ) ;
#31590 = CARTESIAN_POINT ( 'NONE',  ( 30.54003665176527349, -287.4226542853485284, -297.5171275647541620 ) ) ;
#31591 = CARTESIAN_POINT ( 'NONE',  ( 209.1283748988095113, 29.46063112669806472, 13.48243931971135012 ) ) ;
#31592 = CARTESIAN_POINT ( 'NONE',  ( -114.1055335641777617, -285.4979963134953778, -269.9949370531536488 ) ) ;
#31593 = CARTESIAN_POINT ( 'NONE',  ( -27.86621114069169280, -291.2282787155681376, -194.1299505027877501 ) ) ;
#31594 = CARTESIAN_POINT ( 'NONE',  ( 19.42890481214846687, -283.5688955815255099, -321.7260395084860534 ) ) ;
#31595 = CARTESIAN_POINT ( 'NONE',  ( 3.388460919053434051, -282.3213103595576854, -331.0032326712681652 ) ) ;
#31596 = CARTESIAN_POINT ( 'NONE',  ( -114.3379633736027046, -296.5616392792451848, -269.6025362622565922 ) ) ;
#31597 = CARTESIAN_POINT ( 'NONE',  ( 24.40777402064800938, -277.4164340614624962, -310.3077885963562039 ) ) ;
#31598 = CARTESIAN_POINT ( 'NONE',  ( -65.93419239661774611, -289.6963316534138357, -201.3957521531118005 ) ) ;
#31599 = CARTESIAN_POINT ( 'NONE',  ( 33.24612186818926318, -274.0804437606964825, -250.0674406358796489 ) ) ;
#31600 = ORIENTED_EDGE ( 'NONE', *, *, #5711, .F. ) ;
#31601 = DIRECTION ( 'NONE',  ( -0.000000000000000000, -0.000000000000000000, -1.000000000000000000 ) ) ;
#31602 = CARTESIAN_POINT ( 'NONE',  ( 5.535221885216643045, -288.5575120494830799, -209.4467284744862070 ) ) ;
#31603 = CARTESIAN_POINT ( 'NONE',  ( -36.26494212304582732, -296.1186519479138610, -347.0574989538328055 ) ) ;
#31604 = CARTESIAN_POINT ( 'NONE',  ( -108.1899705745931044, -284.9661675174141351, -288.3726488235844272 ) ) ;
#31605 = CARTESIAN_POINT ( 'NONE',  ( 19.69432321872898584, -275.3106535725914341, -321.7589162018619504 ) ) ;
#31606 = CARTESIAN_POINT ( 'NONE',  ( 4.079631519686741647, -293.2456110996500911, -205.5092249541860099 ) ) ;
#31607 = CARTESIAN_POINT ( 'NONE',  ( 36.18396607520516994, -285.4592748441824597, -252.0777404733550213 ) ) ;
#31608 = CARTESIAN_POINT ( 'NONE',  ( 39.69045920771608138, -293.8847398970609106, -270.3057362904817182 ) ) ;
#31609 = CARTESIAN_POINT ( 'NONE',  ( -109.9943504101857314, -290.9820580472552365, -263.0344616019719979 ) ) ;
#31610 = CARTESIAN_POINT ( 'NONE',  ( 128.9467878515196162, -299.5541904835127980, -201.6105732245967488 ) ) ;
#31611 = CARTESIAN_POINT ( 'NONE',  ( 85.55100297371598117, -373.0521521680024648, -413.1172536214571096 ) ) ;
#31612 = CARTESIAN_POINT ( 'NONE',  ( -76.41338813104214012, -208.2854332698812243, -353.5099304025617357 ) ) ;
#31613 = CARTESIAN_POINT ( 'NONE',  ( -109.5621785376481512, -285.7590397302182623, -294.9966664917826051 ) ) ;
#31614 = CARTESIAN_POINT ( 'NONE',  ( 40.64545035920995986, -273.2666405000204009, -288.1938231032136741 ) ) ;
#31615 = ORIENTED_EDGE ( 'NONE', *, *, #12972, .T. ) ;
#31616 = CARTESIAN_POINT ( 'NONE',  ( -56.41250293446099562, -282.2240861343788083, -341.1462191906463772 ) ) ;
#31617 = CARTESIAN_POINT ( 'NONE',  ( -89.20100201988842059, -277.4252228645872265, -327.2501072400982025 ) ) ;
#31618 = CARTESIAN_POINT ( 'NONE',  ( 36.96326303731531482, -283.6719962765264427, -279.6614286388080473 ) ) ;
#31619 = CARTESIAN_POINT ( 'NONE',  ( -105.1058646074189653, -262.8840186013622429, -316.9941098723735990 ) ) ;
#31620 = CARTESIAN_POINT ( 'NONE',  ( -71.49181066764296588, -282.0691204901697802, -338.7159001505358447 ) ) ;
#31621 = CARTESIAN_POINT ( 'NONE',  ( 35.61298303957731548, -285.7767479664731241, -286.2153042961209053 ) ) ;
#31622 = CARTESIAN_POINT ( 'NONE',  ( -89.33275675203243793, -275.1903692999144937, -215.1783313827606605 ) ) ;
#31623 = CARTESIAN_POINT ( 'NONE',  ( -3.109377626976773890, -295.0793128955564839, -334.9067339296058208 ) ) ;
#31624 = CARTESIAN_POINT ( 'NONE',  ( -32.10554565368732227, -290.8043708015716220, -197.0420268373906083 ) ) ;
#31625 = CARTESIAN_POINT ( 'NONE',  ( -103.5138418283205937, -278.6913751229081413, -309.6389870895413878 ) ) ;
#31626 = CARTESIAN_POINT ( 'NONE',  ( 33.24219355772338247, -275.7980969960622701, -288.9867442042744301 ) ) ;
#31627 = CARTESIAN_POINT ( 'NONE',  ( 36.29296320578048096, -274.2004955341757295, -248.7411298974482463 ) ) ;
#31628 = DIRECTION ( 'NONE',  ( -0.000000000000000000, -0.000000000000000000, -1.000000000000000000 ) ) ;
#31629 = CARTESIAN_POINT ( 'NONE',  ( -33.69173762154775886, -275.0060845995964200, -345.2849583103067062 ) ) ;
#31630 = CARTESIAN_POINT ( 'NONE',  ( 32.88227782188145909, -295.3655190961599146, -300.6145655306884237 ) ) ;
#31631 = CARTESIAN_POINT ( 'NONE',  ( 201.0776230153480526, -147.7221692137691775, -8.778910157967986905 ) ) ;
#31632 = CIRCLE ( 'NONE', #43719, 25.00000000000001066 ) ;
#31633 = CARTESIAN_POINT ( 'NONE',  ( 208.8914279315829106, 0.04196010845019378793, -7.500000000000011546 ) ) ;
#31634 = CARTESIAN_POINT ( 'NONE',  ( -87.12872584445554480, -284.8447281865615537, -324.2402024237510432 ) ) ;
#31635 = CARTESIAN_POINT ( 'NONE',  ( -70.01382348071287254, -285.2366746354434213, -338.9793698795769501 ) ) ;
#31636 = CARTESIAN_POINT ( 'NONE',  ( -68.81131046605683821, -284.9757417579568255, -204.3658256840728598 ) ) ;
#31637 = CARTESIAN_POINT ( 'NONE',  ( -64.64789361071770202, -275.8144449706422279, -338.9778654478266731 ) ) ;
#31638 = CARTESIAN_POINT ( 'NONE',  ( 36.36915669432283238, -283.5322742621667658, -279.5886563088085381 ) ) ;
#31639 = CARTESIAN_POINT ( 'NONE',  ( -13.57998123185541850, -275.2180122261977431, -340.1721088107518085 ) ) ;
#31640 = CARTESIAN_POINT ( 'NONE',  ( -78.79551492306752891, -278.7047127963085700, -330.8861960760188481 ) ) ;
#31641 = CARTESIAN_POINT ( 'NONE',  ( 207.0609454132517726, 35.99714003645362226, 15.00000000000000000 ) ) ;
#31642 = CARTESIAN_POINT ( 'NONE',  ( -95.78964758816373148, -280.0293439850141795, -220.4610873726086027 ) ) ;
#31643 = CARTESIAN_POINT ( 'NONE',  ( -22.58413131596649848, -280.7284065665521098, -194.7970326231106526 ) ) ;
#31644 = ORIENTED_EDGE ( 'NONE', *, *, #3875, .F. ) ;
#31645 = ORIENTED_EDGE ( 'NONE', *, *, #9205, .F. ) ;
#31646 = CARTESIAN_POINT ( 'NONE',  ( 199.4949018615358511, 17.05867184936722936, -10.28330198088168501 ) ) ;
#31647 = CARTESIAN_POINT ( 'NONE',  ( 36.30936625334612700, -289.6391041640442268, -288.1874893336914170 ) ) ;
#31648 = CARTESIAN_POINT ( 'NONE',  ( -108.4583930955421636, -295.5225415981411743, -287.5900575030865411 ) ) ;
#31649 = CARTESIAN_POINT ( 'NONE',  ( -107.1643914186132918, -290.3148879563284481, -238.0146506444686736 ) ) ;
#31650 = CARTESIAN_POINT ( 'NONE',  ( 35.56953862388974130, -285.6226743145971341, -257.3465426152315558 ) ) ;
#31652 = CARTESIAN_POINT ( 'NONE',  ( -107.5251792754394558, -289.0998521598905313, -246.8610484537966272 ) ) ;
#31651 = CARTESIAN_POINT ( 'NONE',  ( -27.74185880043491537, -284.7511786946188863, -197.4007317255870078 ) ) ;
#31653 = CARTESIAN_POINT ( 'NONE',  ( -46.79111464945430043, -287.1347290993908814, -197.5238096685875462 ) ) ;
#31654 = CARTESIAN_POINT ( 'NONE',  ( -7.254749641371684099, -287.0639612120409652, -340.3838921088807865 ) ) ;
#31655 = CARTESIAN_POINT ( 'NONE',  ( 6.357400499688796280, -288.6453714808767472, -209.3431758782986662 ) ) ;
#31656 = CARTESIAN_POINT ( 'NONE',  ( -18.21598123060010721, -286.8060514119883919, -343.0538638398181774 ) ) ;
#31657 = CARTESIAN_POINT ( 'NONE',  ( -40.23168218731265000, -284.0306225597175285, -343.5393692074190994 ) ) ;
#31658 = CARTESIAN_POINT ( 'NONE',  ( -109.0255577970418415, -292.2592061426248051, -293.1462992156468772 ) ) ;
#31659 = CARTESIAN_POINT ( 'NONE',  ( 82.12709634636649980, -301.2636011320335570, -194.3234711915518460 ) ) ;
#31660 = CARTESIAN_POINT ( 'NONE',  ( 199.0143093133015100, 17.19615242270663202, -9.000000000000001776 ) ) ;
#31661 = CARTESIAN_POINT ( 'NONE',  ( -84.34020419986087802, -299.3312816093250035, -211.1964764290941901 ) ) ;
#31662 = CARTESIAN_POINT ( 'NONE',  ( -6.692461502728587419, -279.6622820339377995, -203.9153265435139986 ) ) ;
#31663 = CARTESIAN_POINT ( 'NONE',  ( 23.75719899250687916, -278.9606242146725208, -226.8648517451182443 ) ) ;
#31664 = CARTESIAN_POINT ( 'NONE',  ( -3.309518236176309358, -293.8114320374659201, -339.2666871655222849 ) ) ;
#31665 = CARTESIAN_POINT ( 'NONE',  ( -88.01092423530337783, -271.5719422238865945, -216.3409571816720245 ) ) ;
#31666 = CARTESIAN_POINT ( 'NONE',  ( 35.29306575426716819, -273.8435390795626176, -286.7133208401646129 ) ) ;
#31667 = CARTESIAN_POINT ( 'NONE',  ( -104.3796268654500210, -297.4628492996155842, -300.6045490638873616 ) ) ;
#31668 = CARTESIAN_POINT ( 'NONE',  ( 188.7149167944524493, -12.49482340714361506, 13.00000000000000178 ) ) ;
#31669 = CARTESIAN_POINT ( 'NONE',  ( 75.13442338291717704, -297.9159792440862020, -194.0828677818368817 ) ) ;
#31670 = CARTESIAN_POINT ( 'NONE',  ( -34.90982439382034386, -293.2618594751951946, -346.3088631521420098 ) ) ;
#31671 = CARTESIAN_POINT ( 'NONE',  ( -57.83630956907590104, -293.2076400547692288, -199.6300493939702960 ) ) ;
#31672 = ADVANCED_FACE ( 'NONE', ( #55534 ), #84383, .F. ) ;
#31673 = DIRECTION ( 'NONE',  ( 0.000000000000000000, 1.000000000000000000, 0.000000000000000000 ) ) ;
#31674 = CARTESIAN_POINT ( 'NONE',  ( 34.22767131610815738, -294.5555833536576529, -285.6010639303100334 ) ) ;
#31675 = CARTESIAN_POINT ( 'NONE',  ( 41.08708295871279859, -293.9068999365417199, -465.6442049081569508 ) ) ;
#31677 = CARTESIAN_POINT ( 'NONE',  ( 18.83309724950744624, -294.2133679068970196, -316.9807719879989918 ) ) ;
#31676 = CARTESIAN_POINT ( 'NONE',  ( -67.25218036032539715, -281.4625194063139588, -339.5259210065718207 ) ) ;
#31678 = CARTESIAN_POINT ( 'NONE',  ( -67.88135284565001371, -283.4420916149674099, -341.0458377732636563 ) ) ;
#31679 = CARTESIAN_POINT ( 'NONE',  ( 34.79356488540131664, -283.1843735584628234, -247.8707258188076992 ) ) ;
#31680 = CARTESIAN_POINT ( 'NONE',  ( -112.3381687415402155, -284.4360108815233730, -253.0038720263462722 ) ) ;
#31681 = CARTESIAN_POINT ( 'NONE',  ( -68.54293615403442175, -289.6410736254920266, -202.3285784733186574 ) ) ;
#31682 = ADVANCED_FACE ( 'NONE', ( #62166 ), #19532, .F. ) ;
#31683 = CARTESIAN_POINT ( 'NONE',  ( 15.26144635241925229, -280.8051034806416624, -325.6387511792363512 ) ) ;
#31684 = CARTESIAN_POINT ( 'NONE',  ( 17.26820761434590068, -285.5373138461500275, -221.1589798619104670 ) ) ;
#31685 = CARTESIAN_POINT ( 'NONE',  ( 32.57740277810245999, -286.8765904871625025, -301.8700303358252768 ) ) ;
#31686 = CARTESIAN_POINT ( 'NONE',  ( -53.30275703964352374, -296.8602561139885552, -342.4670182210999769 ) ) ;
#31687 = CARTESIAN_POINT ( 'NONE',  ( -112.1444856307785614, -280.1747292922206611, -254.7046915513597867 ) ) ;
#31689 = CARTESIAN_POINT ( 'NONE',  ( -59.73608192447613874, -279.4207704095745157, -200.8054307858841412 ) ) ;
#31688 = CARTESIAN_POINT ( 'NONE',  ( -5.226898591084080614, -292.6517535143096325, -338.5445237236838238 ) ) ;
#31690 = CARTESIAN_POINT ( 'NONE',  ( 22.20790884732915771, -293.0633223826307017, -221.5467340838717973 ) ) ;
#31691 = CARTESIAN_POINT ( 'NONE',  ( -112.9006632345497394, -282.6370507681265849, -269.9645206891372027 ) ) ;
#31692 = EDGE_CURVE ( 'NONE', #2170, #46575, #24817, .T. ) ;
#31693 = CARTESIAN_POINT ( 'NONE',  ( -95.48725449159030632, -279.8994201392774244, -317.7531029649275638 ) ) ;
#31695 = CARTESIAN_POINT ( 'NONE',  ( -37.00647208094338936, -294.1065667860947315, -343.6081098213658152 ) ) ;
#31694 = AXIS2_PLACEMENT_3D ( 'NONE', #45495, #67321, #60679 ) ;
#31696 = CARTESIAN_POINT ( 'NONE',  ( -56.84443915194403729, -295.8006349699807629, -197.8873670510351985 ) ) ;
#31697 = ORIENTED_EDGE ( 'NONE', *, *, #68134, .F. ) ;
#31698 = CARTESIAN_POINT ( 'NONE',  ( 139.6539576904058606, 132.0000000000000568, 10.50000000000000000 ) ) ;
#31699 = CARTESIAN_POINT ( 'NONE',  ( -13.81382168236735453, -282.3387376185723951, -199.4666214804129538 ) ) ;
#31700 = CARTESIAN_POINT ( 'NONE',  ( 32.80750523410983988, -293.3302592988459310, -290.8285448946089673 ) ) ;
#31701 = VECTOR ( 'NONE', #15840, 1000.000000000000000 ) ;
#31702 = CARTESIAN_POINT ( 'NONE',  ( 31.98288692825983404, -272.6237833571632905, -237.0123917617631264 ) ) ;
#31703 = CARTESIAN_POINT ( 'NONE',  ( -48.92262123649869210, -296.9669618639499049, -194.4215012050215705 ) ) ;
#31704 = CARTESIAN_POINT ( 'NONE',  ( 18.29774641103156796, -289.5890328478654396, -322.8734999650166628 ) ) ;
#31705 = CARTESIAN_POINT ( 'NONE',  ( -31.87347319535359347, -288.8146914552878570, -343.2066483003274016 ) ) ;
#31706 = B_SPLINE_CURVE_WITH_KNOTS ( 'NONE', 3,
 ( #18457, #45933, #90861, #17544 ),
 .UNSPECIFIED., .F., .F.,
 ( 4, 4 ),
 ( 0.000000000000000000, 0.001074155171061463854 ),
 .UNSPECIFIED. ) ;
#31707 = CARTESIAN_POINT ( 'NONE',  ( -101.4241730879958254, -280.5659399149620299, -233.9723228616421977 ) ) ;
#31708 = CARTESIAN_POINT ( 'NONE',  ( -67.24908155059992509, -299.4146921300625195, -202.6455285206034773 ) ) ;
#31709 = CARTESIAN_POINT ( 'NONE',  ( -9.080349657951865439, -279.2250951291436536, -202.6231923054262438 ) ) ;
#31710 = VERTEX_POINT ( 'NONE', #33742 ) ;
#31711 = CARTESIAN_POINT ( 'NONE',  ( -75.76566857880099803, -297.2209533044920704, -203.5965486413334986 ) ) ;
#31712 = CARTESIAN_POINT ( 'NONE',  ( -64.62165223510481837, -293.6133828685094613, -201.0860827745362371 ) ) ;
#31713 = CARTESIAN_POINT ( 'NONE',  ( 199.0061125298537377, 249.5000000000000568, -7.725424859374024678 ) ) ;
#31714 = CARTESIAN_POINT ( 'NONE',  ( -93.52349448395433740, -291.8663853719565395, -223.5708705120093782 ) ) ;
#31715 = CARTESIAN_POINT ( 'NONE',  ( 208.4306832106271088, 42.44233620800392970, -7.500000000000012434 ) ) ;
#31716 = ORIENTED_EDGE ( 'NONE', *, *, #10707, .F. ) ;
#31717 = CARTESIAN_POINT ( 'NONE',  ( -40.55591917488535358, -290.1517546168335002, -194.6515535156463841 ) ) ;
#31718 = CARTESIAN_POINT ( 'NONE',  ( -107.2535800384607683, -272.3426188741493092, -248.9671800270169228 ) ) ;
#31719 = CYLINDRICAL_SURFACE ( 'NONE', #76808, 2.000000000000000000 ) ;
#31720 = CARTESIAN_POINT ( 'NONE',  ( 175.2296996224750103, 250.5000000000000568, 0.000000000000000000 ) ) ;
#31721 = CARTESIAN_POINT ( 'NONE',  ( -105.3946199326761359, -292.5220187246089836, -235.7263304947500444 ) ) ;
#31722 = CARTESIAN_POINT ( 'NONE',  ( -88.47809603358389552, -286.1948066931273615, -334.5364918783848793 ) ) ;
#31723 = CARTESIAN_POINT ( 'NONE',  ( -7.547864174331647469, -288.4438165807034125, -201.7145174248215653 ) ) ;
#31724 = CARTESIAN_POINT ( 'NONE',  ( 34.65490009692324946, -273.8157396209811623, -290.8167259753296889 ) ) ;
#31725 = CARTESIAN_POINT ( 'NONE',  ( 33.42323654118416698, -277.1697606067490369, -247.0948632554170104 ) ) ;
#31726 = CARTESIAN_POINT ( 'NONE',  ( -2.949643699780619688, -290.5902078109149329, -204.3421763437440575 ) ) ;
#31727 = CARTESIAN_POINT ( 'NONE',  ( -31.19793442991275612, -281.9892563525241940, -194.7939784165786250 ) ) ;
#31728 = EDGE_LOOP ( 'NONE', ( #19512, #37845, #93570, #56816 ) ) ;
#31729 = CARTESIAN_POINT ( 'NONE',  ( -18.71766321217296181, -282.1546293932814820, -341.1033233331066867 ) ) ;
#31730 = CARTESIAN_POINT ( 'NONE',  ( -104.6975156503065847, -279.1553599703948976, -307.0310869529659499 ) ) ;
#31731 = CARTESIAN_POINT ( 'NONE',  ( -2.556667356714538819, -279.2967692811753295, -202.0968480614500891 ) ) ;
#31732 = CARTESIAN_POINT ( 'NONE',  ( 63.58840756535673222, 47.24236442185751628, -315.7359544152388366 ) ) ;
#31733 = CARTESIAN_POINT ( 'NONE',  ( 37.67829887599565808, -276.6983139779528642, -286.6958664055291024 ) ) ;
#31734 = APPLICATION_PROTOCOL_DEFINITION ( 'draft international standard', 'automotive_design', 1998, #2714 ) ;
#31735 = CARTESIAN_POINT ( 'NONE',  ( -73.63234562624435853, -275.0999704676132183, -203.1778854431856303 ) ) ;
#31736 = CARTESIAN_POINT ( 'NONE',  ( -107.3452863284742449, -275.1604526064901393, -262.5058405983616012 ) ) ;
#31737 = VERTEX_POINT ( 'NONE', #49353 ) ;
#31738 = CARTESIAN_POINT ( 'NONE',  ( -73.68631503275130967, -290.6263995946848695, -334.0410824891840207 ) ) ;
#31739 = CARTESIAN_POINT ( 'NONE',  ( -104.2529272901706179, -291.8404560376891368, -306.3730839265644477 ) ) ;
#31740 = CARTESIAN_POINT ( 'NONE',  ( -4.780232890902527565, -291.8412761275359344, -204.8976238329101420 ) ) ;
#31741 = CARTESIAN_POINT ( 'NONE',  ( -18.19127754818147125, -285.8000810026210274, -195.7890253703707799 ) ) ;
#31742 = CARTESIAN_POINT ( 'NONE',  ( 73.43068321062709458, -134.2641364535880939, 0.000000000000000000 ) ) ;
#31743 = CARTESIAN_POINT ( 'NONE',  ( -37.56316512000142893, -281.4548757140970565, -344.1733544659482504 ) ) ;
#31744 = CARTESIAN_POINT ( 'NONE',  ( 22.17779627711555079, -290.0249118884566428, -314.7478766808773116 ) ) ;
#31745 = CARTESIAN_POINT ( 'NONE',  ( -6.985395507497001333, -281.1263059000270346, -337.5255556735269238 ) ) ;
#31746 = CARTESIAN_POINT ( 'NONE',  ( 18.32719162700897542, -282.1883334674241723, -222.3603717562722011 ) ) ;
#31747 = APPLICATION_CONTEXT ( 'automotive_design' ) ;
#31748 = CARTESIAN_POINT ( 'NONE',  ( 38.55113162583872821, -288.3475780284512098, -258.7368638129711371 ) ) ;
#31749 = CARTESIAN_POINT ( 'NONE',  ( -110.2292480326194521, -278.9689932649845332, -276.0899462611741342 ) ) ;
#31750 = CARTESIAN_POINT ( 'NONE',  ( -30.71623702496241748, -290.9289376234380029, -193.9927621085660689 ) ) ;
#31751 = CARTESIAN_POINT ( 'NONE',  ( 33.70620831435992670, -287.9807511608051982, -240.9586434013265830 ) ) ;
#31752 = CARTESIAN_POINT ( 'NONE',  ( -3.522066819966669815, -286.9789546031654481, -201.2397336393281080 ) ) ;
#31753 = CARTESIAN_POINT ( 'NONE',  ( -103.0117370278437221, -284.2858308864481387, -302.3589568781726484 ) ) ;
#31754 = EDGE_LOOP ( 'NONE', ( #88527, #67687, #90731, #60590 ) ) ;
#31755 = FACE_OUTER_BOUND ( 'NONE', #70860, .T. ) ;
#31756 = CARTESIAN_POINT ( 'NONE',  ( -8.995689436432197539, -294.2793800456232702, -200.0986873452157226 ) ) ;
#31757 = CARTESIAN_POINT ( 'NONE',  ( 36.61024445866254950, -291.9893659132109747, -250.7042011461205107 ) ) ;
#31758 = CARTESIAN_POINT ( 'NONE',  ( 17.60384876144849287, -275.3002858623294173, -318.7989869804835621 ) ) ;
#31759 = CARTESIAN_POINT ( 'NONE',  ( -113.4996495248957586, -296.0352185049387685, -259.6226531438382494 ) ) ;
#31760 = CIRCLE ( 'NONE', #24176, 4.999999999999990230 ) ;
#31761 = CARTESIAN_POINT ( 'NONE',  ( 7.109717562458071072, -291.1501353631761049, -211.5837480527513890 ) ) ;
#31762 = CARTESIAN_POINT ( 'NONE',  ( -63.41575280811702697, -295.9476800648075709, -201.0384564183853229 ) ) ;
#31763 = CARTESIAN_POINT ( 'NONE',  ( -66.73711755853138072, -292.8632882122278147, -203.1075683379044676 ) ) ;
#31764 = CARTESIAN_POINT ( 'NONE',  ( -5.921562004080793251, -293.5548528198679037, -204.1128396214604663 ) ) ;
#31765 = CARTESIAN_POINT ( 'NONE',  ( 208.9100279911569658, 35.82717761498059872, 14.27724168160876950 ) ) ;
#31766 = CARTESIAN_POINT ( 'NONE',  ( -1.600891109880263841, -292.5794578030966591, -336.5014585808833090 ) ) ;
#31767 = CARTESIAN_POINT ( 'NONE',  ( -112.2245992611167793, -298.4877883262126375, -275.3867228762755417 ) ) ;
#31768 = CARTESIAN_POINT ( 'NONE',  ( -13.19903733447574901, -289.6719311585343348, -339.5025692339283410 ) ) ;
#31769 = CARTESIAN_POINT ( 'NONE',  ( -17.76047963875726765, -278.7807243189188853, -343.1277490994326627 ) ) ;
#31770 = CARTESIAN_POINT ( 'NONE',  ( -105.9963593142793599, -276.9067761242620236, -304.4591271649478017 ) ) ;
#31771 = CARTESIAN_POINT ( 'NONE',  ( -95.94461552330328402, -272.5730258650728501, -220.5511780372910096 ) ) ;
#31772 = CARTESIAN_POINT ( 'NONE',  ( 20.45490370165923721, -280.2831900985194693, -317.2945993183348037 ) ) ;
#31773 = CARTESIAN_POINT ( 'NONE',  ( -51.18746048210949340, -275.6261829625855739, -345.2926556269869138 ) ) ;
#31774 = EDGE_CURVE ( 'NONE', #6020, #36590, #11962, .T. ) ;
#31775 = CARTESIAN_POINT ( 'NONE',  ( -107.3441061250242825, -294.9402167524035008, -292.9069301903481914 ) ) ;
#31776 = CARTESIAN_POINT ( 'NONE',  ( -94.69784351963394897, -273.8422338702360435, -225.0382155619596176 ) ) ;
#31778 = CARTESIAN_POINT ( 'NONE',  ( -63.30473799775171528, -273.5375915509443985, -202.1206455988851189 ) ) ;
#31777 = CARTESIAN_POINT ( 'NONE',  ( -112.0323145975978321, -288.7047437098329965, -259.9941125139034739 ) ) ;
#31779 = CARTESIAN_POINT ( 'NONE',  ( -31.82677828541186216, -288.9845056599974100, -347.2159241085329882 ) ) ;
#31780 = CARTESIAN_POINT ( 'NONE',  ( -56.98577446623215792, -299.7800471105067572, -197.5573270854397094 ) ) ;
#31781 = CARTESIAN_POINT ( 'NONE',  ( -110.5679336986514585, -294.7512726635061995, -254.8740717498590982 ) ) ;
#31782 = CARTESIAN_POINT ( 'NONE',  ( -10.76749526745584618, -281.9115609947952521, -342.5145941235296050 ) ) ;
#31783 = DIRECTION ( 'NONE',  ( 0.000000000000000000, 0.000000000000000000, 1.000000000000000000 ) ) ;
#31784 = CARTESIAN_POINT ( 'NONE',  ( 28.37792330265520846, -279.0702568186964072, -234.1169682662477385 ) ) ;
#31785 = LINE ( 'NONE', #9997, #61913 ) ;
#31786 = CARTESIAN_POINT ( 'NONE',  ( -110.3664153697937564, -289.4439490184408896, -262.9772525857731580 ) ) ;
#31787 = CARTESIAN_POINT ( 'NONE',  ( -110.1962111355657754, -282.5068708570287868, -284.6119322945127124 ) ) ;
#31788 = CARTESIAN_POINT ( 'NONE',  ( 200.2324206114115555, 214.8829713991971744, -2.809954999877010806 ) ) ;
#31789 =( NAMED_UNIT ( * ) SI_UNIT ( $, .STERADIAN. ) SOLID_ANGLE_UNIT ( ) );
#31790 = CARTESIAN_POINT ( 'NONE',  ( -85.08307072620955580, -289.3929332587509293, -212.5185542506116860 ) ) ;
#31791 = CARTESIAN_POINT ( 'NONE',  ( -89.74871073326912096, -274.8161165442882066, -218.5517270248318482 ) ) ;
#31792 = CARTESIAN_POINT ( 'NONE',  ( -70.28537121042901958, -284.6816990562390401, -339.5327396634178285 ) ) ;
#31794 = CARTESIAN_POINT ( 'NONE',  ( -107.7611527384710541, -284.2974269724152236, -289.6463136459557859 ) ) ;
#31793 = CARTESIAN_POINT ( 'NONE',  ( -3.186173223533343535, -272.5795070579386561, -202.9470280987365527 ) ) ;
#31795 = CARTESIAN_POINT ( 'NONE',  ( 35.29170777241810697, -277.1361690703892009, -282.4916152360212891 ) ) ;
#31796 = CARTESIAN_POINT ( 'NONE',  ( -56.63292713618687912, -278.1099745024274057, -340.9860351287802587 ) ) ;
#31797 = EDGE_CURVE ( 'NONE', #46866, #44867, #47464, .T. ) ;
#31798 = CARTESIAN_POINT ( 'NONE',  ( 14.39285596943708789, -284.3248188417588835, -324.6615447973005075 ) ) ;
#31799 = ORIENTED_EDGE ( 'NONE', *, *, #27878, .T. ) ;
#31800 = DIRECTION ( 'NONE',  ( 0.000000000000000000, 0.000000000000000000, 1.000000000000000000 ) ) ;
#31801 = CARTESIAN_POINT ( 'NONE',  ( 26.51055703655141471, -293.9524580666045495, -313.3947009090193205 ) ) ;
#31802 = CARTESIAN_POINT ( 'NONE',  ( 5.652619050774053910, -288.6172405577019617, -209.2787414049485619 ) ) ;
#31803 = EDGE_CURVE ( 'NONE', #19733, #1988, #65674, .T. ) ;
#31804 = DIRECTION ( 'NONE',  ( 0.000000000000000000, 0.000000000000000000, -1.000000000000000000 ) ) ;
#31805 = CARTESIAN_POINT ( 'NONE',  ( 36.57525178469694538, -291.4809262143062369, -305.9938812882205070 ) ) ;
#31806 = CARTESIAN_POINT ( 'NONE',  ( -95.09618839529409229, -277.0620616649609360, -321.0422575294525132 ) ) ;
#31807 = CARTESIAN_POINT ( 'NONE',  ( -30.74599173846373645, -290.5339486922550805, -194.3948969467839447 ) ) ;
#31808 = CARTESIAN_POINT ( 'NONE',  ( -93.79862918966466623, -286.7385158621798382, -222.9973880291659896 ) ) ;
#31809 = CARTESIAN_POINT ( 'NONE',  ( -62.10807861360017768, -279.1386519388497618, -340.1622862601814745 ) ) ;
#31810 = CARTESIAN_POINT ( 'NONE',  ( -69.56104999889298313, -287.0616343506380872, -201.0610778605604878 ) ) ;
#31811 = CARTESIAN_POINT ( 'NONE',  ( 22.62392511233066372, -284.1681633043053239, -315.4281530696096638 ) ) ;
#31812 = CARTESIAN_POINT ( 'NONE',  ( -22.93681887511569073, -277.0395634160643112, -346.0558967817065650 ) ) ;
#31813 = CARTESIAN_POINT ( 'NONE',  ( -80.22794689398779155, -277.4484990829081426, -334.3766129019576283 ) ) ;
#31814 = CARTESIAN_POINT ( 'NONE',  ( -101.1433752010043747, -298.9909116034737053, -231.9116312453902822 ) ) ;
#31815 = CARTESIAN_POINT ( 'NONE',  ( 156.4851178187871312, 14.99999999999999467, 7.000000000000000888 ) ) ;
#31816 = CARTESIAN_POINT ( 'NONE',  ( -95.99890600148557951, -275.6948066931273615, -223.6242672951989618 ) ) ;
#31817 = AXIS2_PLACEMENT_3D ( 'NONE', #57230, #70016, #34035 ) ;
#31818 = CARTESIAN_POINT ( 'NONE',  ( -70.17202744168670847, -295.7637598136120687, -202.0787989412391994 ) ) ;
#31819 = CARTESIAN_POINT ( 'NONE',  ( 17.06571399127465583, -89.54582641780471874, 22.50000000000000000 ) ) ;
#31820 = CARTESIAN_POINT ( 'NONE',  ( -24.32479269652457177, -276.3892560612371767, -342.3052298048591524 ) ) ;
#31821 = CARTESIAN_POINT ( 'NONE',  ( -76.24436942978653065, -274.7497161139079935, -204.3104947960326854 ) ) ;
#31822 = VECTOR ( 'NONE', #81628, 1000.000000000000000 ) ;
#31823 = CARTESIAN_POINT ( 'NONE',  ( 30.51943510554037431, -280.1448344558133954, -234.3634104413949615 ) ) ;
#31824 = CARTESIAN_POINT ( 'NONE',  ( 36.69337778888591828, -289.2849849583721493, -268.2616577575786323 ) ) ;
#31825 = CARTESIAN_POINT ( 'NONE',  ( -110.5447287818828102, -297.7990780355128209, -291.9483894297014785 ) ) ;
#31826 = CARTESIAN_POINT ( 'NONE',  ( -110.4163765976229428, -297.4664551539190143, -293.3854289970482796 ) ) ;
#31827 = CARTESIAN_POINT ( 'NONE',  ( 19.86196082207895586, -294.8835905162221707, -222.1141532739970046 ) ) ;
#31828 = CARTESIAN_POINT ( 'NONE',  ( 34.50163982809560537, -279.2817490408192498, -249.4192238045684746 ) ) ;
#31829 = CARTESIAN_POINT ( 'NONE',  ( 37.14402007957295382, -283.4845641785113344, -271.3081467475175828 ) ) ;
#31830 = CARTESIAN_POINT ( 'NONE',  ( -73.52587143549826010, -295.6478766138080232, -205.3071408107068407 ) ) ;
#31831 = CARTESIAN_POINT ( 'NONE',  ( -106.2732027943526560, -285.7318680082088918, -302.8401628202364009 ) ) ;
#31832 = CARTESIAN_POINT ( 'NONE',  ( 9.237442516738328280, -285.6300666963919070, -213.7518471595305414 ) ) ;
#31833 = CARTESIAN_POINT ( 'NONE',  ( 37.88668148172862260, -280.7003687205219649, -254.3606081014471272 ) ) ;
#31834 = CARTESIAN_POINT ( 'NONE',  ( 66.45820036739932846, 46.88234517766255749, -318.5738176559102044 ) ) ;
#31835 = EDGE_LOOP ( 'NONE', ( #65337, #16237, #35843, #37883 ) ) ;
#31836 = CARTESIAN_POINT ( 'NONE',  ( 22.81227569721311355, -286.7617784443814912, -317.5001754276903512 ) ) ;
#31837 = CARTESIAN_POINT ( 'NONE',  ( 13.15724001548059441, -286.4481424706384018, -217.5472115923622312 ) ) ;
#31838 = ORIENTED_EDGE ( 'NONE', *, *, #11779, .T. ) ;
#31839 = CARTESIAN_POINT ( 'NONE',  ( -113.8988191518282491, -285.5646572735515747, -275.7099750386934147 ) ) ;
#31840 = CARTESIAN_POINT ( 'NONE',  ( 23.06743953656408053, -275.3148381989095128, -229.3164619267827788 ) ) ;
#31841 = CARTESIAN_POINT ( 'NONE',  ( -33.54087841627652011, -291.0192777922545702, -193.7644714204199374 ) ) ;
#31842 = CARTESIAN_POINT ( 'NONE',  ( 30.99036858264368277, -282.6588078435840430, -305.6320858171718555 ) ) ;
#31843 = DIRECTION ( 'NONE',  ( 0.000000000000000000, 0.000000000000000000, 1.000000000000000000 ) ) ;
#31844 = CARTESIAN_POINT ( 'NONE',  ( -112.3185891297875543, -280.2521489285202279, -256.1075677718598627 ) ) ;
#31845 = CARTESIAN_POINT ( 'NONE',  ( 25.91537443563242959, -282.4653371581390502, -314.2509961836761363 ) ) ;
#31846 = CARTESIAN_POINT ( 'NONE',  ( -92.05005921254146983, -282.6952119285918457, -226.6919474004047572 ) ) ;
#31847 = CARTESIAN_POINT ( 'NONE',  ( 180.8476761818623402, 253.8486742402554910, -166.7977385971483955 ) ) ;
#31848 = EDGE_LOOP ( 'NONE', ( #2915, #46604, #83770, #35704 ) ) ;
#31849 = CARTESIAN_POINT ( 'NONE',  ( -4.232582328867905197, -278.6149089201633728, -337.4858259348673073 ) ) ;
#31850 = CARTESIAN_POINT ( 'NONE',  ( -114.2697642191412655, -272.9088482181212498, -284.0992320288099791 ) ) ;
#31851 = CARTESIAN_POINT ( 'NONE',  ( 31.84994229670647670, -279.9390543397678925, -298.3676068523774916 ) ) ;
#31852 = CARTESIAN_POINT ( 'NONE',  ( -104.8531774944120798, -296.2762003072896846, -242.3237662583216547 ) ) ;
#31853 = CARTESIAN_POINT ( 'NONE',  ( 35.42616303855504611, -293.3768198400439928, -295.5116376855012845 ) ) ;
#31854 = DIRECTION ( 'NONE',  ( -1.000000000000000000, -0.000000000000000000, -0.000000000000000000 ) ) ;
#31856 = CARTESIAN_POINT ( 'NONE',  ( -69.12072839533406921, -287.8771842285432285, -336.9684282428895585 ) ) ;
#31855 = CARTESIAN_POINT ( 'NONE',  ( -75.47001902956293407, -296.1291383984989238, -204.0822949002132418 ) ) ;
#31857 = CARTESIAN_POINT ( 'NONE',  ( 25.48506558515284937, -295.9508207140413560, -310.0009049432887878 ) ) ;
#31858 = CARTESIAN_POINT ( 'NONE',  ( -1.963600746039354306, -287.8458789502048489, -205.8863748293175604 ) ) ;
#31859 = ORIENTED_EDGE ( 'NONE', *, *, #51756, .F. ) ;
#31860 = CARTESIAN_POINT ( 'NONE',  ( -5.994023019284250964, -293.3954294072080984, -200.2744594085232563 ) ) ;
#31861 = CARTESIAN_POINT ( 'NONE',  ( -99.66508547038839083, -285.5705881369278814, -232.1361929606052570 ) ) ;
#31862 = CARTESIAN_POINT ( 'NONE',  ( -97.91052340887563332, -295.9766752593686761, -223.4419120162062882 ) ) ;
#31863 = CARTESIAN_POINT ( 'NONE',  ( -86.41777221615089388, -292.1937952520814292, -211.1675960672763779 ) ) ;
#31864 = CARTESIAN_POINT ( 'NONE',  ( -74.65454616443274460, -292.0615893721245016, -203.0760644864496101 ) ) ;
#31865 = CARTESIAN_POINT ( 'NONE',  ( 5.846333416531644289, -288.6151341068022020, -329.2781200263282244 ) ) ;
#31866 = ORIENTED_EDGE ( 'NONE', *, *, #89197, .T. ) ;
#31867 = CARTESIAN_POINT ( 'NONE',  ( 208.6208076322478746, 32.98517505407394168, 14.49999999999999822 ) ) ;
#31868 = CARTESIAN_POINT ( 'NONE',  ( 74.09727644056822271, -301.2935895614463675, -194.5614116136725045 ) ) ;
#31869 = CARTESIAN_POINT ( 'NONE',  ( -68.66757489526206371, -272.4444544232246699, -200.4418753842954857 ) ) ;
#31870 = ADVANCED_FACE ( 'NONE', ( #77301 ), #56615, .T. ) ;
#31871 = CARTESIAN_POINT ( 'NONE',  ( 25.75568344301485268, -281.1211054849086963, -307.6382906422340398 ) ) ;
#31872 = ORIENTED_EDGE ( 'NONE', *, *, #43435, .T. ) ;
#31873 = CARTESIAN_POINT ( 'NONE',  ( -9.240139294532259129, -276.2020906246852974, -341.9839438271516201 ) ) ;
#31874 = CARTESIAN_POINT ( 'NONE',  ( -92.60383411666781228, -271.6433330869302836, -221.4475517326621912 ) ) ;
#31875 = CARTESIAN_POINT ( 'NONE',  ( -70.30982684041379116, -281.4733711013172410, -203.8341187175132063 ) ) ;
#31876 = CARTESIAN_POINT ( 'NONE',  ( 23.46419122538822322, -274.2768113399873755, -313.0346475994430762 ) ) ;
#31877 = CARTESIAN_POINT ( 'NONE',  ( -108.5639646114405963, -297.9906066198687995, -252.5749204066959237 ) ) ;
#31878 = CARTESIAN_POINT ( 'NONE',  ( 9.161364539541075658, -299.7274143246822291, -197.0432256491417320 ) ) ;
#31879 = CARTESIAN_POINT ( 'NONE',  ( -109.1043702041562682, -298.4791070789244714, -244.7376990471343561 ) ) ;
#31880 = CARTESIAN_POINT ( 'NONE',  ( -65.58680202967329365, -271.7047737576141344, -200.4858111787266637 ) ) ;
#31881 = CARTESIAN_POINT ( 'NONE',  ( 32.72439651894691082, -293.9259643279607417, -249.3388585973115141 ) ) ;
#31882 = CARTESIAN_POINT ( 'NONE',  ( -57.80149485178242941, -290.3575542961208953, -199.6199712493877314 ) ) ;
#31883 = DIRECTION ( 'NONE',  ( -1.000000000000000000, 0.000000000000000000, 0.000000000000000000 ) ) ;
#31884 = CARTESIAN_POINT ( 'NONE',  ( -10.37506249526197699, -274.8869956241390469, -198.2466361817992322 ) ) ;
#31885 = CARTESIAN_POINT ( 'NONE',  ( -65.81510352289728871, -273.8356662857958668, -203.1430749908509199 ) ) ;
#31886 = CARTESIAN_POINT ( 'NONE',  ( 23.85053063380354743, -280.8521416932389343, -316.2828902533398718 ) ) ;
#31887 = CARTESIAN_POINT ( 'NONE',  ( -34.88834522886462963, -297.0215532193161039, -345.4877409546422768 ) ) ;
#31888 = CARTESIAN_POINT ( 'NONE',  ( 214.2238915819278589, 32.98517505407394168, 10.00000000000000000 ) ) ;
#31889 = CARTESIAN_POINT ( 'NONE',  ( -109.6595637643180794, -283.5992156922690128, -281.7647174284704192 ) ) ;
#31890 = CARTESIAN_POINT ( 'NONE',  ( -60.68705807224014137, -281.3540195782809974, -341.8649252344125102 ) ) ;
#31891 = CARTESIAN_POINT ( 'NONE',  ( 32.62767779990911521, -273.8248737225063110, -247.4009919039763190 ) ) ;
#31892 = CARTESIAN_POINT ( 'NONE',  ( -43.04105364428300362, -281.9804960131575626, -195.5267823691980027 ) ) ;
#31893 = DIRECTION ( 'NONE',  ( -1.000000000000000000, 0.000000000000000000, 0.000000000000000000 ) ) ;
#31894 = CARTESIAN_POINT ( 'NONE',  ( -112.3417001281054297, -274.5519904173220311, -270.3865538441530134 ) ) ;
#31895 = CARTESIAN_POINT ( 'NONE',  ( -41.13236985096396126, -272.4052040967222865, -194.2037420736955369 ) ) ;
#31896 = CIRCLE ( 'NONE', #4718, 3.000000000000002665 ) ;
#31897 = CARTESIAN_POINT ( 'NONE',  ( -59.10917007174773374, -279.3333775728684145, -342.3069703749188761 ) ) ;
#31898 = DIRECTION ( 'NONE',  ( -1.000000000000000000, 0.000000000000000000, -0.000000000000000000 ) ) ;
#31899 = CARTESIAN_POINT ( 'NONE',  ( -96.89410921334201987, -285.8390263795151327, -316.8672979406983927 ) ) ;
#31900 = CARTESIAN_POINT ( 'NONE',  ( 199.1087447750284980, 64.61450673763175701, 10.46317447812566392 ) ) ;
#31901 = CARTESIAN_POINT ( 'NONE',  ( -109.7634582419306497, -288.8031995013129176, -250.8165591967779164 ) ) ;
#31902 = DIRECTION ( 'NONE',  ( -0.2156506209390900430, 0.000000000000000000, 0.9764705882352960886 ) ) ;
#31903 = CARTESIAN_POINT ( 'NONE',  ( -101.8234346083377204, -294.8711233832095218, -305.4215860656804011 ) ) ;
#31904 = CARTESIAN_POINT ( 'NONE',  ( 21.31917642920348754, -286.3220671818577898, -315.8763828933383593 ) ) ;
#31905 = CARTESIAN_POINT ( 'NONE',  ( 79.80194596570532894, 84.98805272827966917, -300.3302785054510196 ) ) ;
#31906 = CARTESIAN_POINT ( 'NONE',  ( -95.50941791035214123, -293.8995456198923648, -317.7259745329529323 ) ) ;
#31907 = CARTESIAN_POINT ( 'NONE',  ( 20.94677185556329846, -286.7015515683531248, -319.6070496759664934 ) ) ;
#31908 = CARTESIAN_POINT ( 'NONE',  ( 35.01907236396948520, -283.3423687231612575, -284.9285592539940808 ) ) ;
#31909 = CARTESIAN_POINT ( 'NONE',  ( -27.52551098264708784, -281.1690817460281551, -345.7637356916616227 ) ) ;
#31910 = CARTESIAN_POINT ( 'NONE',  ( -69.97245264539293430, -289.4943724409212109, -335.6760795783523008 ) ) ;
#31911 = CARTESIAN_POINT ( 'NONE',  ( 34.22742982456013294, -283.2022142483533571, -287.5388747412744124 ) ) ;
#31912 = CARTESIAN_POINT ( 'NONE',  ( -24.02609789398796636, -283.6805377689173042, -342.3006513673317386 ) ) ;
#31913 = CARTESIAN_POINT ( 'NONE',  ( 20.24864189410923032, -290.2009997342684642, -318.9590532439549975 ) ) ;
#31914 = CARTESIAN_POINT ( 'NONE',  ( -43.29187421240101230, -298.1457895272055794, -193.5381517441040842 ) ) ;
#31915 = CARTESIAN_POINT ( 'NONE',  ( -35.52378678070758156, -274.0743408453358825, -193.3694505866060922 ) ) ;
#31916 = CARTESIAN_POINT ( 'NONE',  ( -49.99173294697245495, -293.8699949332213350, -196.7435368656326489 ) ) ;
#31917 = DIRECTION ( 'NONE',  ( -1.000000000000000000, 1.124465274301078034E-16, 0.000000000000000000 ) ) ;
#31918 = CARTESIAN_POINT ( 'NONE',  ( -85.33152481854864391, -281.9090924074130839, -210.2361428286349110 ) ) ;
#31919 = CARTESIAN_POINT ( 'NONE',  ( -31.61595600124092442, -274.9799995323535882, -345.3607659508787719 ) ) ;
#31920 = DIRECTION ( 'NONE',  ( -1.000000000000000000, -9.031908658476993102E-16, 0.000000000000000000 ) ) ;
#31921 = CARTESIAN_POINT ( 'NONE',  ( -110.8448982739032687, -295.2085583523438004, -250.0735484861346549 ) ) ;
#31922 = CARTESIAN_POINT ( 'NONE',  ( -108.4916734135219656, -291.8939093006709982, -290.1482683914920813 ) ) ;
#31923 = CARTESIAN_POINT ( 'NONE',  ( -51.57319391114928209, -273.2140119269045044, -198.6059989695407921 ) ) ;
#31924 = CARTESIAN_POINT ( 'NONE',  ( -110.6646592534776232, -292.1687075913327476, -262.9819976625192339 ) ) ;
#31925 = CARTESIAN_POINT ( 'NONE',  ( -25.38243844869774435, -293.1494479978140362, -198.0572463151052602 ) ) ;
#31927 = EDGE_CURVE ( 'NONE', #17402, #90054, #33063, .T. ) ;
#31926 = CARTESIAN_POINT ( 'NONE',  ( -78.92774084220380360, -285.3815113308673403, -331.5867272440648321 ) ) ;
#31928 = CARTESIAN_POINT ( 'NONE',  ( -47.68176297217866022, -293.3485544582074454, -194.5998119806215527 ) ) ;
#31929 = CARTESIAN_POINT ( 'NONE',  ( -90.45570503368409732, -292.6344998693948583, -215.2221533620264324 ) ) ;
#31930 = CARTESIAN_POINT ( 'NONE',  ( -3.145635356501999880, -294.4203921897134819, -334.8563050794364244 ) ) ;
#31931 = CARTESIAN_POINT ( 'NONE',  ( 32.83726428960925148, -289.2069678626473888, -243.7587688623997906 ) ) ;
#31932 = CARTESIAN_POINT ( 'NONE',  ( 38.66818699411951599, -281.8737954578546692, -282.7519086214052777 ) ) ;
#31933 = CARTESIAN_POINT ( 'NONE',  ( -4.174018851904285121, -296.5441181210520654, -194.8118598026143218 ) ) ;
#31934 = CARTESIAN_POINT ( 'NONE',  ( -109.3037131088121612, -284.0370359753096636, -297.9043881315205340 ) ) ;
#31935 = CARTESIAN_POINT ( 'NONE',  ( -9.348653367303350947, -278.6643636632716152, -339.5720734106865280 ) ) ;
#31936 = EDGE_CURVE ( 'NONE', #69774, #78913, #15765, .T. ) ;
#31937 = CARTESIAN_POINT ( 'NONE',  ( -45.69984345545591253, -281.9552266982748847, -343.3320169154444557 ) ) ;
#31938 = CARTESIAN_POINT ( 'NONE',  ( 6.398740975593778302, -284.6456943985136263, -209.3728041133678346 ) ) ;
#31939 = CARTESIAN_POINT ( 'NONE',  ( -39.94463377582687258, -275.2240852786313212, -346.0940523342308097 ) ) ;
#31940 = DIRECTION ( 'NONE',  ( -1.000000000000000000, -0.000000000000000000, -0.000000000000000000 ) ) ;
#31941 = CARTESIAN_POINT ( 'NONE',  ( -51.03557406219254489, -282.7394153745999574, -342.1794875296856731 ) ) ;
#31942 = CARTESIAN_POINT ( 'NONE',  ( -45.24773267194631643, -281.1593317729493720, -194.1145467414838208 ) ) ;
#31943 = CARTESIAN_POINT ( 'NONE',  ( 30.15008815713381907, -287.0867521836036644, -307.0465474153882610 ) ) ;
#31944 = CARTESIAN_POINT ( 'NONE',  ( -39.69916556040571010, -296.8422720438277906, -344.3495036058563983 ) ) ;
#31945 = CARTESIAN_POINT ( 'NONE',  ( 19.29637331677102452, -277.8516235887336165, -321.3568127997767192 ) ) ;
#31946 = CARTESIAN_POINT ( 'NONE',  ( 28.07215220619743334, -276.3448830913356460, -230.5820953063862646 ) ) ;
#31947 = CARTESIAN_POINT ( 'NONE',  ( -96.88692640626264563, -277.7955435774362627, -312.6127471272376965 ) ) ;
#31948 = CARTESIAN_POINT ( 'NONE',  ( -67.58300229782625479, -299.6546725945485150, -201.8964377673428601 ) ) ;
#31949 = CARTESIAN_POINT ( 'NONE',  ( 27.97982403285748276, -285.0635795132146200, -233.7430230635522150 ) ) ;
#31950 = CARTESIAN_POINT ( 'NONE',  ( -112.8759555970320463, -292.2841868556409395, -259.9233491448626978 ) ) ;
#31951 = CARTESIAN_POINT ( 'NONE',  ( -36.18752924115639757, -290.9872492672425892, -197.0485618474658907 ) ) ;
#31952 = ORIENTED_EDGE ( 'NONE', *, *, #63462, .T. ) ;
#31953 = CARTESIAN_POINT ( 'NONE',  ( -30.80085406721504171, -291.8038276289709074, -197.6335109850780611 ) ) ;
#31954 = ORIENTED_EDGE ( 'NONE', *, *, #37042, .F. ) ;
#31955 = CARTESIAN_POINT ( 'NONE',  ( -45.97725273223464626, -290.2387521758650450, -346.6171789037773010 ) ) ;
#31956 = CARTESIAN_POINT ( 'NONE',  ( -54.52478548652082679, -280.4770368167814922, -199.2551044200497188 ) ) ;
#31957 = CARTESIAN_POINT ( 'NONE',  ( -105.6884919800661322, -295.0213861220104263, -305.2661931755152409 ) ) ;
#31958 = CARTESIAN_POINT ( 'NONE',  ( 32.61584204828126587, -287.7934497353121515, -238.3071889476116212 ) ) ;
#31959 = CARTESIAN_POINT ( 'NONE',  ( 5.164463920278626219, -286.9429476111998270, -206.1184260131755934 ) ) ;
#31960 = CARTESIAN_POINT ( 'NONE',  ( -88.90621632563291143, -284.1342473866651517, -322.1349688073923971 ) ) ;
#31961 = CARTESIAN_POINT ( 'NONE',  ( -95.69098327614956645, -240.0217764934971001, -341.7741963911435619 ) ) ;
#31962 = CARTESIAN_POINT ( 'NONE',  ( -112.8381603000581350, -269.0091090816746942, -295.8145170300798554 ) ) ;
#31963 = CARTESIAN_POINT ( 'NONE',  ( -89.05334355809267777, -229.2207001999348677, -344.3638864873447005 ) ) ;
#31964 = AXIS2_PLACEMENT_3D ( 'NONE', #68516, #4120, #54295 ) ;
#31965 = CARTESIAN_POINT ( 'NONE',  ( -69.33123261485080491, -276.6812832171280547, -336.1721864582053740 ) ) ;
#31966 = CARTESIAN_POINT ( 'NONE',  ( -61.90630208261759293, -276.2992970384053706, -339.4861145567745666 ) ) ;
#31967 = CARTESIAN_POINT ( 'NONE',  ( -99.54745726220131985, -272.8218831187957107, -224.9275258499349945 ) ) ;
#31968 = CARTESIAN_POINT ( 'NONE',  ( -109.1411030854801680, -269.7224105353499226, -295.4917919841202547 ) ) ;
#31969 = CARTESIAN_POINT ( 'NONE',  ( -111.6998803920500194, -277.0096726131649802, -288.4204631147621853 ) ) ;
#31970 = EDGE_LOOP ( 'NONE', ( #61434, #14826, #51298, #60157 ) ) ;
#31971 = CARTESIAN_POINT ( 'NONE',  ( -108.1696792713219537, -291.2815145907476335, -252.3829820995457283 ) ) ;
#31972 = CARTESIAN_POINT ( 'NONE',  ( -34.77642259965058713, -298.8863312046613601, -193.5222535600145477 ) ) ;
#31973 = CARTESIAN_POINT ( 'NONE',  ( -73.25748586429388354, -298.0816139074282205, -202.2612753892758235 ) ) ;
#31974 = CARTESIAN_POINT ( 'NONE',  ( -35.64848614041083152, -295.1970355033479336, -343.3539746444233742 ) ) ;
#31975 = ORIENTED_EDGE ( 'NONE', *, *, #62639, .F. ) ;
#31976 = CARTESIAN_POINT ( 'NONE',  ( -81.68114528108452532, -279.5708025579765490, -331.5438590043891054 ) ) ;
#31977 = CARTESIAN_POINT ( 'NONE',  ( 9.166618469806152802, -281.9401319130670345, -331.6514369918072020 ) ) ;
#31978 = CARTESIAN_POINT ( 'NONE',  ( -83.18941239012731614, -278.7765105923450051, -327.6297055266257985 ) ) ;
#31979 = CARTESIAN_POINT ( 'NONE',  ( 22.73089993036286671, -277.9420915592434653, -316.9145473372589095 ) ) ;
#31980 = CARTESIAN_POINT ( 'NONE',  ( -34.43264168466875930, -296.6639937130342446, -196.7726070210977127 ) ) ;
#31981 = CARTESIAN_POINT ( 'NONE',  ( 222.8344101925596306, -44.55766379199612004, 22.50000000000000000 ) ) ;
#31982 = CARTESIAN_POINT ( 'NONE',  ( -97.64763201024906891, -278.1465152655208044, -311.4974107704672406 ) ) ;
#31983 = CARTESIAN_POINT ( 'NONE',  ( 17.96624922607475483, -275.6223732806200246, -216.9444315659675055 ) ) ;
#31984 = CARTESIAN_POINT ( 'NONE',  ( -5.844916577696278814, -287.3314721402164764, -340.0837893332466138 ) ) ;
#31985 = CARTESIAN_POINT ( 'NONE',  ( -38.35657888232754686, -276.0395859197232085, -195.3679804698540181 ) ) ;
#31986 = CARTESIAN_POINT ( 'NONE',  ( 23.04116999833489388, -274.7571934940123697, -317.2066346513356052 ) ) ;
#31987 = DIRECTION ( 'NONE',  ( 1.000000000000000000, 0.000000000000000000, 0.000000000000000000 ) ) ;
#31988 = CARTESIAN_POINT ( 'NONE',  ( -70.05382376342366513, -288.6916700083741603, -335.8159647033965030 ) ) ;
#31989 = CARTESIAN_POINT ( 'NONE',  ( -110.8261557548513139, -284.1876919767618688, -247.5247831497662219 ) ) ;
#31990 = CARTESIAN_POINT ( 'NONE',  ( 23.40381856939280070, -280.3733317625773225, -312.6453463948412264 ) ) ;
#31992 = CARTESIAN_POINT ( 'NONE',  ( -41.37701451950836429, -284.0808237527692768, -196.0178244446223630 ) ) ;
#31991 = CARTESIAN_POINT ( 'NONE',  ( -5.285548949164077470, -279.0572488752454205, -204.1208123464883784 ) ) ;
#31993 = CARTESIAN_POINT ( 'NONE',  ( -62.47099950814151725, -291.3791134923286563, -341.0802947170757307 ) ) ;
#31994 = CARTESIAN_POINT ( 'NONE',  ( -109.6747952858519994, -279.5928836896200664, -282.8873786463282158 ) ) ;
#31995 = CARTESIAN_POINT ( 'NONE',  ( 138.5464851867201617, 180.7133913485274093, -241.3450705794696205 ) ) ;
#31996 = CARTESIAN_POINT ( 'NONE',  ( -24.68671676498891543, -281.2932795958516863, -345.5564807554345066 ) ) ;
#31997 = CARTESIAN_POINT ( 'NONE',  ( 33.55350136275063022, -295.2337867552957960, -245.7322287256875484 ) ) ;
#31998 = CARTESIAN_POINT ( 'NONE',  ( -74.49267372065884274, -277.8048166309754947, -204.0755299897761006 ) ) ;
#31999 = CARTESIAN_POINT ( 'NONE',  ( -65.85659864257682727, -285.4244470034578853, -339.9229974522152133 ) ) ;
#32000 = CARTESIAN_POINT ( 'NONE',  ( 197.6897354370363473, 68.42890619940936858, 10.08371065145146872 ) ) ;
#32001 = CARTESIAN_POINT ( 'NONE',  ( -76.44537179901922741, -293.4540489764297604, -205.6461673090609850 ) ) ;
#32002 = CARTESIAN_POINT ( 'NONE',  ( 21.57826782591973114, -274.1893918477034617, -316.7869431542051188 ) ) ;
#32003 = CARTESIAN_POINT ( 'NONE',  ( 2.665679482944644629, -285.7715786691190942, -204.7595296100580526 ) ) ;
#32004 = CARTESIAN_POINT ( 'NONE',  ( -90.37722399140584173, -289.6856194578234636, -219.0417880621873792 ) ) ;
#32005 = CARTESIAN_POINT ( 'NONE',  ( -48.18343439339133027, -263.2279375582672856, -443.0391293175771352 ) ) ;
#32006 = CARTESIAN_POINT ( 'NONE',  ( 20.39958492059878026, -274.8742674453797008, -315.8477130392956269 ) ) ;
#32007 = CARTESIAN_POINT ( 'NONE',  ( -47.99330059431824225, -293.3285065996022354, -343.8803275178525496 ) ) ;
#32008 = CARTESIAN_POINT ( 'NONE',  ( -113.5000000000000568, -190.7866584945343504, -447.4016117689005796 ) ) ;
#32009 = CARTESIAN_POINT ( 'NONE',  ( 201.6359441630863500, 62.93935058108146308, 6.999999999999996447 ) ) ;
#32010 = CARTESIAN_POINT ( 'NONE',  ( 25.92896271279305154, -291.4638424328961719, -227.6121752193068914 ) ) ;
#32011 = CARTESIAN_POINT ( 'NONE',  ( -105.3425452505865962, -286.5345412973486532, -241.5534608477831853 ) ) ;
#32012 = CARTESIAN_POINT ( 'NONE',  ( -2.288377031563566533, -286.8345532044896800, -337.7795023884337979 ) ) ;
#32013 = CARTESIAN_POINT ( 'NONE',  ( 0.4558526818627712252, -287.9913483902537337, -207.1612409286476009 ) ) ;
#32014 = CARTESIAN_POINT ( 'NONE',  ( 199.9311642430739653, 275.7557892102190067, -9.103929867429339851 ) ) ;
#32015 = CARTESIAN_POINT ( 'NONE',  ( 35.79188056954839681, -288.3996901881048984, -273.7571519457596310 ) ) ;
#32016 = CARTESIAN_POINT ( 'NONE',  ( 29.42954581387986224, -295.0702523157631276, -235.3202499388733884 ) ) ;
#32017 = CARTESIAN_POINT ( 'NONE',  ( -35.09237171215954731, -55.96374926131388605, 22.50000000000000000 ) ) ;
#32018 = CARTESIAN_POINT ( 'NONE',  ( 13.96946583782010620, -287.9580253817053404, -213.4113852361003012 ) ) ;
#32019 = CARTESIAN_POINT ( 'NONE',  ( -103.7224080617017847, -276.1560174391986493, -306.4570430947074442 ) ) ;
#32020 = CIRCLE ( 'NONE', #3288, 6.500000000000033751 ) ;
#32021 = CARTESIAN_POINT ( 'NONE',  ( -95.19209669629114501, -278.1979918697487051, -321.1457210475748525 ) ) ;
#32022 = AXIS2_PLACEMENT_3D ( 'NONE', #85814, #92929, #64565 ) ;
#32023 = CARTESIAN_POINT ( 'NONE',  ( 22.86143368094143113, -280.5762170911689850, -222.3680122932001666 ) ) ;
#32024 = CARTESIAN_POINT ( 'NONE',  ( -66.23208441319731321, -299.6519751437826358, -201.5338523080350228 ) ) ;
#32025 = CARTESIAN_POINT ( 'NONE',  ( -48.18343439343219359, -265.6641742835798823, -502.8827764852874225 ) ) ;
#32026 = CARTESIAN_POINT ( 'NONE',  ( -19.31102908077654945, -284.2839792367648215, -197.5607364776439852 ) ) ;
#32027 = CARTESIAN_POINT ( 'NONE',  ( 202.8019728163925492, 61.40723988820079171, -7.000000000000000888 ) ) ;
#32028 = CARTESIAN_POINT ( 'NONE',  ( -109.3763362795433380, -276.4583063858643754, -288.3545119142069666 ) ) ;
#32029 = CARTESIAN_POINT ( 'NONE',  ( 16.37555915972660259, -280.2894872585930557, -322.7751182829704817 ) ) ;
#32030 = DIRECTION ( 'NONE',  ( 1.000000000000000000, 0.000000000000000000, 0.000000000000000000 ) ) ;
#32031 = CARTESIAN_POINT ( 'NONE',  ( -14.81303407438512920, -275.2454511245171034, -343.3216278436320295 ) ) ;
#32032 = AXIS2_PLACEMENT_3D ( 'NONE', #35874, #58133, #6065 ) ;
#32033 = CARTESIAN_POINT ( 'NONE',  ( -78.31935103185020353, -297.1342574607348865, -331.6725587702009648 ) ) ;
#32034 = CARTESIAN_POINT ( 'NONE',  ( 6.736064839718973296, -281.3887484030951782, -333.1846588522895445 ) ) ;
#32035 = CARTESIAN_POINT ( 'NONE',  ( -57.98253738569656690, -298.7201153642972713, -200.0947370821152731 ) ) ;
#32036 = CARTESIAN_POINT ( 'NONE',  ( -96.97257719552548849, -298.5138026828739726, -222.4293250339174790 ) ) ;
#32037 = CARTESIAN_POINT ( 'NONE',  ( -29.98351685608239592, -273.8145655281006725, -197.7116539398417672 ) ) ;
#32038 = CARTESIAN_POINT ( 'NONE',  ( 37.42006093121500498, -295.6290118130862083, -276.3343691895940424 ) ) ;
#32039 = CARTESIAN_POINT ( 'NONE',  ( 30.13053733563801018, -287.2370886836560544, -233.1493159620859501 ) ) ;
#32040 = CARTESIAN_POINT ( 'NONE',  ( -110.6821945957990749, -276.8643752507669547, -252.1288293495414052 ) ) ;
#32041 = CARTESIAN_POINT ( 'NONE',  ( -106.0031489579009474, -290.8354881621830259, -235.3923703725757832 ) ) ;
#32042 = EDGE_CURVE ( 'NONE', #35022, #60748, #55993, .T. ) ;
#32043 = CARTESIAN_POINT ( 'NONE',  ( 17.07345212859976513, -285.9111754903252063, -221.3281124510065752 ) ) ;
#32044 = CARTESIAN_POINT ( 'NONE',  ( 37.24020743009980805, -291.4443189532779570, -261.9755118474089954 ) ) ;
#32045 = EDGE_LOOP ( 'NONE', ( #46274, #43050 ) ) ;
#32046 = CARTESIAN_POINT ( 'NONE',  ( 207.9738562182569979, 296.4636489450776367, -53.99999999999996447 ) ) ;
#32047 = CARTESIAN_POINT ( 'NONE',  ( -10.70750508443766336, -288.2029641790746837, -338.4492520772749913 ) ) ;
#32048 = CARTESIAN_POINT ( 'NONE',  ( 202.9228084772383340, 300.2547313093774619, -4.941765029749829452 ) ) ;
#32049 = CARTESIAN_POINT ( 'NONE',  ( -74.15258365676309893, -284.4699494192838642, -337.7834632798797543 ) ) ;
#32050 = CARTESIAN_POINT ( 'NONE',  ( -25.04727851266873273, -291.2640311931895667, -194.5873269362672318 ) ) ;
#32051 = CARTESIAN_POINT ( 'NONE',  ( 22.23692858310425535, -282.5093135698551805, -222.8343035938656271 ) ) ;
#32052 = CARTESIAN_POINT ( 'NONE',  ( -35.36565949769887851, -281.3916044359212947, -193.8667371012928413 ) ) ;
#32053 = CARTESIAN_POINT ( 'NONE',  ( -76.12892137985416241, -283.4192246183785642, -332.2638588864539315 ) ) ;
#32054 = CARTESIAN_POINT ( 'NONE',  ( -100.7506633848914532, -297.1291343217696976, -226.6538149999235259 ) ) ;
#32055 = CARTESIAN_POINT ( 'NONE',  ( -105.8821865621944482, -274.2210059718004800, -243.6981114570576210 ) ) ;
#32056 = CARTESIAN_POINT ( 'NONE',  ( 22.32338184616281396, -290.9563049268516011, -225.5066332715741169 ) ) ;
#32057 = CARTESIAN_POINT ( 'NONE',  ( -40.77825468412755328, -272.8030252614012738, -196.9945683960216627 ) ) ;
#32058 = ORIENTED_EDGE ( 'NONE', *, *, #50406, .F. ) ;
#32059 = CARTESIAN_POINT ( 'NONE',  ( 186.2362647323748490, 249.5000000000000568, 22.80382896336987031 ) ) ;
#32060 = CARTESIAN_POINT ( 'NONE',  ( -72.05922115847914711, -285.4351851772863142, -336.2094887573258575 ) ) ;
#32061 = CARTESIAN_POINT ( 'NONE',  ( -53.21179875707857576, -296.3305898399432863, -345.4463168423347383 ) ) ;
#32062 = CARTESIAN_POINT ( 'NONE',  ( -108.8179802862372156, -285.0008273800320353, -285.7513601206922544 ) ) ;
#32063 = CARTESIAN_POINT ( 'NONE',  ( 10.37040957557863230, -275.4709780767523171, -330.5652885095761917 ) ) ;
#32064 = CARTESIAN_POINT ( 'NONE',  ( -2.109941594086266914, -293.1575623248617717, -201.9940674419532058 ) ) ;
#32065 = CARTESIAN_POINT ( 'NONE',  ( 35.58887856450918008, -285.9537473155775160, -290.9375527471842133 ) ) ;
#32066 = CARTESIAN_POINT ( 'NONE',  ( -3.334518190640860524, -292.8221923266876843, -201.2867855567963602 ) ) ;
#32067 = CARTESIAN_POINT ( 'NONE',  ( -95.78269330669334636, -290.2708205165193363, -314.1625476471908769 ) ) ;
#32068 = DIRECTION ( 'NONE',  ( -0.2156506209390900430, 0.000000000000000000, -0.9764705882352960886 ) ) ;
#32069 = DIRECTION ( 'NONE',  ( 2.220446049250312686E-15, 0.000000000000000000, 1.000000000000000000 ) ) ;
#32070 = CARTESIAN_POINT ( 'NONE',  ( -21.32748300042747047, -109.1711728762462599, -358.9589870467152082 ) ) ;
#32071 = CARTESIAN_POINT ( 'NONE',  ( -95.30271994553761772, -286.7486808275992871, -220.6509291276668705 ) ) ;
#32072 = CARTESIAN_POINT ( 'NONE',  ( -111.2869819898779866, -275.6237833571633473, -305.9350535429201159 ) ) ;
#32073 = ORIENTED_EDGE ( 'NONE', *, *, #85946, .F. ) ;
#32074 = CARTESIAN_POINT ( 'NONE',  ( -61.65013534321383304, -282.2957530560925079, -339.5761776175779119 ) ) ;
#32075 = CARTESIAN_POINT ( 'NONE',  ( -113.0456101871530592, -278.0434275631234868, -284.3857043565927256 ) ) ;
#32076 = CARTESIAN_POINT ( 'NONE',  ( -39.78600746564308821, -282.0215683001354705, -195.5548766155741021 ) ) ;
#32077 = CARTESIAN_POINT ( 'NONE',  ( -75.54299273995306407, -209.4449673374598149, -355.7036186976513932 ) ) ;
#32078 = CARTESIAN_POINT ( 'NONE',  ( -37.33268361118738454, -281.6267396580638547, -346.7848558294755890 ) ) ;
#32079 = CARTESIAN_POINT ( 'NONE',  ( 20.81214822973163336, -284.9250317276720352, -223.5436714221757484 ) ) ;
#32080 = CARTESIAN_POINT ( 'NONE',  ( -108.0229871219324025, -274.7654568338024887, -242.9317705756486419 ) ) ;
#32081 = CARTESIAN_POINT ( 'NONE',  ( -45.09103359206184081, -295.6451422462782261, -343.0610436786520268 ) ) ;
#32082 = ORIENTED_EDGE ( 'NONE', *, *, #19750, .T. ) ;
#32083 = CARTESIAN_POINT ( 'NONE',  ( -3.393670155583646597, -291.1950900457537728, -205.1784919218372067 ) ) ;
#32084 = CARTESIAN_POINT ( 'NONE',  ( -97.84356587086362822, -278.5682003954476045, -317.8251783733547882 ) ) ;
#32085 = CARTESIAN_POINT ( 'NONE',  ( 19.85550291320718941, -274.9116816451208933, -224.9816635841000618 ) ) ;
#32086 = CARTESIAN_POINT ( 'NONE',  ( 21.48464173678410916, -275.1373264880589886, -319.5643090745783752 ) ) ;
#32087 = CARTESIAN_POINT ( 'NONE',  ( 41.08708295871279859, -293.9068999365417199, -465.6442049081569508 ) ) ;
#32088 = CARTESIAN_POINT ( 'NONE',  ( -25.24924945877150861, -272.2060155210314747, -196.2903500954780327 ) ) ;
#32089 = CARTESIAN_POINT ( 'NONE',  ( 24.42080315769786125, -295.5793515982531403, -315.3720463854793934 ) ) ;
#32090 = CARTESIAN_POINT ( 'NONE',  ( 153.7504314680575987, 128.6410103095127226, 12.94315874461255689 ) ) ;
#32091 = AXIS2_PLACEMENT_3D ( 'NONE', #60315, #10556, #31883 ) ;
#32092 = CARTESIAN_POINT ( 'NONE',  ( 195.2616234104794728, 71.31492948064700954, 13.29451844366211866 ) ) ;
#32093 = CIRCLE ( 'NONE', #88034, 26.99999999999999289 ) ;
#32094 = CARTESIAN_POINT ( 'NONE',  ( -80.79836427686932154, -284.7369270057944277, -329.4644607051857861 ) ) ;
#32095 = CARTESIAN_POINT ( 'NONE',  ( 17.11590623432395475, -284.0491827155746591, -323.4301284291572074 ) ) ;
#32096 = CARTESIAN_POINT ( 'NONE',  ( -109.0272987253608363, -284.0893804607008519, -256.0409356430674848 ) ) ;
#32097 = CARTESIAN_POINT ( 'NONE',  ( 14.27647268826083859, -274.7122533925004859, -323.1769808572024658 ) ) ;
#32098 = CARTESIAN_POINT ( 'NONE',  ( -56.61717963045364144, -285.1637002456756704, -342.0501782889522815 ) ) ;
#32099 = CARTESIAN_POINT ( 'NONE',  ( -98.23252094285805924, -276.4599854975878657, -311.8703421778951110 ) ) ;
#32100 = EDGE_CURVE ( 'NONE', #82047, #58642, #77747, .T. ) ;
#32101 =( GEOMETRIC_REPRESENTATION_CONTEXT ( 3 ) GLOBAL_UNCERTAINTY_ASSIGNED_CONTEXT ( ( #36837 ) ) GLOBAL_UNIT_ASSIGNED_CONTEXT ( ( #76509, #40946, #40478 ) ) REPRESENTATION_CONTEXT ( 'NONE', 'WORKASPACE' ) );
#32102 = CARTESIAN_POINT ( 'NONE',  ( 35.32510718580935816, -276.5046316906208972, -260.6780818678755622 ) ) ;
#32103 = EDGE_CURVE ( 'NONE', #63802, #31343, #80773, .T. ) ;
#32104 = CYLINDRICAL_SURFACE ( 'NONE', #13936, 24.00000000000000355 ) ;
#32105 = AXIS2_PLACEMENT_3D ( 'NONE', #76977, #54713, #91636 ) ;
#32106 = CARTESIAN_POINT ( 'NONE',  ( -36.76405678750610662, -280.8620680775485425, -193.5117469678797022 ) ) ;
#32107 = CARTESIAN_POINT ( 'NONE',  ( -64.72629259894902987, -280.1964588649249777, -198.4049243463213088 ) ) ;
#32108 = ORIENTED_EDGE ( 'NONE', *, *, #12755, .F. ) ;
#32109 = ORIENTED_EDGE ( 'NONE', *, *, #48515, .F. ) ;
#32110 = CARTESIAN_POINT ( 'NONE',  ( 82.64890176555634582, -299.5541904835127980, -195.3611179825600175 ) ) ;
#32111 = CARTESIAN_POINT ( 'NONE',  ( -24.02664636421022237, -288.0807479783902636, -195.7221530634781459 ) ) ;
#32112 = CARTESIAN_POINT ( 'NONE',  ( -26.19286370360628169, -294.1037444226016646, -342.6681382016752764 ) ) ;
#32113 = CARTESIAN_POINT ( 'NONE',  ( -112.7696401988369814, -289.7125050854687629, -285.3924768128118217 ) ) ;
#32114 = B_SPLINE_CURVE_WITH_KNOTS ( 'NONE', 3,
 ( #65146, #73156, #7346, #15382, #22034, #43335, #44246, #73618, #30061, #247, #50439, #7803, #36690, #14929, #58946, #8279, #78853, #57101, #14003, #43784, #71777, #29130, #42863, #37159, #66068, #85941, #724, #87794, #22943, #93057, #6900 ),
 .UNSPECIFIED., .F., .F.,
 ( 4, 2, 2, 2, 1, 2, 2, 2, 2, 2, 2, 2, 2, 2, 2, 4 ),
 ( 0.000000000000000000, 0.005913895122008330264, 0.007392368902510404807, 0.008870842683012480218, 0.01182779024401667614, 0.01478473780502087206, 0.01626321158552301166, 0.01774168536602514779, 0.02365558048803392821, 0.02661252804903820046, 0.02809100182954044761, 0.02956947561004270170, 0.03548337073205194009, 0.03844031829305656622, 0.04139726585406118542, 0.04731116097607026422 ),
 .UNSPECIFIED. ) ;
#32115 = CARTESIAN_POINT ( 'NONE',  ( 33.24670168618867905, -285.5005518376915461, -248.0643989013786097 ) ) ;
#32117 = CARTESIAN_POINT ( 'NONE',  ( -73.09709437192304904, -289.8116019873651794, -205.4997853387870066 ) ) ;
#32116 = CARTESIAN_POINT ( 'NONE',  ( 35.58255743526108006, -285.9928287594933067, -260.1177032164763432 ) ) ;
#32118 = CARTESIAN_POINT ( 'NONE',  ( -25.09056769541773235, -287.4167986635021634, -197.9421444574102509 ) ) ;
#32119 = CARTESIAN_POINT ( 'NONE',  ( -112.2127695572321500, -276.6084302456295632, -265.9652553019528796 ) ) ;
#32120 = CARTESIAN_POINT ( 'NONE',  ( 36.00873599911082579, -286.2139928166764662, -291.0524191956897084 ) ) ;
#32121 = CARTESIAN_POINT ( 'NONE',  ( 33.94000919001867800, -289.2491378173115208, -246.8731416063353947 ) ) ;
#32122 = CARTESIAN_POINT ( 'NONE',  ( 24.85504240161681366, -284.9816810451083029, -228.1291856884065226 ) ) ;
#32123 = CARTESIAN_POINT ( 'NONE',  ( 35.66462184815443948, -282.5775475765608462, -276.7598081705659183 ) ) ;
#32124 = CARTESIAN_POINT ( 'NONE',  ( 20.10476282909932166, -290.2212647467921443, -318.8372185212502927 ) ) ;
#32125 = CARTESIAN_POINT ( 'NONE',  ( 208.6208076322478746, 32.98517505407394168, 13.08022668053247095 ) ) ;
#32126 = CARTESIAN_POINT ( 'NONE',  ( 155.4162060973593213, 20.04122387618562939, -15.25295451850657358 ) ) ;
#32127 = CARTESIAN_POINT ( 'NONE',  ( -62.39115482748979957, -299.6489439279044973, -199.0740994153643442 ) ) ;
#32128 = CARTESIAN_POINT ( 'NONE',  ( 29.57710527583184756, -279.1031206910064384, -236.3803571566485857 ) ) ;
#32129 = CARTESIAN_POINT ( 'NONE',  ( -50.52857049235809228, -291.0850188997316650, -194.6626023429500094 ) ) ;
#32130 = CARTESIAN_POINT ( 'NONE',  ( -110.6011763037998747, -294.8303284794328647, -279.6869412284991085 ) ) ;
#32131 = CARTESIAN_POINT ( 'NONE',  ( 34.41833540617255238, -280.4448749674814394, -286.2274590782195673 ) ) ;
#32132 = CARTESIAN_POINT ( 'NONE',  ( -68.87066569254632498, -271.7142674303379408, -202.9139362639011495 ) ) ;
#32133 = CARTESIAN_POINT ( 'NONE',  ( -63.73052980004775492, -296.7185716184507100, -339.0071099239967225 ) ) ;
#32134 = FILL_AREA_STYLE ('',( #2787 ) ) ;
#32135 = CARTESIAN_POINT ( 'NONE',  ( 97.67869099132846600, -298.1933505581249619, -194.0885504402530728 ) ) ;
#32136 = CARTESIAN_POINT ( 'NONE',  ( 24.87193957083375295, -292.3769067849592034, -314.0122142888834560 ) ) ;
#32137 = CARTESIAN_POINT ( 'NONE',  ( -60.46116585165769663, -293.1717801410790685, -200.4444552939437187 ) ) ;
#32138 = DIRECTION ( 'NONE',  ( 0.000000000000000000, 0.000000000000000000, 1.000000000000000000 ) ) ;
#32139 = CARTESIAN_POINT ( 'NONE',  ( 30.00038310982760947, -293.9703699323951014, -241.6370488712062752 ) ) ;
#32140 = DIRECTION ( 'NONE',  ( -0.000000000000000000, 0.000000000000000000, 1.000000000000000000 ) ) ;
#32142 = CARTESIAN_POINT ( 'NONE',  ( -26.20740738324616714, -294.9064477241673217, -342.5069946843668731 ) ) ;
#32141 = CARTESIAN_POINT ( 'NONE',  ( -106.7228214564766517, -282.1882831759584178, -299.8999288511420218 ) ) ;
#32143 = CARTESIAN_POINT ( 'NONE',  ( 33.56592810279381212, -281.9357346024767708, -300.5157485781939499 ) ) ;
#32144 = CARTESIAN_POINT ( 'NONE',  ( 9.903215597816359406, -282.6168194147061854, -211.3260124695724471 ) ) ;
#32145 = CARTESIAN_POINT ( 'NONE',  ( -26.61985071651751156, -285.8515771332424151, -194.0791202020755861 ) ) ;
#32146 = CARTESIAN_POINT ( 'NONE',  ( -93.92647831743205700, -289.2327514552350181, -221.3897865101162097 ) ) ;
#32147 = CARTESIAN_POINT ( 'NONE',  ( -34.52412969220306138, -281.4972230269272586, -346.6157509629684910 ) ) ;
#32148 = CARTESIAN_POINT ( 'NONE',  ( -40.34049286915740140, -288.0093238300307235, -347.0063840666759347 ) ) ;
#32149 = CARTESIAN_POINT ( 'NONE',  ( -48.18343439339133027, -291.0521521680024080, -435.6442049081568939 ) ) ;
#32150 = CARTESIAN_POINT ( 'NONE',  ( -70.06062047065620391, -297.0907504691072631, -336.5117995295676110 ) ) ;
#32151 = CARTESIAN_POINT ( 'NONE',  ( -71.29260842501039974, -278.9169105144516152, -338.8150595858230076 ) ) ;
#32153 = CARTESIAN_POINT ( 'NONE',  ( -22.18587604685646397, -279.9182442886329341, -198.8782400538389368 ) ) ;
#32152 = CARTESIAN_POINT ( 'NONE',  ( 37.96226306148032137, -291.6077645447603572, -273.1395938017559502 ) ) ;
#32154 = CARTESIAN_POINT ( 'NONE',  ( 36.70357884842792373, -293.4534699618284321, -249.1873445060794268 ) ) ;
#32155 = CARTESIAN_POINT ( 'NONE',  ( -110.3238210573160814, -282.8839533935214945, -250.5962620008469059 ) ) ;
#32156 = CARTESIAN_POINT ( 'NONE',  ( -28.80276998113174969, -278.9441809999948418, -344.9256331223715506 ) ) ;
#32157 = CARTESIAN_POINT ( 'NONE',  ( 35.77039601752356646, -292.5445027382672265, -265.3120231461800813 ) ) ;
#32158 = CIRCLE ( 'NONE', #10982, 2.000000000000001776 ) ;
#32159 = CARTESIAN_POINT ( 'NONE',  ( -101.1489920581274617, -271.0844958157555311, -230.6287895603641687 ) ) ;
#32160 = ORIENTED_EDGE ( 'NONE', *, *, #22050, .T. ) ;
#32161 = CARTESIAN_POINT ( 'NONE',  ( 190.2832783574276903, 8.542400036368780647, 9.000000000000001776 ) ) ;
#32162 = CIRCLE ( 'NONE', #92641, 0.4999999999999983347 ) ;
#32163 = CARTESIAN_POINT ( 'NONE',  ( 32.40368120952480524, -293.3479379400545781, -292.1227866632826817 ) ) ;
#32164 = CARTESIAN_POINT ( 'NONE',  ( 208.4306832106270804, -199.2391364535880882, 0.000000000000000000 ) ) ;
#32165 = CARTESIAN_POINT ( 'NONE',  ( -92.08974858914540107, -293.4094976428775681, -313.9805196606274080 ) ) ;
#32166 = CARTESIAN_POINT ( 'NONE',  ( -101.0688888548078666, -272.3171808282273219, -227.3361863632982534 ) ) ;
#32167 = CARTESIAN_POINT ( 'NONE',  ( 34.38603150638219574, -288.5286359645543826, -243.7447548483897322 ) ) ;
#32168 = CARTESIAN_POINT ( 'NONE',  ( 31.39868659444720222, -287.7126360876585522, -294.9326307103727345 ) ) ;
#32169 = VECTOR ( 'NONE', #78468, 1000.000000000000000 ) ;
#32170 = CARTESIAN_POINT ( 'NONE',  ( -97.44001153033948981, -279.4820731503508000, -313.0315984227354988 ) ) ;
#32171 = CARTESIAN_POINT ( 'NONE',  ( -36.49091421304517269, -299.8230862102235506, -196.3475185273377122 ) ) ;
#32172 = CARTESIAN_POINT ( 'NONE',  ( -96.71793929998518990, -277.9476640710905144, -227.2149393871871723 ) ) ;
#32173 = EDGE_LOOP ( 'NONE', ( #86260, #48009, #63311, #11264 ) ) ;
#32174 = CARTESIAN_POINT ( 'NONE',  ( -114.1808714800626916, -272.4572214948289002, -264.6241286613252441 ) ) ;
#32175 = CARTESIAN_POINT ( 'NONE',  ( -60.73423236463455765, -293.6665821841398838, -199.6380524494565520 ) ) ;
#32176 = CARTESIAN_POINT ( 'NONE',  ( 22.46734290608615581, -294.5138773816356093, -223.1246125363533395 ) ) ;
#32177 = FACE_OUTER_BOUND ( 'NONE', #62147, .T. ) ;
#32178 = CARTESIAN_POINT ( 'NONE',  ( -107.0467789165242891, -290.9100151247752706, -292.5533464571436753 ) ) ;
#32179 = LINE ( 'NONE', #66768, #5825 ) ;
#32180 = CARTESIAN_POINT ( 'NONE',  ( -27.97787172230660246, -290.3092628590002278, -195.1243673037924680 ) ) ;
#32181 = CARTESIAN_POINT ( 'NONE',  ( -77.52006940727925155, -297.1636004414818899, -209.3267083803866910 ) ) ;
#32182 = DIRECTION ( 'NONE',  ( 0.000000000000000000, 0.000000000000000000, 1.000000000000000000 ) ) ;
#32183 = CARTESIAN_POINT ( 'NONE',  ( -108.1478418983590757, -291.7079662112038250, -298.8075244133791557 ) ) ;
#32184 = CARTESIAN_POINT ( 'NONE',  ( -2.602324593224680793, -297.1233781216987495, -342.4248175857292154 ) ) ;
#32185 = CARTESIAN_POINT ( 'NONE',  ( -38.68267965962606780, -288.0354893360201345, -195.5270013178786428 ) ) ;
#32186 = CARTESIAN_POINT ( 'NONE',  ( 28.25556057384566344, -273.0708667715167053, -234.2387795365413865 ) ) ;
#32187 = CARTESIAN_POINT ( 'NONE',  ( -3.470884329266651580, -276.4229604262348516, -204.0589377984777286 ) ) ;
#32188 = CARTESIAN_POINT ( 'NONE',  ( -22.42870598061681520, -290.3244204270775413, -197.4302136928437790 ) ) ;
#32189 = CARTESIAN_POINT ( 'NONE',  ( -112.8459830926621663, -280.3250994698489649, -277.2428428359876875 ) ) ;
#32190 = AXIS2_PLACEMENT_3D ( 'NONE', #3861, #76762, #18064 ) ;
#32191 = VERTEX_POINT ( 'NONE', #48875 ) ;
#32192 = CARTESIAN_POINT ( 'NONE',  ( 9.968359227623851737, -281.7288842460441174, -326.1560474453642655 ) ) ;
#32193 = CARTESIAN_POINT ( 'NONE',  ( -91.10250224597039903, -278.8736926504901135, -325.1279636279851957 ) ) ;
#32194 = CARTESIAN_POINT ( 'NONE',  ( 37.75324310583263809, -280.5372181615706495, -285.4858732045136662 ) ) ;
#32195 = CARTESIAN_POINT ( 'NONE',  ( 63.42269039470908609, 47.43533074464846777, -315.9655852024159230 ) ) ;
#32196 = CARTESIAN_POINT ( 'NONE',  ( 32.80961911128900255, -276.8924477317431752, -301.5318193105213140 ) ) ;
#32197 = CARTESIAN_POINT ( 'NONE',  ( -15.99008950958257991, -275.8433804732711110, -197.0477229558706256 ) ) ;
#32198 = CARTESIAN_POINT ( 'NONE',  ( -54.42813229853333468, -297.7662352645559167, -345.3683826091709648 ) ) ;
#32199 = EDGE_LOOP ( 'NONE', ( #46513, #64743, #59187, #43388 ) ) ;
#32200 = ORIENTED_EDGE ( 'NONE', *, *, #55616, .T. ) ;
#32201 = DIRECTION ( 'NONE',  ( 0.000000000000000000, 0.000000000000000000, 1.000000000000000000 ) ) ;
#32202 = CARTESIAN_POINT ( 'NONE',  ( -99.09477969312752066, -291.0876510141624181, -309.8678672499180493 ) ) ;
#32203 = CARTESIAN_POINT ( 'NONE',  ( -40.27687523391615798, -290.8486774883558610, -346.3039873528174439 ) ) ;
#32204 = CARTESIAN_POINT ( 'NONE',  ( -110.0734738020615140, -289.9975223248215457, -263.0138895065859401 ) ) ;
#32205 = CARTESIAN_POINT ( 'NONE',  ( -80.89819907993499726, -284.9861552802685765, -206.8747494338723527 ) ) ;
#32206 = CARTESIAN_POINT ( 'NONE',  ( 150.4957602436334412, 21.00000000000000000, -3.637614988394445081 ) ) ;
#32207 = CARTESIAN_POINT ( 'NONE',  ( -2.063978847144392947, -280.9767570088134221, -335.1978020052873717 ) ) ;
#32208 = CARTESIAN_POINT ( 'NONE',  ( 36.50067403360087326, -289.3136365659321996, -262.7342406910485693 ) ) ;
#32209 = CARTESIAN_POINT ( 'NONE',  ( -21.25554649829815546, -281.3220712254017712, -342.3298469887318447 ) ) ;
#32210 = EDGE_CURVE ( 'NONE', #45666, #67402, #3664, .T. ) ;
#32211 = CARTESIAN_POINT ( 'NONE',  ( 32.43959880854713163, -282.5613434196513367, -247.1397469063622623 ) ) ;
#32212 = CARTESIAN_POINT ( 'NONE',  ( 37.88013025497256336, -288.6855003090064429, -285.6743948231272725 ) ) ;
#32213 = CARTESIAN_POINT ( 'NONE',  ( -94.84317303782539454, -279.6796644029840877, -225.2680486695198852 ) ) ;
#32214 = CARTESIAN_POINT ( 'NONE',  ( -96.26356086346071095, -290.0089469606664920, -221.3896212359633182 ) ) ;
#32215 = CARTESIAN_POINT ( 'NONE',  ( -111.7160819607365738, -285.1122859357790276, -289.7163666339131964 ) ) ;
#32216 = CARTESIAN_POINT ( 'NONE',  ( -2.256567359835757181, -286.9962189965971220, -201.8733146190533034 ) ) ;
#32217 = CARTESIAN_POINT ( 'NONE',  ( -86.92728023471225640, -283.9318838215097003, -324.0051758269629545 ) ) ;
#32218 = ORIENTED_EDGE ( 'NONE', *, *, #58549, .F. ) ;
#32219 = CARTESIAN_POINT ( 'NONE',  ( 41.08708295871279859, -293.9068999365417199, -472.6442049081569508 ) ) ;
#32220 = CARTESIAN_POINT ( 'NONE',  ( -25.24241823611405877, -294.0652479960531309, -195.5686527472780085 ) ) ;
#32221 = CARTESIAN_POINT ( 'NONE',  ( 34.99188720886146342, -291.9189866085632161, -245.2777599125674044 ) ) ;
#32222 = CARTESIAN_POINT ( 'NONE',  ( 32.31830253633833649, -274.9098179559817368, -292.9640486980184164 ) ) ;
#32223 = CARTESIAN_POINT ( 'NONE',  ( -32.02784585440693377, -294.3353892984665663, -347.0886022834904452 ) ) ;
#32224 = CARTESIAN_POINT ( 'NONE',  ( -109.3843267870809228, -289.2347090133541769, -254.8508730272920388 ) ) ;
#32225 = CARTESIAN_POINT ( 'NONE',  ( 19.59851942928052537, -292.4535114628120027, -317.6452105804276016 ) ) ;
#32226 = VECTOR ( 'NONE', #87542, 1000.000000000000000 ) ;
#32227 = CARTESIAN_POINT ( 'NONE',  ( -44.35333418936818362, -293.1667142387942704, -197.2486277647709016 ) ) ;
#32228 = CARTESIAN_POINT ( 'NONE',  ( 208.1597743490453638, 35.80769208713102358, 15.05537761763264371 ) ) ;
#32229 = VECTOR ( 'NONE', #14206, 1000.000000000000000 ) ;
#32230 = CARTESIAN_POINT ( 'NONE',  ( 36.79377204633100007, -291.7119545663063036, -282.8470202735847465 ) ) ;
#32231 = CARTESIAN_POINT ( 'NONE',  ( 36.17919655412337221, -295.7434367353993707, -285.2464710003911819 ) ) ;
#32232 = CARTESIAN_POINT ( 'NONE',  ( 35.35923419026552494, -288.6095270909180499, -279.1918935565688002 ) ) ;
#32233 = CARTESIAN_POINT ( 'NONE',  ( -70.81702276271015251, -279.4714406329405278, -337.8726694500839471 ) ) ;
#32234 = CARTESIAN_POINT ( 'NONE',  ( -14.72166629277199945, -275.5604466277056872, -343.6036917696333148 ) ) ;
#32235 = CARTESIAN_POINT ( 'NONE',  ( -34.04527844338633003, -297.2896107109601189, -193.5230290258803620 ) ) ;
#32236 = CARTESIAN_POINT ( 'NONE',  ( -65.33540394513283900, -277.7632060720709433, -201.3852762297734387 ) ) ;
#32237 = CARTESIAN_POINT ( 'NONE',  ( -92.76626186915059691, -276.2298706324993418, -322.7298619205337218 ) ) ;
#32238 = AXIS2_PLACEMENT_3D ( 'NONE', #52924, #75645, #38717 ) ;
#32239 = CARTESIAN_POINT ( 'NONE',  ( -78.23797558997959811, -294.2994180815049958, -331.4859898249936236 ) ) ;
#32240 = CARTESIAN_POINT ( 'NONE',  ( -58.16716152484593749, -275.7833505258702189, -198.2569754551813901 ) ) ;
#32241 = CARTESIAN_POINT ( 'NONE',  ( -54.24314367885441612, -274.4806985650496358, -199.2398562268362241 ) ) ;
#32242 = CARTESIAN_POINT ( 'NONE',  ( 196.0517256323039135, 25.50333437355849142, 11.93519303445567736 ) ) ;
#32244 = CARTESIAN_POINT ( 'NONE',  ( -65.81118855939183732, -273.5023600684870075, -203.1414167560695319 ) ) ;
#32243 = CARTESIAN_POINT ( 'NONE',  ( -6.326998723337653452, -286.6668614897027965, -339.0378615201952925 ) ) ;
#32245 = CIRCLE ( 'NONE', #15627, 0.5000000000000000000 ) ;
#32246 = CARTESIAN_POINT ( 'NONE',  ( 36.38539468981196023, -287.8314402785017023, -292.6176190156853067 ) ) ;
#32247 = CARTESIAN_POINT ( 'NONE',  ( -34.15967351294457899, -300.0716840673962338, -195.0048420694594711 ) ) ;
#32248 = CARTESIAN_POINT ( 'NONE',  ( -106.4456722396703725, -294.9276701827540137, -241.6440592496219608 ) ) ;
#32249 = CARTESIAN_POINT ( 'NONE',  ( -38.73988127609003840, -282.2664427798089832, -347.1869203580518501 ) ) ;
#32250 = CARTESIAN_POINT ( 'NONE',  ( 155.2961426000043730, 19.82592759221628498, 13.64628225442075937 ) ) ;
#32251 = CARTESIAN_POINT ( 'NONE',  ( -111.3836069725953024, -276.3945524031435070, -282.6228425162307758 ) ) ;
#32252 = VECTOR ( 'NONE', #73854, 1000.000000000000000 ) ;
#32253 = DIRECTION ( 'NONE',  ( -0.9531768234071978929, 0.3024135303179465439, 0.000000000000000000 ) ) ;
#32254 = CARTESIAN_POINT ( 'NONE',  ( -101.4631401186011459, -289.8340395935156266, -234.5416235684411106 ) ) ;
#32255 = FACE_OUTER_BOUND ( 'NONE', #54741, .T. ) ;
#32256 = FACE_OUTER_BOUND ( 'NONE', #46606, .T. ) ;
#32257 = CARTESIAN_POINT ( 'NONE',  ( -73.57132889767861172, -289.5716214838470819, -204.6337891756796523 ) ) ;
#32258 = CARTESIAN_POINT ( 'NONE',  ( 7.739928421113376089, -276.2007600089746120, -212.0657106346083083 ) ) ;
#32259 = CARTESIAN_POINT ( 'NONE',  ( 37.29393907335293079, -283.1845464576910558, -286.7962111365069973 ) ) ;
#32261 = CARTESIAN_POINT ( 'NONE',  ( -32.14570100355977189, -282.9847833372272135, -343.1759625755273078 ) ) ;
#32260 = CARTESIAN_POINT ( 'NONE',  ( 95.58944840416511113, -297.7283352241495891, -195.0504912288055550 ) ) ;
#32262 = CARTESIAN_POINT ( 'NONE',  ( -27.22700639542446055, -275.6083583574713884, -197.4190153406925958 ) ) ;
#32263 = CARTESIAN_POINT ( 'NONE',  ( 35.26764813401671717, -276.4783980577627176, -279.7369091912106001 ) ) ;
#32264 = CARTESIAN_POINT ( 'NONE',  ( 26.61322196549786412, -284.0789346999468421, -309.6357126892287965 ) ) ;
#32265 = ORIENTED_EDGE ( 'NONE', *, *, #26684, .T. ) ;
#32266 = CARTESIAN_POINT ( 'NONE',  ( 189.9243309297870610, 215.0000000000000568, 20.22542485937349355 ) ) ;
#32267 = CARTESIAN_POINT ( 'NONE',  ( 34.45072584340250188, -293.7381287420843705, -298.1972020753325410 ) ) ;
#32268 = CARTESIAN_POINT ( 'NONE',  ( -70.74050075527206616, -287.5893880694603126, -203.5908323389459156 ) ) ;
#32269 = DIRECTION ( 'NONE',  ( 1.000000000000000000, 0.000000000000000000, 0.000000000000000000 ) ) ;
#32270 = CARTESIAN_POINT ( 'NONE',  ( -72.02372285203398405, -283.1237833571631768, -198.2697987213421698 ) ) ;
#32271 = CARTESIAN_POINT ( 'NONE',  ( -110.5160414611179505, -277.4519852121095482, -293.9776425699749325 ) ) ;
#32272 = CARTESIAN_POINT ( 'NONE',  ( -110.0250025524820785, -288.6594980502424619, -293.4154749958042885 ) ) ;
#32273 = CARTESIAN_POINT ( 'NONE',  ( -72.72374852345218699, -287.0947370963862681, -205.7029838738236265 ) ) ;
#32274 = CARTESIAN_POINT ( 'NONE',  ( 6.008198648516186680, -278.2156342905747124, -330.4140878174021054 ) ) ;
#32275 = CARTESIAN_POINT ( 'NONE',  ( -32.36307777113534456, -287.5390106590699588, -194.0996451132782283 ) ) ;
#32276 = CARTESIAN_POINT ( 'NONE',  ( 23.44754035571330775, -284.1506537678160953, -314.3111134739431236 ) ) ;
#32277 = CARTESIAN_POINT ( 'NONE',  ( -14.58766863316399309, -276.9319815117594317, -343.9781706223171796 ) ) ;
#32278 = CARTESIAN_POINT ( 'NONE',  ( -102.0981396277692852, -277.8377682362244059, -312.1189909655019505 ) ) ;
#32280 = CARTESIAN_POINT ( 'NONE',  ( -107.1648759016839847, -298.8115035065173970, -244.4045847718304572 ) ) ;
#32279 = AXIS2_PLACEMENT_3D ( 'NONE', #74155, #31544, #58578 ) ;
#32281 = CARTESIAN_POINT ( 'NONE',  ( 156.4869342561325993, 15.84738232520213863, 9.998183562658692125 ) ) ;
#32282 = CARTESIAN_POINT ( 'NONE',  ( -112.3452863284742875, -275.1604526064900824, -261.9424758988611188 ) ) ;
#32283 = CARTESIAN_POINT ( 'NONE',  ( -36.88194192547111072, -296.1974401242884483, -194.5964544069025806 ) ) ;
#32285 = AXIS2_PLACEMENT_3D ( 'NONE', #22689, #51562, #80450 ) ;
#32284 = DIRECTION ( 'NONE',  ( 0.000000000000000000, 0.000000000000000000, -1.000000000000000000 ) ) ;
#32286 = CARTESIAN_POINT ( 'NONE',  ( -89.13386536462138565, -277.3122977515685648, -321.9650924524983111 ) ) ;
#32287 = AXIS2_PLACEMENT_3D ( 'NONE', #32110, #75657, #54341 ) ;
#32288 = CARTESIAN_POINT ( 'NONE',  ( -69.97662454651160147, -274.8369238568205901, -201.0433116877852626 ) ) ;
#32289 = CARTESIAN_POINT ( 'NONE',  ( 38.63666777377471817, -280.7483853767105870, -281.3204894922679387 ) ) ;
#32290 = CARTESIAN_POINT ( 'NONE',  ( 36.28010480961432904, -289.2133780135225720, -262.7582336555315692 ) ) ;
#32291 = CARTESIAN_POINT ( 'NONE',  ( -112.2122030526331287, -298.2590715771484042, -255.5589953414583704 ) ) ;
#32292 = CARTESIAN_POINT ( 'NONE',  ( -44.74191011189814304, -296.3487757258884017, -346.6588917906612437 ) ) ;
#32293 = CARTESIAN_POINT ( 'NONE',  ( 9.989181565077073444, -294.7057653998595015, -212.3300037107543972 ) ) ;
#32294 = CARTESIAN_POINT ( 'NONE',  ( -38.35368219736916728, -278.0392828269668257, -195.5219115804316061 ) ) ;
#32295 = VECTOR ( 'NONE', #13067, 1000.000000000000000 ) ;
#32296 = CARTESIAN_POINT ( 'NONE',  ( 33.33626291598083213, -283.1662259193070099, -246.8334676036583915 ) ) ;
#32297 = CARTESIAN_POINT ( 'NONE',  ( -37.80746338938782714, -296.1261205785993980, -195.9225710704702124 ) ) ;
#32298 = CARTESIAN_POINT ( 'NONE',  ( -110.3357146914367490, -285.8744170749661748, -292.2767830340557680 ) ) ;
#32299 = CARTESIAN_POINT ( 'NONE',  ( -4.443570321141995016, -285.4166419349108992, -204.8482251309627031 ) ) ;
#32300 = CARTESIAN_POINT ( 'NONE',  ( -82.07967447956953322, -220.3963648522054370, -351.9527955420491594 ) ) ;
#32301 = ORIENTED_EDGE ( 'NONE', *, *, #46824, .F. ) ;
#32302 = EDGE_CURVE ( 'NONE', #27101, #10184, #12926, .T. ) ;
#32303 = CARTESIAN_POINT ( 'NONE',  ( 33.41010517135428159, -286.9799189786174338, -252.2477048155458021 ) ) ;
#32304 = ORIENTED_EDGE ( 'NONE', *, *, #8766, .T. ) ;
#32305 = CARTESIAN_POINT ( 'NONE',  ( -92.20297315227257684, -284.8937206349091866, -323.9496730260005961 ) ) ;
#32306 = CIRCLE ( 'NONE', #85236, 0.9999999999999977796 ) ;
#32307 = CARTESIAN_POINT ( 'NONE',  ( 0.6198357200240276477, -274.9067993234393157, -207.9831628796951861 ) ) ;
#32308 = CARTESIAN_POINT ( 'NONE',  ( 34.48725945327707620, -286.0087922681374835, -243.7414019185382585 ) ) ;
#32309 = CONICAL_SURFACE ( 'NONE', #41410, 6.249455242036738412, 0.09862129276975223346 ) ;
#32310 = CARTESIAN_POINT ( 'NONE',  ( -44.85303184136727594, -290.8796471091947637, -193.9862463122042016 ) ) ;
#32311 = ADVANCED_FACE ( 'NONE', ( #20487 ), #30366, .F. ) ;
#32312 = CARTESIAN_POINT ( 'NONE',  ( 200.2296996224750103, 68.12454877777268791, 0.000000000000000000 ) ) ;
#32313 = CARTESIAN_POINT ( 'NONE',  ( -97.16550227132226780, -280.7118629999972654, -222.9921360119068368 ) ) ;
#32314 = CARTESIAN_POINT ( 'NONE',  ( 34.56926708955342775, -282.2332892996662963, -297.8303204697812134 ) ) ;
#32315 = CARTESIAN_POINT ( 'NONE',  ( -21.33282851196157992, -277.7666405000204577, -200.3683826091710216 ) ) ;
#32316 = CARTESIAN_POINT ( 'NONE',  ( -99.42433144932330435, -248.5360940272530001, -334.3804182888130754 ) ) ;
#32317 = ORIENTED_EDGE ( 'NONE', *, *, #86489, .F. ) ;
#32318 = CARTESIAN_POINT ( 'NONE',  ( 36.16979982627429280, -277.3721129016309419, -256.3579824915490804 ) ) ;
#32319 = CARTESIAN_POINT ( 'NONE',  ( 173.1255004754493712, 243.5021256030123027, -179.3842541629520611 ) ) ;
#32320 = TOROIDAL_SURFACE ( 'NONE', #20229, 24.00000000000002132, 2.046895004029262388 ) ;
#32321 = CARTESIAN_POINT ( 'NONE',  ( 14.49507151843468300, -278.8053531906564331, -216.5787671083034240 ) ) ;
#32322 = CARTESIAN_POINT ( 'NONE',  ( -70.34718550594215003, -297.2412399472815423, -338.8196606254690550 ) ) ;
#32323 = CARTESIAN_POINT ( 'NONE',  ( -88.19069716722290764, -296.6661121821695133, -217.7711979766835384 ) ) ;
#32324 = CARTESIAN_POINT ( 'NONE',  ( -25.02510931891547230, -291.7128637054604496, -194.4148969184278712 ) ) ;
#32325 = DIRECTION ( 'NONE',  ( -0.8571673007021122226, 1.049727191138618696E-16, 0.5150380749100541555 ) ) ;
#32327 = CARTESIAN_POINT ( 'NONE',  ( 15.61761637174408079, -285.2169997241592796, -218.9631490465316119 ) ) ;
#32326 = CARTESIAN_POINT ( 'NONE',  ( -113.6465790904518229, -295.0648493868808373, -275.2831899912055178 ) ) ;
#32328 = CARTESIAN_POINT ( 'NONE',  ( 23.96626899298357571, -295.9863589187013986, -312.3103182508652935 ) ) ;
#32329 = CARTESIAN_POINT ( 'NONE',  ( 18.13753566622487057, -288.1847579160051396, -222.1605176268522257 ) ) ;
#32330 = ORIENTED_EDGE ( 'NONE', *, *, #49257, .F. ) ;
#32331 = CARTESIAN_POINT ( 'NONE',  ( 34.23643443135534170, -294.8458823230296844, -298.0990138190774132 ) ) ;
#32332 = CARTESIAN_POINT ( 'NONE',  ( -109.9331421419225308, -284.9296889926879999, -279.0719114223929864 ) ) ;
#32333 = CARTESIAN_POINT ( 'NONE',  ( -39.11411323897724657, -293.8688619392580108, -346.9435394099575660 ) ) ;
#32334 = CIRCLE ( 'NONE', #5102, 2.000000000000001776 ) ;
#32335 = CARTESIAN_POINT ( 'NONE',  ( -92.70285612861634661, -292.0866334253823311, -217.0003165465266477 ) ) ;
#32336 = CARTESIAN_POINT ( 'NONE',  ( -79.56588751481959321, -291.9908621514224478, -205.9806751378311560 ) ) ;
#32337 = CARTESIAN_POINT ( 'NONE',  ( -29.17101451503082998, -289.1124041353048710, -342.9024158832058333 ) ) ;
#32338 = EDGE_LOOP ( 'NONE', ( #86764, #16134, #22665, #92379 ) ) ;
#32339 = LINE ( 'NONE', #61240, #86626 ) ;
#32340 = CARTESIAN_POINT ( 'NONE',  ( -111.6566287797313066, -274.6499668381442234, -256.4209244867586790 ) ) ;
#32341 = CARTESIAN_POINT ( 'NONE',  ( -108.7906646557815122, -271.7004588130334923, -242.5917494710402309 ) ) ;
#32342 = EDGE_CURVE ( 'NONE', #66900, #61882, #20903, .T. ) ;
#32343 = CARTESIAN_POINT ( 'NONE',  ( 35.66252737393860173, -280.6953467798653037, -276.7836653902211879 ) ) ;
#32344 = VERTEX_POINT ( 'NONE', #73466 ) ;
#32345 = ORIENTED_EDGE ( 'NONE', *, *, #26014, .T. ) ;
#32346 = CARTESIAN_POINT ( 'NONE',  ( 38.43259605435577697, -274.8919769162088187, -256.9522760687449363 ) ) ;
#32347 = CARTESIAN_POINT ( 'NONE',  ( -108.5001396552410284, -295.2833197611125797, -251.1504883938874855 ) ) ;
#32348 = CARTESIAN_POINT ( 'NONE',  ( -73.42196341943370896, -279.3965083370046614, -335.2531643537352011 ) ) ;
#32349 = CARTESIAN_POINT ( 'NONE',  ( 31.32626742168720568, -273.3184131282981753, -242.0200803012417055 ) ) ;
#32350 = CARTESIAN_POINT ( 'NONE',  ( -109.1708914671404216, -297.9559892846735352, -255.2109676722522522 ) ) ;
#32351 = CARTESIAN_POINT ( 'NONE',  ( -75.38275588740876287, -298.6120167188104233, -207.6356462301342276 ) ) ;
#32352 = CARTESIAN_POINT ( 'NONE',  ( -59.93058115945312636, -299.3644882323160914, -197.5312893871767983 ) ) ;
#32353 = CARTESIAN_POINT ( 'NONE',  ( -27.19254136597337279, -272.2005099159476345, -195.6402176614799941 ) ) ;
#32354 = CARTESIAN_POINT ( 'NONE',  ( 35.74420764866165001, -294.2447221213153625, -273.4850649989338649 ) ) ;
#32355 = CARTESIAN_POINT ( 'NONE',  ( -3.348062670835536991, -291.0850095665383037, -205.0939169477127848 ) ) ;
#32356 = CARTESIAN_POINT ( 'NONE',  ( 196.0143093133015384, 19.33012701892218743, 12.49999999999999112 ) ) ;
#32357 = CARTESIAN_POINT ( 'NONE',  ( 39.25541075472718688, -275.9471107175803581, -262.5803281006356542 ) ) ;
#32358 = CARTESIAN_POINT ( 'NONE',  ( -102.0314305036114177, -273.1804833387137705, -236.4250285445152713 ) ) ;
#32359 = CARTESIAN_POINT ( 'NONE',  ( 36.26447050974762476, -283.7390765580696552, -286.5620009352759894 ) ) ;
#32360 = CARTESIAN_POINT ( 'NONE',  ( -65.08904940218464219, -282.0920310978439147, -341.6730784576504902 ) ) ;
#32361 = DIRECTION ( 'NONE',  ( -0.000000000000000000, 1.000000000000000000, -0.000000000000000000 ) ) ;
#32362 = CARTESIAN_POINT ( 'NONE',  ( -82.90325194787516239, -282.8907312274963601, -327.6690081599109021 ) ) ;
#32363 = CARTESIAN_POINT ( 'NONE',  ( -93.05776711153009728, -281.8497423675445361, -320.8356247917740802 ) ) ;
#32364 = CARTESIAN_POINT ( 'NONE',  ( 29.68352570831852333, -274.5330799555257499, -300.7419345787084808 ) ) ;
#32365 = CARTESIAN_POINT ( 'NONE',  ( -32.04088924950214334, -282.1190584623532800, -195.4975217166891355 ) ) ;
#32366 = CARTESIAN_POINT ( 'NONE',  ( 154.9842916688209868, 275.0000000000000568, -12.88888888888890705 ) ) ;
#32367 = DIRECTION ( 'NONE',  ( 0.000000000000000000, 1.000000000000000000, 0.000000000000000000 ) ) ;
#32368 = CARTESIAN_POINT ( 'NONE',  ( -5.430534733744966758, -272.8648975631196549, -201.1648901865350183 ) ) ;
#32369 = AXIS2_PLACEMENT_3D ( 'NONE', #61812, #11611, #75086 ) ;
#32370 = CARTESIAN_POINT ( 'NONE',  ( -106.9488764411532600, -280.1831986199911171, -298.7313388095516302 ) ) ;
#32371 = CYLINDRICAL_SURFACE ( 'NONE', #12027, 5.000000000000000888 ) ;
#32372 = CARTESIAN_POINT ( 'NONE',  ( -109.5571685140269551, -286.7588443331821395, -247.9533079844526640 ) ) ;
#32373 = AXIS2_PLACEMENT_3D ( 'NONE', #65834, #22692, #58702 ) ;
#32374 = CARTESIAN_POINT ( 'NONE',  ( 208.5338978937603258, 38.36651302259750196, 14.22786471510243089 ) ) ;
#32375 = CARTESIAN_POINT ( 'NONE',  ( -69.34226144694790150, -289.6310272311670815, -202.5168244816508150 ) ) ;
#32376 = CARTESIAN_POINT ( 'NONE',  ( 139.6925840978351516, -141.7221692137691775, 21.50000000000000000 ) ) ;
#32377 = CARTESIAN_POINT ( 'NONE',  ( -108.2150961877190838, -295.5983150738486529, -251.2315247105417200 ) ) ;
#32378 = CARTESIAN_POINT ( 'NONE',  ( -91.51002333266008293, -287.9728055004209750, -321.1970073512915747 ) ) ;
#32379 = FACE_OUTER_BOUND ( 'NONE', #13467, .T. ) ;
#32380 = CARTESIAN_POINT ( 'NONE',  ( -111.1138956086464020, -294.3775424377677723, -283.9477102097837928 ) ) ;
#32381 = CARTESIAN_POINT ( 'NONE',  ( 11.64741596629121823, -285.1973680554068551, -211.7876736251588738 ) ) ;
#32382 = CARTESIAN_POINT ( 'NONE',  ( 27.56825487165307820, -283.6262049400421006, -305.4771848922749200 ) ) ;
#32383 = CARTESIAN_POINT ( 'NONE',  ( 6.324130911590088111, -280.7083881226946005, -332.6128191718094058 ) ) ;
#32384 = CARTESIAN_POINT ( 'NONE',  ( -13.28787469182305792, -288.7308308813364874, -339.2843613905860707 ) ) ;
#32385 = AXIS2_PLACEMENT_3D ( 'NONE', #74700, #67137, #2271 ) ;
#32386 = CARTESIAN_POINT ( 'NONE',  ( 32.53038872741445431, -282.6714239488571820, -247.1080796639563744 ) ) ;
#32387 = CARTESIAN_POINT ( 'NONE',  ( -34.31686453079056776, -280.8939502873100196, -197.2496267091526363 ) ) ;
#32388 = CARTESIAN_POINT ( 'NONE',  ( 33.30329505202329443, -289.1932470475849186, -244.1372460893867071 ) ) ;
#32389 = CARTESIAN_POINT ( 'NONE',  ( -85.21807702622959368, -297.5780897807170504, -210.0547954318478503 ) ) ;
#32390 = ORIENTED_EDGE ( 'NONE', *, *, #91063, .F. ) ;
#32391 = AXIS2_PLACEMENT_3D ( 'NONE', #6752, #66365, #86250 ) ;
#32392 = CARTESIAN_POINT ( 'NONE',  ( -32.68260308280422066, -274.1093157272443932, -193.4890523665611113 ) ) ;
#32393 = CARTESIAN_POINT ( 'NONE',  ( -9.128663604227064354, -294.4026341400522142, -201.1984510684911527 ) ) ;
#32394 = DIRECTION ( 'NONE',  ( 0.000000000000000000, -1.000000000000000000, 0.000000000000000000 ) ) ;
#32395 = CARTESIAN_POINT ( 'NONE',  ( -4.771743288812468897, -279.1233781216988064, -337.9199732462171255 ) ) ;
#32396 = ORIENTED_EDGE ( 'NONE', *, *, #16325, .T. ) ;
#32397 = CARTESIAN_POINT ( 'NONE',  ( -34.38922664861754441, -275.0149512517467656, -345.4697814598350192 ) ) ;
#32398 = CARTESIAN_POINT ( 'NONE',  ( 189.9243309297870610, 276.0000000000000568, 20.22542485937349355 ) ) ;
#32399 = CARTESIAN_POINT ( 'NONE',  ( -96.71010705810103047, -295.5989722807323687, -222.5925856902501039 ) ) ;
#32400 = CARTESIAN_POINT ( 'NONE',  ( -76.61200643603298488, -272.8598460136507242, -208.7029010885975993 ) ) ;
#32401 = CARTESIAN_POINT ( 'NONE',  ( -95.67497020326675283, -292.7002995774033138, -225.3284925121474771 ) ) ;
#32402 = AXIS2_PLACEMENT_3D ( 'NONE', #68978, #32980, #90702 ) ;
#32403 = CARTESIAN_POINT ( 'NONE',  ( -34.78945241426409751, -284.7798300885380627, -344.3430452014534922 ) ) ;
#32404 = CARTESIAN_POINT ( 'NONE',  ( -97.89255279504368445, -292.6043255270955115, -223.7330670399650501 ) ) ;
#32405 = CARTESIAN_POINT ( 'NONE',  ( 1.435608388423053272, -293.8737294512537801, -204.3489427776735852 ) ) ;
#32406 = CARTESIAN_POINT ( 'NONE',  ( 35.70797416219151899, -293.3907598458124539, -270.7620413100024734 ) ) ;
#32407 = CARTESIAN_POINT ( 'NONE',  ( 21.90533250431893819, -288.9218133125194186, -224.3742744604433597 ) ) ;
#32408 = CARTESIAN_POINT ( 'NONE',  ( 21.96934963379798589, -281.0587317681415129, -221.2571529626713414 ) ) ;
#32409 = CARTESIAN_POINT ( 'NONE',  ( -95.42056359907546437, -293.9693401420921646, -318.7150820059781609 ) ) ;
#32410 = CARTESIAN_POINT ( 'NONE',  ( -47.25846401018586818, -283.0081704693097890, -346.7198620699309117 ) ) ;
#32411 = CARTESIAN_POINT ( 'NONE',  ( 31.81112822514513994, -277.9017789624232364, -298.6009576284413924 ) ) ;
#32412 = CARTESIAN_POINT ( 'NONE',  ( -53.88499642491207453, -275.4017514920610097, -344.3515122700736129 ) ) ;
#32413 = CARTESIAN_POINT ( 'NONE',  ( 208.4306832106271088, -44.55766379199612004, 0.000000000000000000 ) ) ;
#32414 = CARTESIAN_POINT ( 'NONE',  ( -93.47337082312604650, -283.3967610902026877, -317.1288845192268013 ) ) ;
#32415 = CARTESIAN_POINT ( 'NONE',  ( -74.82709311628362059, -280.7695548127976508, -203.5565220971852796 ) ) ;
#32416 = CARTESIAN_POINT ( 'NONE',  ( 24.52078660090812434, -286.0053344338332977, -224.9094629061029593 ) ) ;
#32417 = CARTESIAN_POINT ( 'NONE',  ( -9.364938622540815771, -294.1829186509569354, -201.7845193528349910 ) ) ;
#32418 = CARTESIAN_POINT ( 'NONE',  ( 27.80787594902894355, -276.6297915557126430, -230.7384826736917773 ) ) ;
#32419 = CARTESIAN_POINT ( 'NONE',  ( 36.02534764677034218, -277.1417454587772227, -292.1001054445010823 ) ) ;
#32420 = CARTESIAN_POINT ( 'NONE',  ( -108.7652147455494003, -278.1864210546953586, -285.4502387065083440 ) ) ;
#32421 = CARTESIAN_POINT ( 'NONE',  ( -44.77594189955190274, -299.9581344516384434, -195.8463219659928427 ) ) ;
#32422 = CARTESIAN_POINT ( 'NONE',  ( -65.76657831342915017, -283.6794743276750523, -201.0813000019735739 ) ) ;
#32423 = CARTESIAN_POINT ( 'NONE',  ( -44.89074754434063408, -291.6259169909620255, -193.7004026931768692 ) ) ;
#32424 = CARTESIAN_POINT ( 'NONE',  ( -74.02413100341306063, -291.1311924263224000, -337.1655309676206116 ) ) ;
#32425 = CARTESIAN_POINT ( 'NONE',  ( -41.59709081642525774, -290.9177642364082885, -197.1255578693039752 ) ) ;
#32426 = ORIENTED_EDGE ( 'NONE', *, *, #1240, .T. ) ;
#32427 = CARTESIAN_POINT ( 'NONE',  ( -4.838180963169321558, -291.0466057699269413, -201.2081893590344635 ) ) ;
#32428 = CARTESIAN_POINT ( 'NONE',  ( -7.257658260007986861, -292.1246974259365174, -203.8251283849321851 ) ) ;
#32429 = ORIENTED_EDGE ( 'NONE', *, *, #6382, .T. ) ;
#32430 = CARTESIAN_POINT ( 'NONE',  ( -41.72907601921568244, -290.1858438987486011, -346.9395758839061727 ) ) ;
#32431 = CARTESIAN_POINT ( 'NONE',  ( -85.55762702215886861, -280.0154206062724143, -215.4146252681086366 ) ) ;
#32432 = CARTESIAN_POINT ( 'NONE',  ( -113.2937005686993501, -295.6070294040862905, -259.6461614683297512 ) ) ;
#32433 = CARTESIAN_POINT ( 'NONE',  ( 1.463067592329282629, -287.2078707335562626, -203.9567746776621391 ) ) ;
#32434 = EDGE_CURVE ( 'NONE', #43263, #8225, #79181, .T. ) ;
#32435 = CARTESIAN_POINT ( 'NONE',  ( 1.507341928917059759, -286.8897900295468162, -203.8890598430689636 ) ) ;
#32436 = CARTESIAN_POINT ( 'NONE',  ( -76.13476189213297118, -283.9191052613003308, -332.2851683735178767 ) ) ;
#32437 = CARTESIAN_POINT ( 'NONE',  ( 173.7950248217412081, 243.4804843829244589, -179.6775006142443374 ) ) ;
#32438 = CARTESIAN_POINT ( 'NONE',  ( 23.88957826587596855, -22.54207381367533714, -343.5632202908770978 ) ) ;
#32439 = CARTESIAN_POINT ( 'NONE',  ( -55.84047289447126872, -169.3153992383580260, -360.5835854410441925 ) ) ;
#32440 = CARTESIAN_POINT ( 'NONE',  ( -71.73912590187161697, -276.7161221966420044, -334.9462867330391873 ) ) ;
#32441 = CARTESIAN_POINT ( 'NONE',  ( 35.32873332832064506, -274.3456371679985182, -260.7053334545656185 ) ) ;
#32442 = CARTESIAN_POINT ( 'NONE',  ( -82.92906580391864679, -296.9550300905445397, -208.3165517894283028 ) ) ;
#32443 = CARTESIAN_POINT ( 'NONE',  ( 202.5199829828008546, 289.9242760918802446, -82.50643157239619541 ) ) ;
#32444 = CARTESIAN_POINT ( 'NONE',  ( -97.55124454307568271, -276.6019314941992207, -317.5639678570206570 ) ) ;
#32445 = CARTESIAN_POINT ( 'NONE',  ( -97.11280006326180114, -274.9161399701190476, -226.6251671795039897 ) ) ;
#32446 = CARTESIAN_POINT ( 'NONE',  ( -110.3674973873447982, -290.9976182341925437, -273.9181996503078267 ) ) ;
#32447 = CARTESIAN_POINT ( 'NONE',  ( -99.79627983481546494, -297.9493676950479539, -225.5997027414165927 ) ) ;
#32448 = CARTESIAN_POINT ( 'NONE',  ( -105.2022907227369899, -297.5146665670653192, -233.9925021789906623 ) ) ;
#32449 = CARTESIAN_POINT ( 'NONE',  ( -70.92890994336237043, -295.6748925296958532, -335.1894473489932693 ) ) ;
#32450 = EDGE_LOOP ( 'NONE', ( #76571, #82977 ) ) ;
#32451 = TOROIDAL_SURFACE ( 'NONE', #43000, 1.000000000000000000, 0.5000000000000000000 ) ;
#32452 = CARTESIAN_POINT ( 'NONE',  ( -72.15505482187559494, -279.4290425871595289, -337.4377885480166697 ) ) ;
#32453 = EDGE_CURVE ( 'NONE', #82273, #30954, #37456, .T. ) ;
#32454 = ADVANCED_FACE ( 'NONE', ( #50757, #71618 ), #14326, .T. ) ;
#32455 = CARTESIAN_POINT ( 'NONE',  ( 22.47146288680990267, -281.7094525246209855, -318.7752120679950281 ) ) ;
#32456 = CARTESIAN_POINT ( 'NONE',  ( -94.62961870973823864, -278.8509340769741129, -316.0046354399279949 ) ) ;
#32457 = CARTESIAN_POINT ( 'NONE',  ( 37.19283742599328235, -277.4996523657072203, -285.1454586091329020 ) ) ;
#32458 = CARTESIAN_POINT ( 'NONE',  ( -105.0087371295930438, -271.4220887925192756, -241.0448966601455822 ) ) ;
#32459 = CARTESIAN_POINT ( 'NONE',  ( 150.7067237504873845, 20.03350844490827853, -5.072059973232346586 ) ) ;
#32460 = CARTESIAN_POINT ( 'NONE',  ( -109.9037758266207447, -278.6076168075037458, -278.7919245255241094 ) ) ;
#32461 = CARTESIAN_POINT ( 'NONE',  ( -92.06125906436095363, -274.0974753519782325, -216.4173631066185521 ) ) ;
#32462 = CIRCLE ( 'NONE', #64282, 4.999999999999990230 ) ;
#32463 = CARTESIAN_POINT ( 'NONE',  ( 38.85478441651682147, -286.3236334001359751, -277.2454490988039879 ) ) ;
#32464 = CARTESIAN_POINT ( 'NONE',  ( -64.20806928646177880, -275.7018206846278190, -200.3244534211798111 ) ) ;
#32465 = CARTESIAN_POINT ( 'NONE',  ( 38.34306530093780907, -273.9944500992896224, -259.8529033564357746 ) ) ;
#32466 = FACE_OUTER_BOUND ( 'NONE', #69684, .T. ) ;
#32467 = CARTESIAN_POINT ( 'NONE',  ( -101.7902247573781835, -289.2768991933272673, -305.0949833633569028 ) ) ;
#32468 = ADVANCED_FACE ( 'NONE', ( #8123 ), #22333, .T. ) ;
#32469 = CARTESIAN_POINT ( 'NONE',  ( -101.3389253635708940, -283.3377889204409712, -313.0907938094499627 ) ) ;
#32470 = CARTESIAN_POINT ( 'NONE',  ( 35.33347399751815487, -279.6088476364748203, -256.2837836662665154 ) ) ;
#32471 = B_SPLINE_CURVE_WITH_KNOTS ( 'NONE', 3,
 ( #62777, #89728, #62282, #55183 ),
 .UNSPECIFIED., .F., .F.,
 ( 4, 4 ),
 ( 0.000000000000000000, 0.001030223387688887536 ),
 .UNSPECIFIED. ) ;
#32473 = CARTESIAN_POINT ( 'NONE',  ( -99.29217534005471180, -283.1938932173042645, -229.0882113862969334 ) ) ;
#32472 = CARTESIAN_POINT ( 'NONE',  ( 29.84507023166866091, -280.5294049156908613, -300.5080369959069913 ) ) ;
#32474 = CARTESIAN_POINT ( 'NONE',  ( -77.32257694246789015, -291.5880538007035625, -333.8761119678735554 ) ) ;
#32475 = CARTESIAN_POINT ( 'NONE',  ( -79.29432953402132966, -280.6766997171642970, -210.1356467112776727 ) ) ;
#32476 = CARTESIAN_POINT ( 'NONE',  ( -108.0627254117779188, -262.2579384450284010, -317.5737540118648781 ) ) ;
#32477 = CARTESIAN_POINT ( 'NONE',  ( 36.56041673708003970, -279.7172213550786068, -251.7891622266978402 ) ) ;
#32478 = CARTESIAN_POINT ( 'NONE',  ( -6.727252182799131397, -294.4541666521365642, -201.8800124452416185 ) ) ;
#32479 = CARTESIAN_POINT ( 'NONE',  ( -72.02403946465955187, -277.8398574152951142, -202.7366815037724450 ) ) ;
#32480 = CARTESIAN_POINT ( 'NONE',  ( -37.80208646944788597, -277.7094474323222926, -343.4740720598367147 ) ) ;
#32481 = CARTESIAN_POINT ( 'NONE',  ( -27.58423511042995102, -284.9287777058946176, -344.9438766267732603 ) ) ;
#32482 = CARTESIAN_POINT ( 'NONE',  ( 193.9723528053802397, 215.0000000000000568, 17.29054515234648548 ) ) ;
#32483 = CARTESIAN_POINT ( 'NONE',  ( -74.92579139469680172, -291.4687874365460516, -335.9107196758862415 ) ) ;
#32484 = CARTESIAN_POINT ( 'NONE',  ( 14.14627780109534427, -285.9504403143811260, -213.2533595926338990 ) ) ;
#32485 = CARTESIAN_POINT ( 'NONE',  ( -91.33068523627710533, -289.6678765267430435, -220.0271344497617179 ) ) ;
#32486 = CARTESIAN_POINT ( 'NONE',  ( -43.18343439339132317, -283.1093320178187582, -430.6442049081568939 ) ) ;
#32487 = CARTESIAN_POINT ( 'NONE',  ( 34.31833529681122030, -274.0225722704693112, -253.9927497677400083 ) ) ;
#32488 = CARTESIAN_POINT ( 'NONE',  ( 15.17361440809236051, -292.4412160138317063, -322.9024775557434168 ) ) ;
#32489 = CARTESIAN_POINT ( 'NONE',  ( 196.7625956450359297, 41.84090722167074006, 13.23774126259613659 ) ) ;
#32490 = DIRECTION ( 'NONE',  ( 0.000000000000000000, 1.000000000000000000, -0.000000000000000000 ) ) ;
#32491 = CARTESIAN_POINT ( 'NONE',  ( 32.69576719977037982, -291.6425581746654530, -240.0715005980366357 ) ) ;
#32492 = CARTESIAN_POINT ( 'NONE',  ( -111.1095757517718425, -286.1806999290394060, -268.1837482222301219 ) ) ;
#32493 = CARTESIAN_POINT ( 'NONE',  ( 11.74394287517603352, -286.6211308050484377, -328.3660631366237226 ) ) ;
#32494 = CARTESIAN_POINT ( 'NONE',  ( 2.752976485267746298, -288.0270291713399047, -208.6538102823708698 ) ) ;
#32495 = DIRECTION ( 'NONE',  ( 0.000000000000000000, 0.000000000000000000, -1.000000000000000000 ) ) ;
#32496 = CARTESIAN_POINT ( 'NONE',  ( 23.66306833262262188, -287.7947908036791773, -229.8835274948197025 ) ) ;
#32497 = CARTESIAN_POINT ( 'NONE',  ( -17.09334165656645510, -294.2922010771532655, -197.7772989917731650 ) ) ;
#32498 = CARTESIAN_POINT ( 'NONE',  ( -97.66878104912215974, -276.0143579469335577, -315.8791474220496411 ) ) ;
#32499 = B_SPLINE_CURVE_WITH_KNOTS ( 'NONE', 3,
 ( #84166, #48176, #12208, #35859, #27357, #77548, #64776, #41539 ),
 .UNSPECIFIED., .F., .F.,
 ( 4, 2, 2, 4 ),
 ( -4.472612521061397354E-06, 0.0004667749420422217231, 0.0007023987193238632977, 0.0009380224966055048181 ),
 .UNSPECIFIED. ) ;
#32500 = CARTESIAN_POINT ( 'NONE',  ( -112.7720585040347743, -278.6924352973895793, -285.7887082993948979 ) ) ;
#32501 = CARTESIAN_POINT ( 'NONE',  ( -37.76201442796587315, -290.1267778830119255, -194.8022830366007554 ) ) ;
#32502 = CARTESIAN_POINT ( 'NONE',  ( -73.76564290355869957, -279.5822535842049774, -202.5059403146675265 ) ) ;
#32503 = CARTESIAN_POINT ( 'NONE',  ( -55.72254121264094096, -299.7944200614800820, -197.9612934927405377 ) ) ;
#32504 = CARTESIAN_POINT ( 'NONE',  ( -48.18343439339133027, -260.4667269298406040, -492.5001339377689078 ) ) ;
#32505 = CARTESIAN_POINT ( 'NONE',  ( -110.0379128990311699, -282.3150227119010083, -288.8072910518047252 ) ) ;
#32506 = CARTESIAN_POINT ( 'NONE',  ( -48.18343439339132317, -268.0622923074284358, -498.6988577443486861 ) ) ;
#32507 = CARTESIAN_POINT ( 'NONE',  ( -110.7164920681103411, -276.5455406390557300, -281.6307847316989523 ) ) ;
#32508 = CARTESIAN_POINT ( 'NONE',  ( 22.63986663616999451, -280.1672660035160334, -315.3856923870417290 ) ) ;
#32509 = DIRECTION ( 'NONE',  ( 0.000000000000000000, 0.000000000000000000, -1.000000000000000000 ) ) ;
#32510 = CARTESIAN_POINT ( 'NONE',  ( 29.92266606438576559, -274.5032344958930253, -306.5033545522953773 ) ) ;
#32511 =( BOUNDED_CURVE ( )  B_SPLINE_CURVE ( 3, ( #63904, #56312, #78554, #71456 ),
 .UNSPECIFIED., .F., .F. ) 
 B_SPLINE_CURVE_WITH_KNOTS ( ( 4, 4 ),
 ( 3.871320309816762339, 4.712388980384689674 ),
 .UNSPECIFIED. ) 
 CURVE ( )  GEOMETRIC_REPRESENTATION_ITEM ( )  RATIONAL_B_SPLINE_CURVE ( ( 1.000000000000000000, 0.9419139527835183046, 0.9419139527835183046, 1.000000000000000000 ) ) 
 REPRESENTATION_ITEM ( '' )  );
#32512 = CARTESIAN_POINT ( 'NONE',  ( -95.30691719897633618, -297.4365997791711607, -315.8665172726256287 ) ) ;
#32513 = CARTESIAN_POINT ( 'NONE',  ( 23.99955774836108091, -281.0876062262976234, -316.3909191206939227 ) ) ;
#32514 = CARTESIAN_POINT ( 'NONE',  ( -75.34295520402633883, -298.4736196271046538, -207.6979000982530579 ) ) ;
#32515 = CARTESIAN_POINT ( 'NONE',  ( -35.50359419720567189, -299.3898790440853759, -193.8538639921639799 ) ) ;
#32516 = CARTESIAN_POINT ( 'NONE',  ( -35.38550754078937643, -273.7440612112474128, -197.3536722973015856 ) ) ;
#32517 = CARTESIAN_POINT ( 'NONE',  ( 36.88353150890747401, -295.4142531733328951, -259.6086467588099822 ) ) ;
#32518 = CARTESIAN_POINT ( 'NONE',  ( 26.35617176857961041, -287.1481718986930787, -227.0757909323515378 ) ) ;
#32519 =( BOUNDED_SURFACE ( )  B_SPLINE_SURFACE ( 3, 2, ( 
 ( #22482, #22944, #93514, #64688, #14478, #51817, #86881, #35775, #58947, #87795, #64228, #71778, #72233, #15860, #65613, #28672, #65147, #44719, #28214, #57102, #51356, #50904, #248, #80246, #21093, #36229, #57557, #49963, #86402, #21556, #29131, #7347, #7804, #50440, #58027, #44247, #79788, #725, #22035, #15383, #66069, #14930, #43785, #29611, #73157, #58489, #8280, #37160, #1181, #30062, #80710, #47030, #81629, #16316, #17256, #45630, #74537, #1639, #68373, #46115, #31462, #9669, #16776, #37607, #67455, #53704, #38552, #60351, #3503, #23879, #38997, #75018, #2583, #23427, #89188, #10131, #66520, #82571, #67909, #24341, #74070, #30519, #45168, #53216, #52747, #82096, #81172, #3035, #66976, #31918, #89651, #46574, #60810, #59417, #24821, #9189, #17719, #38067, #75472, #2115, #10595, #39456, #32395, #61294, #88731, #88271, #90129, #31005, #59891, #25280, #54157, #83026, #18180, #8731, #52293, #84894, #12005, #56041, #70722, #20533, #33788, #91533, #75933 ),
 ( #70264, #56527, #41811, #40855, #48924, #92000, #90573, #62703, #5854, #34263, #61741, #68848, #55104, #12973, #26690, #32852, #39931, #55579, #69773, #34725, #84427, #63170, #3977, #19575, #27153, #63641, #18644, #4903, #40386, #20044, #77345, #11061, #83486, #25733, #48443, #92463, #54615, #83971, #47511, #12479, #19119, #47974, #76417, #27628, #41329, #5398, #76878, #77823, #11539, #85384, #69304, #4432, #33312, #62208, #91038, #26210, #21925, #43229, #64111, #28562, #50798, #78293, #29500, #86763, #72129, #20985, #42278, #56996, #50321, #64585, #141, #28109, #93410, #13892, #79682, #36582, #87225, #57453, #71191, #29021, #49852, #79227, #78751, #65496, #42746, #22372, #80135, #36121, #51246, #35670, #6318, #86295, #71662, #6795, #21448, #14369, #1073, #7245, #8167, #65038, #58381, #57908, #15275, #44133, #87682, #14825, #43679, #49403, #72575, #7697, #615, #73038, #37051, #92949, #13431, #65962, #35186, #85834, #29953, #58837, #73510, #61176, #60236 ),
 ( #80590, #37950, #8620, #45999, #81977, #15746, #67340, #89537, #81512, #22834, #51702, #23767, #81061, #37497, #44606, #73956, #52632, #88620, #89074, #9071, #16659, #31805, #2471, #24223, #66406, #1522, #53099, #30409, #52179, #66858, #17133, #45514, #16206, #82459, #17607, #74904, #74415, #39341, #23305, #10016, #38886, #1993, #9545, #45057, #67795, #31348, #59300, #30885, #59778, #68260, #38431, #2920, #88148, #3382, #60698, #24701, #53585, #46458, #75360, #10475, #32270, #27038, #90924, #5740, #40740, #3863, #91419, #54041, #90464, #26090, #5281, #34614, #62091, #33667, #11890, #84311, #70613, #55927, #54979, #63055, #12359, #10944, #47860, #84779, #48328, #75820, #82911, #69193, #19930, #69657, #46918, #18065, #4787, #83855, #48798, #62577, #77230, #39810, #26572, #77708, #68732, #4323, #12857, #41695, #19007, #76763, #32742, #55460, #41207, #19462, #83374, #91884, #25621, #70145, #61631, #54503, #40277, #34150, #18523, #47389, #90012, #25167, #76299 ),
 ( #11425, #33200, #87121, #22271, #8055, #42158, #13783, #44028, #35, #6207, #93303, #72928, #56406, #63525, #50693, #79114, #28453, #79578, #72473, #85267, #35075, #50210, #42634, #13318, #15170, #85728, #51145, #71550, #7589, #57348, #43575, #58279, #92352, #21340, #14262, #27510, #27996, #64934, #6685, #86653, #21818, #71075, #20416, #14722, #49284, #63992, #35562, #78180, #92833, #56888, #7142, #20874, #64475, #49746, #80029, #78643, #86188, #43120, #36475, #28915, #72026, #36016, #65391, #57803, #504, #29386, #37850, #1418, #51595, #65860, #88038, #66756, #8972, #9437, #23195, #1884, #45893, #81408, #74311, #87576, #24120, #67692, #73406, #30777, #30304, #81873, #38324, #968, #44500, #58731, #67238, #24586, #75255, #16103, #8516, #45412, #73855, #59676, #29848, #2820, #2368, #88519, #23667, #44955, #22720, #52533, #17024, #16558, #31246, #31702, #52076, #60133, #88972, #52999, #80481, #74798, #9915, #15631, #38788, #60595, #89430, #37395, #66304 ),
 ( #53474, #82353, #17501, #46354, #59192, #36947, #80959, #83268, #90815, #39697, #69545, #18897, #32165, #68622, #18412, #26926, #47272, #76650, #46810, #55814, #76188, #61528, #55352, #11318, #61980, #62941, #12246, #84204, #5163, #48685, #25974, #54858, #10370, #3756, #11775, #40169, #33549, #62457, #53937, #39237, #91300, #68153, #82806, #54395, #61066, #89907, #3273, #47752, #25065, #69086, #32638, #34038, #17957, #25516, #75712, #26463, #4675, #10835, #83740, #77117, #4214, #90359, #33089, #40627, #19351, #48213, #41092, #70020, #91775, #84668, #19819, #34966, #13670, #86532, #28343, #21226, #34506, #64821, #14606, #20303, #42520, #42047, #28805, #78989, #12740, #85150, #5631, #50095, #65276, #22161, #56776, #49174, #86075, #20764, #49636, #70504, #43464, #14144, #6567, #78531, #85618, #41582, #71432, #57689, #35446, #64365, #72361, #92716, #43008, #71912, #93191, #92242, #57233, #7033, #63413, #21700, #35903, #93645, #78068, #27397, #13211, #50577, #27886 ),
 ( #79472, #7478, #36363, #381, #56287, #29269, #70961, #58165, #6094, #87009, #63878, #77589, #83043, #37737, #54174, #37285, #43916, #66191, #22608, #8407, #44385, #51952, #3994, #15512, #11081, #59079, #60021, #80843, #8859, #18196, #9320, #36830, #72811, #30190, #47048, #1771, #7936, #15054, #30655, #44844, #75949, #66645, #38203, #65749, #59556, #39948, #858, #87922, #68864, #32869, #73747, #88406, #29739, #16446, #67117, #74203, #73295, #61757, #80371, #15992, #58620, #51483, #1308, #45298, #87461, #23073, #90589, #2251, #51029, #23556, #52425, #81300, #79917, #31135, #90147, #25296, #49417, #64131, #4447, #69788, #6333, #56057, #62224, #55594, #35202, #18662, #25750, #12987, #41347, #84442, #41825, #34739, #47529, #91053, #12494, #4919, #69320, #71206, #47989, #40402, #27168, #11554, #55121, #76893, #84911, #19591, #83987, #85399, #20547, #20058, #48460, #42295, #26228, #48940, #77839, #33806, #70280, #19134, #70736, #34278, #76433, #12021, #62719 ),
 ( #40870, #91549, #26706, #77360, #5413, #54631, #63186, #78307, #92016, #63655, #5870, #92478, #13446, #83503, #27643, #56544, #33327, #57467, #630, #7258, #22387, #51259, #42760, #92965, #80150, #57012, #71680, #43244, #93425, #155, #8183, #8632, #65052, #36595, #14839, #87241, #73523, #58851, #29035, #65974, #15290, #13907, #50813, #87695, #44147, #78766, #85848, #72142, #29966, #43692, #49866, #21001, #72589, #86781, #22847, #7711, #73052, #6811, #65510, #51714, #35685, #36135, #80603, #44621, #21940, #79697, #64600, #58395, #37065, #1085, #86310, #15761, #28577, #57923, #21462, #50336, #29515, #37509, #79243, #14385, #28123, #53599, #54052, #30900, #2006, #16671, #82922, #24235, #37963, #90025, #25178, #10955, #45069, #45527, #46929, #2932, #9084, #2483, #75832, #59312, #66419, #82471, #81992, #31360, #17618, #75373, #88161, #66870, #53112, #74428, #16218, #18076, #88632, #81074, #67807, #52192, #59791, #23780, #31816, #60249, #52644, #32282, #61189 ) ),
 .UNSPECIFIED., .T., .F., .F. ) 
 B_SPLINE_SURFACE_WITH_KNOTS ( ( 4, 3, 4 ),
 ( 3, 2, 2, 2, 2, 2, 2, 2, 2, 2, 2, 2, 2, 2, 2, 2, 2, 2, 2, 2, 2, 2, 2, 2, 2, 2, 2, 2, 2, 2, 2, 2, 2, 2, 2, 2, 2, 2, 2, 2, 2, 2, 2, 2, 2, 2, 2, 2, 2, 2, 2, 2, 2, 2, 2, 2, 2, 2, 2, 2, 2, 3 ),
 ( 0.000000000000000000, 0.5000000000000000000, 1.000000000000000000 ),
 ( -0.05855608392607185297, 0.000000000000000000, 0.01428571428571428527, 0.02857142857142857054, 0.04285714285714285754, 0.05714285714285714107, 0.07142857142857142461, 0.08571428571428571508, 0.1000000000000000056, 0.1142857142857142821, 0.1285714285714285587, 0.1428571428571428492, 0.1571428571428571397, 0.1714285714285714302, 0.1857142857142857206, 0.2000000000000000111, 0.2142857142857142738, 0.2285714285714285643, 0.2428571428571428548, 0.2571428571428571175, 0.2714285714285714080, 0.2857142857142856984, 0.2999999999999999889, 0.3142857142857142794, 0.3285714285714285698, 0.3428571428571428603, 0.3571428571428571508, 0.3714285714285714413, 0.3857142857142857317, 0.4000000000000000222, 0.4142857142857143127, 0.4285714285714285476, 0.4428571428571428381, 0.4571428571428571286, 0.4714285714285714191, 0.4857142857142857095, 0.5000000000000000000, 0.5142857142857142350, 0.5285714285714285809, 0.5428571428571428159, 0.5571428571428571619, 0.5714285714285713969, 0.5857142857142857428, 0.5999999999999999778, 0.6142857142857143238, 0.6285714285714285587, 0.6428571428571429047, 0.6571428571428571397, 0.6714285714285713746, 0.6857142857142857206, 0.6999999999999999556, 0.7142857142857143016, 0.7285714285714285365, 0.7428571428571428825, 0.7571428571428571175, 0.7714285714285714635, 0.7857142857142856984, 0.8000000000000000444, 0.8142857142857142794, 0.8285714285714286254, 0.8428571428571428603, 0.8500000000000000888 ),
 .UNSPECIFIED. ) 
 GEOMETRIC_REPRESENTATION_ITEM ( )  RATIONAL_B_SPLINE_SURFACE ( (
 ( 1.000000000000000000, 1.000000000000000000, 1.000000000000000000, 0.9749279121818236193, 1.000000000000000000, 0.9749279121818236193, 1.000000000000000000, 0.9749279121818236193, 1.000000000000000000, 0.9749279121818236193, 1.000000000000000000, 0.9749279121818236193, 1.000000000000000000, 0.9749279121818236193, 1.000000000000000000, 0.9749279121818236193, 1.000000000000000000, 0.9749279121818236193, 1.000000000000000000, 0.9749279121818236193, 1.000000000000000000, 0.9749279121818236193, 1.000000000000000000, 0.9749279121818236193, 1.000000000000000000, 0.9749279121818236193, 1.000000000000000000, 0.9749279121818236193, 1.000000000000000000, 0.9749279121818236193, 1.000000000000000000, 0.9749279121818236193, 1.000000000000000000, 0.9749279121818236193, 1.000000000000000000, 0.9749279121818236193, 1.000000000000000000, 0.9749279121818236193, 1.000000000000000000, 0.9749279121818236193, 1.000000000000000000, 0.9749279121818236193, 1.000000000000000000, 0.9749279121818236193, 1.000000000000000000, 0.9749279121818236193, 1.000000000000000000, 0.9749279121818236193, 1.000000000000000000, 0.9749279121818236193, 1.000000000000000000, 0.9749279121818236193, 1.000000000000000000, 0.9749279121818236193, 1.000000000000000000, 0.9749279121818236193, 1.000000000000000000, 0.9749279121818236193, 1.000000000000000000, 0.9749279121818236193, 1.000000000000000000, 0.9749279121818236193, 1.000000000000000000, 0.9749279121818236193, 1.000000000000000000, 0.9749279121818236193, 1.000000000000000000, 0.9749279121818236193, 1.000000000000000000, 0.9749279121818236193, 1.000000000000000000, 0.9749279121818236193, 1.000000000000000000, 0.9749279121818236193, 1.000000000000000000, 0.9749279121818236193, 1.000000000000000000, 0.9749279121818236193, 1.000000000000000000, 0.9749279121818236193, 1.000000000000000000, 0.9749279121818236193, 1.000000000000000000, 0.9749279121818236193, 1.000000000000000000, 0.9749279121818236193, 1.000000000000000000, 0.9749279121818236193, 1.000000000000000000, 0.9749279121818236193, 1.000000000000000000, 0.9749279121818236193, 1.000000000000000000, 0.9749279121818236193, 1.000000000000000000, 0.9749279121818236193, 1.000000000000000000, 0.9749279121818236193, 1.000000000000000000, 0.9749279121818236193, 1.000000000000000000, 0.9749279121818236193, 1.000000000000000000, 0.9749279121818236193, 1.000000000000000000, 0.9749279121818236193, 1.000000000000000000, 0.9749279121818236193, 1.000000000000000000, 0.9749279121818236193, 1.000000000000000000, 0.9749279121818236193, 1.000000000000000000, 0.9749279121818236193, 1.000000000000000000, 0.9749279121818236193, 1.000000000000000000, 0.9749279121818236193, 1.000000000000000000, 0.9749279121818236193, 1.000000000000000000, 0.9874639560909115321, 0.9874639560909117542),
 ( 0.3333333333333333703, 0.3333333333333333703, 0.3333333333333333703, 0.3249759707272745768, 0.3333333333333333703, 0.3249759707272745768, 0.3333333333333333703, 0.3249759707272745768, 0.3333333333333333703, 0.3249759707272745768, 0.3333333333333333703, 0.3249759707272745768, 0.3333333333333333703, 0.3249759707272745768, 0.3333333333333333703, 0.3249759707272745768, 0.3333333333333333703, 0.3249759707272745768, 0.3333333333333333703, 0.3249759707272745768, 0.3333333333333333703, 0.3249759707272745768, 0.3333333333333333703, 0.3249759707272745768, 0.3333333333333333703, 0.3249759707272745768, 0.3333333333333333703, 0.3249759707272745768, 0.3333333333333333703, 0.3249759707272745768, 0.3333333333333333703, 0.3249759707272745768, 0.3333333333333333703, 0.3249759707272745768, 0.3333333333333333703, 0.3249759707272745768, 0.3333333333333333703, 0.3249759707272745768, 0.3333333333333333703, 0.3249759707272745768, 0.3333333333333333703, 0.3249759707272745768, 0.3333333333333333703, 0.3249759707272745768, 0.3333333333333333703, 0.3249759707272745768, 0.3333333333333333703, 0.3249759707272745768, 0.3333333333333333703, 0.3249759707272745768, 0.3333333333333333703, 0.3249759707272745768, 0.3333333333333333703, 0.3249759707272745768, 0.3333333333333333703, 0.3249759707272745768, 0.3333333333333333703, 0.3249759707272745768, 0.3333333333333333703, 0.3249759707272745768, 0.3333333333333333703, 0.3249759707272745768, 0.3333333333333333703, 0.3249759707272745768, 0.3333333333333333703, 0.3249759707272745768, 0.3333333333333333703, 0.3249759707272745768, 0.3333333333333333703, 0.3249759707272745768, 0.3333333333333333703, 0.3249759707272745768, 0.3333333333333333703, 0.3249759707272745768, 0.3333333333333333703, 0.3249759707272745768, 0.3333333333333333703, 0.3249759707272745768, 0.3333333333333333703, 0.3249759707272745768, 0.3333333333333333703, 0.3249759707272745768, 0.3333333333333333703, 0.3249759707272745768, 0.3333333333333333703, 0.3249759707272745768, 0.3333333333333333703, 0.3249759707272745768, 0.3333333333333333703, 0.3249759707272745768, 0.3333333333333333703, 0.3249759707272745768, 0.3333333333333333703, 0.3249759707272745768, 0.3333333333333333703, 0.3249759707272745768, 0.3333333333333333703, 0.3249759707272745768, 0.3333333333333333703, 0.3249759707272745768, 0.3333333333333333703, 0.3249759707272745768, 0.3333333333333333703, 0.3249759707272745768, 0.3333333333333333703, 0.3249759707272745768, 0.3333333333333333703, 0.3249759707272745768, 0.3333333333333333703, 0.3249759707272745768, 0.3333333333333333703, 0.3249759707272745768, 0.3333333333333333703, 0.3249759707272745768, 0.3333333333333333703, 0.3249759707272745768, 0.3333333333333333703, 0.3249759707272745768, 0.3333333333333333703, 0.3249759707272745768, 0.3333333333333333703, 0.3291546520303039181, 0.3291546520303039736),
 ( 0.3333333333333333703, 0.3333333333333333703, 0.3333333333333333703, 0.3249759707272745768, 0.3333333333333333703, 0.3249759707272745768, 0.3333333333333333703, 0.3249759707272745768, 0.3333333333333333703, 0.3249759707272745768, 0.3333333333333333703, 0.3249759707272745768, 0.3333333333333333703, 0.3249759707272745768, 0.3333333333333333703, 0.3249759707272745768, 0.3333333333333333703, 0.3249759707272745768, 0.3333333333333333703, 0.3249759707272745768, 0.3333333333333333703, 0.3249759707272745768, 0.3333333333333333703, 0.3249759707272745768, 0.3333333333333333703, 0.3249759707272745768, 0.3333333333333333703, 0.3249759707272745768, 0.3333333333333333703, 0.3249759707272745768, 0.3333333333333333703, 0.3249759707272745768, 0.3333333333333333703, 0.3249759707272745768, 0.3333333333333333703, 0.3249759707272745768, 0.3333333333333333703, 0.3249759707272745768, 0.3333333333333333703, 0.3249759707272745768, 0.3333333333333333703, 0.3249759707272745768, 0.3333333333333333703, 0.3249759707272745768, 0.3333333333333333703, 0.3249759707272745768, 0.3333333333333333703, 0.3249759707272745768, 0.3333333333333333703, 0.3249759707272745768, 0.3333333333333333703, 0.3249759707272745768, 0.3333333333333333703, 0.3249759707272745768, 0.3333333333333333703, 0.3249759707272745768, 0.3333333333333333703, 0.3249759707272745768, 0.3333333333333333703, 0.3249759707272745768, 0.3333333333333333703, 0.3249759707272745768, 0.3333333333333333703, 0.3249759707272745768, 0.3333333333333333703, 0.3249759707272745768, 0.3333333333333333703, 0.3249759707272745768, 0.3333333333333333703, 0.3249759707272745768, 0.3333333333333333703, 0.3249759707272745768, 0.3333333333333333703, 0.3249759707272745768, 0.3333333333333333703, 0.3249759707272745768, 0.3333333333333333703, 0.3249759707272745768, 0.3333333333333333703, 0.3249759707272745768, 0.3333333333333333703, 0.3249759707272745768, 0.3333333333333333703, 0.3249759707272745768, 0.3333333333333333703, 0.3249759707272745768, 0.3333333333333333703, 0.3249759707272745768, 0.3333333333333333703, 0.3249759707272745768, 0.3333333333333333703, 0.3249759707272745768, 0.3333333333333333703, 0.3249759707272745768, 0.3333333333333333703, 0.3249759707272745768, 0.3333333333333333703, 0.3249759707272745768, 0.3333333333333333703, 0.3249759707272745768, 0.3333333333333333703, 0.3249759707272745768, 0.3333333333333333703, 0.3249759707272745768, 0.3333333333333333703, 0.3249759707272745768, 0.3333333333333333703, 0.3249759707272745768, 0.3333333333333333703, 0.3249759707272745768, 0.3333333333333333703, 0.3249759707272745768, 0.3333333333333333703, 0.3249759707272745768, 0.3333333333333333703, 0.3249759707272745768, 0.3333333333333333703, 0.3249759707272745768, 0.3333333333333333703, 0.3249759707272745768, 0.3333333333333333703, 0.3291546520303039181, 0.3291546520303039736),
 ( 1.000000000000000000, 1.000000000000000000, 1.000000000000000000, 0.9749279121818236193, 1.000000000000000000, 0.9749279121818236193, 1.000000000000000000, 0.9749279121818236193, 1.000000000000000000, 0.9749279121818236193, 1.000000000000000000, 0.9749279121818236193, 1.000000000000000000, 0.9749279121818236193, 1.000000000000000000, 0.9749279121818236193, 1.000000000000000000, 0.9749279121818236193, 1.000000000000000000, 0.9749279121818236193, 1.000000000000000000, 0.9749279121818236193, 1.000000000000000000, 0.9749279121818236193, 1.000000000000000000, 0.9749279121818236193, 1.000000000000000000, 0.9749279121818236193, 1.000000000000000000, 0.9749279121818236193, 1.000000000000000000, 0.9749279121818236193, 1.000000000000000000, 0.9749279121818236193, 1.000000000000000000, 0.9749279121818236193, 1.000000000000000000, 0.9749279121818236193, 1.000000000000000000, 0.9749279121818236193, 1.000000000000000000, 0.9749279121818236193, 1.000000000000000000, 0.9749279121818236193, 1.000000000000000000, 0.9749279121818236193, 1.000000000000000000, 0.9749279121818236193, 1.000000000000000000, 0.9749279121818236193, 1.000000000000000000, 0.9749279121818236193, 1.000000000000000000, 0.9749279121818236193, 1.000000000000000000, 0.9749279121818236193, 1.000000000000000000, 0.9749279121818236193, 1.000000000000000000, 0.9749279121818236193, 1.000000000000000000, 0.9749279121818236193, 1.000000000000000000, 0.9749279121818236193, 1.000000000000000000, 0.9749279121818236193, 1.000000000000000000, 0.9749279121818236193, 1.000000000000000000, 0.9749279121818236193, 1.000000000000000000, 0.9749279121818236193, 1.000000000000000000, 0.9749279121818236193, 1.000000000000000000, 0.9749279121818236193, 1.000000000000000000, 0.9749279121818236193, 1.000000000000000000, 0.9749279121818236193, 1.000000000000000000, 0.9749279121818236193, 1.000000000000000000, 0.9749279121818236193, 1.000000000000000000, 0.9749279121818236193, 1.000000000000000000, 0.9749279121818236193, 1.000000000000000000, 0.9749279121818236193, 1.000000000000000000, 0.9749279121818236193, 1.000000000000000000, 0.9749279121818236193, 1.000000000000000000, 0.9749279121818236193, 1.000000000000000000, 0.9749279121818236193, 1.000000000000000000, 0.9749279121818236193, 1.000000000000000000, 0.9749279121818236193, 1.000000000000000000, 0.9749279121818236193, 1.000000000000000000, 0.9749279121818236193, 1.000000000000000000, 0.9749279121818236193, 1.000000000000000000, 0.9749279121818236193, 1.000000000000000000, 0.9749279121818236193, 1.000000000000000000, 0.9749279121818236193, 1.000000000000000000, 0.9749279121818236193, 1.000000000000000000, 0.9749279121818236193, 1.000000000000000000, 0.9749279121818236193, 1.000000000000000000, 0.9874639560909115321, 0.9874639560909117542),
 ( 0.3333333333333333703, 0.3333333333333333703, 0.3333333333333333703, 0.3249759707272745768, 0.3333333333333333703, 0.3249759707272745768, 0.3333333333333333703, 0.3249759707272745768, 0.3333333333333333703, 0.3249759707272745768, 0.3333333333333333703, 0.3249759707272745768, 0.3333333333333333703, 0.3249759707272745768, 0.3333333333333333703, 0.3249759707272745768, 0.3333333333333333703, 0.3249759707272745768, 0.3333333333333333703, 0.3249759707272745768, 0.3333333333333333703, 0.3249759707272745768, 0.3333333333333333703, 0.3249759707272745768, 0.3333333333333333703, 0.3249759707272745768, 0.3333333333333333703, 0.3249759707272745768, 0.3333333333333333703, 0.3249759707272745768, 0.3333333333333333703, 0.3249759707272745768, 0.3333333333333333703, 0.3249759707272745768, 0.3333333333333333703, 0.3249759707272745768, 0.3333333333333333703, 0.3249759707272745768, 0.3333333333333333703, 0.3249759707272745768, 0.3333333333333333703, 0.3249759707272745768, 0.3333333333333333703, 0.3249759707272745768, 0.3333333333333333703, 0.3249759707272745768, 0.3333333333333333703, 0.3249759707272745768, 0.3333333333333333703, 0.3249759707272745768, 0.3333333333333333703, 0.3249759707272745768, 0.3333333333333333703, 0.3249759707272745768, 0.3333333333333333703, 0.3249759707272745768, 0.3333333333333333703, 0.3249759707272745768, 0.3333333333333333703, 0.3249759707272745768, 0.3333333333333333703, 0.3249759707272745768, 0.3333333333333333703, 0.3249759707272745768, 0.3333333333333333703, 0.3249759707272745768, 0.3333333333333333703, 0.3249759707272745768, 0.3333333333333333703, 0.3249759707272745768, 0.3333333333333333703, 0.3249759707272745768, 0.3333333333333333703, 0.3249759707272745768, 0.3333333333333333703, 0.3249759707272745768, 0.3333333333333333703, 0.3249759707272745768, 0.3333333333333333703, 0.3249759707272745768, 0.3333333333333333703, 0.3249759707272745768, 0.3333333333333333703, 0.3249759707272745768, 0.3333333333333333703, 0.3249759707272745768, 0.3333333333333333703, 0.3249759707272745768, 0.3333333333333333703, 0.3249759707272745768, 0.3333333333333333703, 0.3249759707272745768, 0.3333333333333333703, 0.3249759707272745768, 0.3333333333333333703, 0.3249759707272745768, 0.3333333333333333703, 0.3249759707272745768, 0.3333333333333333703, 0.3249759707272745768, 0.3333333333333333703, 0.3249759707272745768, 0.3333333333333333703, 0.3249759707272745768, 0.3333333333333333703, 0.3249759707272745768, 0.3333333333333333703, 0.3249759707272745768, 0.3333333333333333703, 0.3249759707272745768, 0.3333333333333333703, 0.3249759707272745768, 0.3333333333333333703, 0.3249759707272745768, 0.3333333333333333703, 0.3249759707272745768, 0.3333333333333333703, 0.3249759707272745768, 0.3333333333333333703, 0.3249759707272745768, 0.3333333333333333703, 0.3291546520303039181, 0.3291546520303039736),
 ( 0.3333333333333333703, 0.3333333333333333703, 0.3333333333333333703, 0.3249759707272745768, 0.3333333333333333703, 0.3249759707272745768, 0.3333333333333333703, 0.3249759707272745768, 0.3333333333333333703, 0.3249759707272745768, 0.3333333333333333703, 0.3249759707272745768, 0.3333333333333333703, 0.3249759707272745768, 0.3333333333333333703, 0.3249759707272745768, 0.3333333333333333703, 0.3249759707272745768, 0.3333333333333333703, 0.3249759707272745768, 0.3333333333333333703, 0.3249759707272745768, 0.3333333333333333703, 0.3249759707272745768, 0.3333333333333333703, 0.3249759707272745768, 0.3333333333333333703, 0.3249759707272745768, 0.3333333333333333703, 0.3249759707272745768, 0.3333333333333333703, 0.3249759707272745768, 0.3333333333333333703, 0.3249759707272745768, 0.3333333333333333703, 0.3249759707272745768, 0.3333333333333333703, 0.3249759707272745768, 0.3333333333333333703, 0.3249759707272745768, 0.3333333333333333703, 0.3249759707272745768, 0.3333333333333333703, 0.3249759707272745768, 0.3333333333333333703, 0.3249759707272745768, 0.3333333333333333703, 0.3249759707272745768, 0.3333333333333333703, 0.3249759707272745768, 0.3333333333333333703, 0.3249759707272745768, 0.3333333333333333703, 0.3249759707272745768, 0.3333333333333333703, 0.3249759707272745768, 0.3333333333333333703, 0.3249759707272745768, 0.3333333333333333703, 0.3249759707272745768, 0.3333333333333333703, 0.3249759707272745768, 0.3333333333333333703, 0.3249759707272745768, 0.3333333333333333703, 0.3249759707272745768, 0.3333333333333333703, 0.3249759707272745768, 0.3333333333333333703, 0.3249759707272745768, 0.3333333333333333703, 0.3249759707272745768, 0.3333333333333333703, 0.3249759707272745768, 0.3333333333333333703, 0.3249759707272745768, 0.3333333333333333703, 0.3249759707272745768, 0.3333333333333333703, 0.3249759707272745768, 0.3333333333333333703, 0.3249759707272745768, 0.3333333333333333703, 0.3249759707272745768, 0.3333333333333333703, 0.3249759707272745768, 0.3333333333333333703, 0.3249759707272745768, 0.3333333333333333703, 0.3249759707272745768, 0.3333333333333333703, 0.3249759707272745768, 0.3333333333333333703, 0.3249759707272745768, 0.3333333333333333703, 0.3249759707272745768, 0.3333333333333333703, 0.3249759707272745768, 0.3333333333333333703, 0.3249759707272745768, 0.3333333333333333703, 0.3249759707272745768, 0.3333333333333333703, 0.3249759707272745768, 0.3333333333333333703, 0.3249759707272745768, 0.3333333333333333703, 0.3249759707272745768, 0.3333333333333333703, 0.3249759707272745768, 0.3333333333333333703, 0.3249759707272745768, 0.3333333333333333703, 0.3249759707272745768, 0.3333333333333333703, 0.3249759707272745768, 0.3333333333333333703, 0.3249759707272745768, 0.3333333333333333703, 0.3249759707272745768, 0.3333333333333333703, 0.3291546520303039181, 0.3291546520303039736),
 ( 1.000000000000000000, 1.000000000000000000, 1.000000000000000000, 0.9749279121818236193, 1.000000000000000000, 0.9749279121818236193, 1.000000000000000000, 0.9749279121818236193, 1.000000000000000000, 0.9749279121818236193, 1.000000000000000000, 0.9749279121818236193, 1.000000000000000000, 0.9749279121818236193, 1.000000000000000000, 0.9749279121818236193, 1.000000000000000000, 0.9749279121818236193, 1.000000000000000000, 0.9749279121818236193, 1.000000000000000000, 0.9749279121818236193, 1.000000000000000000, 0.9749279121818236193, 1.000000000000000000, 0.9749279121818236193, 1.000000000000000000, 0.9749279121818236193, 1.000000000000000000, 0.9749279121818236193, 1.000000000000000000, 0.9749279121818236193, 1.000000000000000000, 0.9749279121818236193, 1.000000000000000000, 0.9749279121818236193, 1.000000000000000000, 0.9749279121818236193, 1.000000000000000000, 0.9749279121818236193, 1.000000000000000000, 0.9749279121818236193, 1.000000000000000000, 0.9749279121818236193, 1.000000000000000000, 0.9749279121818236193, 1.000000000000000000, 0.9749279121818236193, 1.000000000000000000, 0.9749279121818236193, 1.000000000000000000, 0.9749279121818236193, 1.000000000000000000, 0.9749279121818236193, 1.000000000000000000, 0.9749279121818236193, 1.000000000000000000, 0.9749279121818236193, 1.000000000000000000, 0.9749279121818236193, 1.000000000000000000, 0.9749279121818236193, 1.000000000000000000, 0.9749279121818236193, 1.000000000000000000, 0.9749279121818236193, 1.000000000000000000, 0.9749279121818236193, 1.000000000000000000, 0.9749279121818236193, 1.000000000000000000, 0.9749279121818236193, 1.000000000000000000, 0.9749279121818236193, 1.000000000000000000, 0.9749279121818236193, 1.000000000000000000, 0.9749279121818236193, 1.000000000000000000, 0.9749279121818236193, 1.000000000000000000, 0.9749279121818236193, 1.000000000000000000, 0.9749279121818236193, 1.000000000000000000, 0.9749279121818236193, 1.000000000000000000, 0.9749279121818236193, 1.000000000000000000, 0.9749279121818236193, 1.000000000000000000, 0.9749279121818236193, 1.000000000000000000, 0.9749279121818236193, 1.000000000000000000, 0.9749279121818236193, 1.000000000000000000, 0.9749279121818236193, 1.000000000000000000, 0.9749279121818236193, 1.000000000000000000, 0.9749279121818236193, 1.000000000000000000, 0.9749279121818236193, 1.000000000000000000, 0.9749279121818236193, 1.000000000000000000, 0.9749279121818236193, 1.000000000000000000, 0.9749279121818236193, 1.000000000000000000, 0.9749279121818236193, 1.000000000000000000, 0.9749279121818236193, 1.000000000000000000, 0.9749279121818236193, 1.000000000000000000, 0.9749279121818236193, 1.000000000000000000, 0.9749279121818236193, 1.000000000000000000, 0.9874639560909115321, 0.9874639560909117542) ) ) 
 REPRESENTATION_ITEM ( '' )  SURFACE ( )  );
#32520 = CARTESIAN_POINT ( 'NONE',  ( 18.94344743393842379, -274.3916380513207969, -321.0982514603747973 ) ) ;
#32521 = AXIS2_PLACEMENT_3D ( 'NONE', #52570, #22310, #44993 ) ;
#32522 = CARTESIAN_POINT ( 'NONE',  ( -38.92230237488710287, -288.9047901732640184, -347.3448935529162327 ) ) ;
#32523 = EDGE_CURVE ( 'NONE', #48610, #85305, #50502, .T. ) ;
#32524 = CARTESIAN_POINT ( 'NONE',  ( 35.89035233665204316, -286.6199563678704862, -271.0502762912408343 ) ) ;
#32525 = CARTESIAN_POINT ( 'NONE',  ( -105.4336747403305736, -288.9663577027548627, -238.7973145445781711 ) ) ;
#32526 = ORIENTED_EDGE ( 'NONE', *, *, #66323, .F. ) ;
#32527 = CARTESIAN_POINT ( 'NONE',  ( 142.9247625494386114, 180.1091408837567371, -243.7470944784683127 ) ) ;
#32528 = CARTESIAN_POINT ( 'NONE',  ( 21.21905379106112832, -287.6725291631148593, -314.0698889227368227 ) ) ;
#32529 = DIRECTION ( 'NONE',  ( 1.000000000000000000, 0.000000000000000000, 0.000000000000000000 ) ) ;
#32530 = CARTESIAN_POINT ( 'NONE',  ( -93.25192376431468233, -284.7730479017733956, -322.9814034909980478 ) ) ;
#32531 = AXIS2_PLACEMENT_3D ( 'NONE', #19728, #91207, #69926 ) ;
#32532 = CARTESIAN_POINT ( 'NONE',  ( -37.78161740844839755, -291.1055214671724229, -193.5976716885569715 ) ) ;
#32533 = CARTESIAN_POINT ( 'NONE',  ( 19.51800930064586836, -282.4570673089704087, -219.6126778980658969 ) ) ;
#32534 = CARTESIAN_POINT ( 'NONE',  ( 33.85928772399658016, -282.5084869852112774, -242.2216466203130665 ) ) ;
#32535 = CARTESIAN_POINT ( 'NONE',  ( -69.01108493927020504, -283.3139436960800595, -336.1476363990104801 ) ) ;
#32536 = CARTESIAN_POINT ( 'NONE',  ( 18.95283399503109933, -278.2412231387264114, -319.9378017746700493 ) ) ;
#32537 = CARTESIAN_POINT ( 'NONE',  ( -101.5496900522852570, -297.1114765037191319, -227.8361201488905010 ) ) ;
#32538 = CARTESIAN_POINT ( 'NONE',  ( -21.84627247365913050, -275.5700987234985178, -198.5200767987247161 ) ) ;
#32539 = CARTESIAN_POINT ( 'NONE',  ( -1.630855336697323299, -290.5479465435475959, -204.7982798323102429 ) ) ;
#32540 = CIRCLE ( 'NONE', #88481, 4.000000000000003553 ) ;
#32541 = CARTESIAN_POINT ( 'NONE',  ( -102.3751945454019108, -271.8089483051880961, -236.2249873332977188 ) ) ;
#32542 = VERTEX_POINT ( 'NONE', #36538 ) ;
#32543 = LINE ( 'NONE', #60953, #83371 ) ;
#32544 = CARTESIAN_POINT ( 'NONE',  ( -108.3523298941789648, -286.1820054077951454, -292.6950531118995968 ) ) ;
#32545 = CARTESIAN_POINT ( 'NONE',  ( -0.8411337741704904003, -295.6587920977971180, -337.8237109144015449 ) ) ;
#32546 = CARTESIAN_POINT ( 'NONE',  ( -71.23283552471657742, -286.2436463648190283, -205.5901089585561010 ) ) ;
#32547 = CARTESIAN_POINT ( 'NONE',  ( 38.90242257371527757, -274.7284465392191350, -279.7311097166445961 ) ) ;
#32548 = CARTESIAN_POINT ( 'NONE',  ( 32.09035506203767341, -293.7779260142291378, -237.1843730163055000 ) ) ;
#32549 = CARTESIAN_POINT ( 'NONE',  ( -13.07652042498867928, -284.5037083708650130, -198.5871217649060725 ) ) ;
#32550 = CARTESIAN_POINT ( 'NONE',  ( -22.20210260406828695, -292.5741117308735397, -194.8314014930393512 ) ) ;
#32551 = CARTESIAN_POINT ( 'NONE',  ( -42.66121851866647319, -289.4542498486399609, -343.2388620441287230 ) ) ;
#32552 = FACE_OUTER_BOUND ( 'NONE', #87279, .T. ) ;
#32553 = CARTESIAN_POINT ( 'NONE',  ( 175.2296996224750103, 275.5000000000000568, 0.000000000000000000 ) ) ;
#32554 = CARTESIAN_POINT ( 'NONE',  ( 153.7037580466550821, 204.4818557570326902, -214.3672810361624954 ) ) ;
#32555 = CARTESIAN_POINT ( 'NONE',  ( -43.62862356746156678, -287.4943387594404385, -194.2611003048058080 ) ) ;
#32556 = CARTESIAN_POINT ( 'NONE',  ( -110.4683760289727132, -293.8380690714490129, -287.0191576251351080 ) ) ;
#32557 = ORIENTED_EDGE ( 'NONE', *, *, #80129, .F. ) ;
#32558 = CARTESIAN_POINT ( 'NONE',  ( 19.58339992406645180, -281.1235365961811112, -316.5735305848129997 ) ) ;
#32559 = CARTESIAN_POINT ( 'NONE',  ( -98.78910984784262439, -277.6009742027237621, -316.7504160945661056 ) ) ;
#32560 = CARTESIAN_POINT ( 'NONE',  ( -88.80956642426248493, -281.3280777181398093, -215.9655722439982810 ) ) ;
#32561 = CARTESIAN_POINT ( 'NONE',  ( 7.628150327998172386, -59.94677518897242408, -352.6193804921139758 ) ) ;
#32562 = CARTESIAN_POINT ( 'NONE',  ( 23.77282892130728698, -280.7420612147766974, -316.2263622695442677 ) ) ;
#32563 = CARTESIAN_POINT ( 'NONE',  ( 19.93982566509851395, -284.9077454862041918, -222.4802139764734363 ) ) ;
#32564 = CARTESIAN_POINT ( 'NONE',  ( -93.25005675248959847, -275.1194957952901063, -219.2091760476533864 ) ) ;
#32565 = CARTESIAN_POINT ( 'NONE',  ( -53.15659392583427945, -295.7526531643723615, -341.7425053747863899 ) ) ;
#32566 = ORIENTED_EDGE ( 'NONE', *, *, #41871, .F. ) ;
#32567 = CARTESIAN_POINT ( 'NONE',  ( -4.598420262554686389, -291.1776227519213762, -204.5510410903042953 ) ) ;
#32568 = CARTESIAN_POINT ( 'NONE',  ( 35.96796492082727070, -276.4957529148528579, -293.5776163616141048 ) ) ;
#32569 = CARTESIAN_POINT ( 'NONE',  ( -56.86161410190220522, -273.7934600391721460, -199.9665721671149754 ) ) ;
#32570 = CARTESIAN_POINT ( 'NONE',  ( 21.62204935220675495, -273.8102839982756791, -221.3226763461425151 ) ) ;
#32571 = DIRECTION ( 'NONE',  ( 1.000000000000000000, 0.000000000000000000, -0.000000000000000000 ) ) ;
#32572 = CARTESIAN_POINT ( 'NONE',  ( -98.10083840596374216, -271.1517187724923019, -226.3059262207511324 ) ) ;
#32573 = CARTESIAN_POINT ( 'NONE',  ( -8.592757392746911194, -296.1085985611081810, -341.2133927272473670 ) ) ;
#32574 = CARTESIAN_POINT ( 'NONE',  ( 151.0524635986548674, 20.99320456764978715, 6.527652849435607862 ) ) ;
#32575 = CARTESIAN_POINT ( 'NONE',  ( -43.27353253609506112, -275.1640841960933699, -506.7538176778678576 ) ) ;
#32576 = CARTESIAN_POINT ( 'NONE',  ( -107.6846607907899056, -285.3593448261918866, -291.0479521449954632 ) ) ;
#32577 = CARTESIAN_POINT ( 'NONE',  ( 37.25555664430955716, -283.1289766948790998, -255.8965648295680637 ) ) ;
#32578 = CARTESIAN_POINT ( 'NONE',  ( -101.8650957439092650, -283.4318674650633056, -304.8290872300131582 ) ) ;
#32579 = CARTESIAN_POINT ( 'NONE',  ( -46.02220270507082489, -275.5637852912332733, -343.7000149732379555 ) ) ;
#32580 = CARTESIAN_POINT ( 'NONE',  ( -64.48532464259463381, -285.2706934516060073, -339.4559016423420417 ) ) ;
#32581 = CARTESIAN_POINT ( 'NONE',  ( -87.58222021782127342, -276.2489144919182991, -324.2739911415999359 ) ) ;
#32582 = CARTESIAN_POINT ( 'NONE',  ( 32.35140462297783159, -276.3294134809819411, -247.4581411124910630 ) ) ;
#32583 = DIRECTION ( 'NONE',  ( 0.000000000000000000, 0.000000000000000000, 1.000000000000000000 ) ) ;
#32584 = CARTESIAN_POINT ( 'NONE',  ( -71.17272845035346052, -280.4197192067070432, -201.3711162142269586 ) ) ;
#32585 = EDGE_CURVE ( 'NONE', #30930, #86528, #68911, .T. ) ;
#32586 = ORIENTED_EDGE ( 'NONE', *, *, #11892, .T. ) ;
#32587 = CARTESIAN_POINT ( 'NONE',  ( 198.0894686820290929, 18.12099305396683135, 11.05388702473232954 ) ) ;
#32588 = CARTESIAN_POINT ( 'NONE',  ( -35.20716411502890963, -287.9390621576985723, -194.6134557383130073 ) ) ;
#32589 = CARTESIAN_POINT ( 'NONE',  ( -93.21231361429809681, -295.0793352926049806, -317.6147993215997190 ) ) ;
#32590 = EDGE_CURVE ( 'NONE', #79924, #19058, #57410, .T. ) ;
#32591 = CARTESIAN_POINT ( 'NONE',  ( -113.0344426688517814, -289.7299764032954386, -283.9973048989509152 ) ) ;
#32593 = CARTESIAN_POINT ( 'NONE',  ( -82.32743018945153324, -289.6688381264211785, -211.5233428701100991 ) ) ;
#32592 = CARTESIAN_POINT ( 'NONE',  ( -4.313967146831214627, -285.0710969631329590, -204.5998545141580109 ) ) ;
#32594 = CARTESIAN_POINT ( 'NONE',  ( -110.6257117043976592, -285.8216191337056671, -265.4538637725397621 ) ) ;
#32595 = CARTESIAN_POINT ( 'NONE',  ( 25.94708344254813781, -274.0946431780135413, -310.7009957916968119 ) ) ;
#32596 = CARTESIAN_POINT ( 'NONE',  ( 33.29301819966787690, -286.3203733230026842, -299.0878774437168204 ) ) ;
#32597 = CARTESIAN_POINT ( 'NONE',  ( -21.43367214812339938, -288.2563288124215433, -197.0676306086918430 ) ) ;
#32598 = CARTESIAN_POINT ( 'NONE',  ( 31.05466940947928478, -285.1423027177601170, -239.0593728467056849 ) ) ;
#32599 = CARTESIAN_POINT ( 'NONE',  ( 20.37378398356347731, -283.1267792657722566, -315.4425037494083881 ) ) ;
#32600 = CARTESIAN_POINT ( 'NONE',  ( -2.624290777631910210, -290.5942469099274490, -337.0299256629942306 ) ) ;
#32601 = CARTESIAN_POINT ( 'NONE',  ( 191.4749582765727212, 14.19731191252289015, 13.00000000000000178 ) ) ;
#32602 = CARTESIAN_POINT ( 'NONE',  ( 197.1513938986460062, -147.7221692137691775, 1.978481845683761620 ) ) ;
#32603 = CARTESIAN_POINT ( 'NONE',  ( -100.4125407091589324, -297.9136228988910489, -312.0655920973689490 ) ) ;
#32604 = VECTOR ( 'NONE', #93117, 1000.000000000000000 ) ;
#32605 = CARTESIAN_POINT ( 'NONE',  ( -65.54522211681664601, -277.6832125674926601, -200.8660678185027280 ) ) ;
#32606 = CARTESIAN_POINT ( 'NONE',  ( 17.38180141793691647, -292.0063132420249303, -216.3464293578725517 ) ) ;
#32607 = CARTESIAN_POINT ( 'NONE',  ( -103.2375753620756740, -295.3995041303965081, -237.0182795954090125 ) ) ;
#32608 = CARTESIAN_POINT ( 'NONE',  ( 24.10398729477568835, -279.6806568240900219, -229.9497019746799538 ) ) ;
#32609 = CARTESIAN_POINT ( 'NONE',  ( -35.32732633982873693, -272.1574449580455735, -195.9356220532301620 ) ) ;
#32610 = CARTESIAN_POINT ( 'NONE',  ( 26.22756049788171850, -295.3698947154877601, -307.2419067558803363 ) ) ;
#32611 = CARTESIAN_POINT ( 'NONE',  ( -113.5916813653544324, -271.1988319013034356, -264.6520495995177953 ) ) ;
#32612 = CARTESIAN_POINT ( 'NONE',  ( 37.81098343651878935, -291.9342970149134544, -281.5882354615037002 ) ) ;
#32613 = CARTESIAN_POINT ( 'NONE',  ( -33.49564653083918131, -293.5267524977109019, -196.8598672718253511 ) ) ;
#32614 = FACE_OUTER_BOUND ( 'NONE', #31754, .T. ) ;
#32615 = CARTESIAN_POINT ( 'NONE',  ( 35.06609209193271681, -294.2171184629137315, -259.8867037813033107 ) ) ;
#32616 = DIRECTION ( 'NONE',  ( 0.000000000000000000, 0.000000000000000000, 1.000000000000000000 ) ) ;
#32618 = CARTESIAN_POINT ( 'NONE',  ( 25.79266356301712548, -294.0549325069128486, -307.0087935066652562 ) ) ;
#32617 = CARTESIAN_POINT ( 'NONE',  ( -11.29474762352851691, -280.7346911788825423, -341.1269635043336734 ) ) ;
#32619 = CARTESIAN_POINT ( 'NONE',  ( -5.455519030079051035, -282.6441329965845171, -340.4487164218373891 ) ) ;
#32620 = CARTESIAN_POINT ( 'NONE',  ( -112.5053660341964274, -284.0109811661047274, -286.9794096883084649 ) ) ;
#32621 = CARTESIAN_POINT ( 'NONE',  ( -111.4418288685744187, -288.4163302953746779, -280.9031186873637012 ) ) ;
#32622 = CARTESIAN_POINT ( 'NONE',  ( 195.4781563537916043, 250.0000000000000568, 15.50000000000000000 ) ) ;
#32623 = CARTESIAN_POINT ( 'NONE',  ( 38.49598568334300097, -279.9195783348995974, -261.4503271250531498 ) ) ;
#32624 = CARTESIAN_POINT ( 'NONE',  ( -1.955624179986581668, -287.5149129998451940, -338.4002107134614903 ) ) ;
#32625 = CARTESIAN_POINT ( 'NONE',  ( 29.33919985515026596, -232.1443419142230766, 22.50000000000000000 ) ) ;
#32626 = CARTESIAN_POINT ( 'NONE',  ( -17.99133341322022872, -296.3986251899053173, -341.5791193670521579 ) ) ;
#32627 = CARTESIAN_POINT ( 'NONE',  ( 23.90631692584607748, -277.5898391021814291, -316.0479508920313378 ) ) ;
#32628 = CARTESIAN_POINT ( 'NONE',  ( -70.94762243691920389, -279.2626800250376391, -205.5185648521822657 ) ) ;
#32629 = CARTESIAN_POINT ( 'NONE',  ( 20.37728320186107567, -293.0284912539166839, -219.3753376206050518 ) ) ;
#32630 = CARTESIAN_POINT ( 'NONE',  ( -105.3718039394970845, -283.0619493256399437, -237.4792206750342132 ) ) ;
#32631 = CARTESIAN_POINT ( 'NONE',  ( -38.48816034180434542, -279.0666862744751029, -345.3523593491173642 ) ) ;
#32632 = CARTESIAN_POINT ( 'NONE',  ( -5.929873331001648928, -291.5342566468563064, -204.1906158462052474 ) ) ;
#32633 = CARTESIAN_POINT ( 'NONE',  ( -95.77176462076158714, -295.1990049728523218, -223.3406095111847947 ) ) ;
#32634 = EDGE_LOOP ( 'NONE', ( #39409, #27624, #92055, #56834 ) ) ;
#32635 = DIRECTION ( 'NONE',  ( 1.000000000000000000, 0.000000000000000000, 0.000000000000000000 ) ) ;
#32636 = CARTESIAN_POINT ( 'NONE',  ( -3.120477932512370156, -294.0947776773638225, -334.9126198492454023 ) ) ;
#32637 = CARTESIAN_POINT ( 'NONE',  ( 133.0380396672494783, -299.5541904835127980, -201.5129295623840449 ) ) ;
#32638 = CARTESIAN_POINT ( 'NONE',  ( 30.89617123739170168, -285.2666405000203440, -285.9686137636504668 ) ) ;
#32639 = CARTESIAN_POINT ( 'NONE',  ( -97.67990044980372488, -272.3869977470603772, -222.7852795422845986 ) ) ;
#32640 = CARTESIAN_POINT ( 'NONE',  ( 38.04650232677378341, -279.7940556838514112, -278.4112173359901021 ) ) ;
#32641 = EDGE_CURVE ( 'NONE', #52690, #82136, #68691, .T. ) ;
#32642 = EDGE_CURVE ( 'NONE', #73985, #17168, #13729, .T. ) ;
#32643 = CARTESIAN_POINT ( 'NONE',  ( -70.86534981146397172, -286.9342654913240267, -201.5900253128242241 ) ) ;
#32644 = CARTESIAN_POINT ( 'NONE',  ( 16.00951215050787368, -288.1027900811589575, -320.2612584891847405 ) ) ;
#32645 = CARTESIAN_POINT ( 'NONE',  ( -105.9058627385197724, -279.7144267401990874, -297.3733995713358809 ) ) ;
#32646 = CARTESIAN_POINT ( 'NONE',  ( -70.94740970461043617, -299.3626559870327810, -204.4028662670947938 ) ) ;
#32647 = CARTESIAN_POINT ( 'NONE',  ( -51.37173314567550619, -276.0304839186034656, -342.4047761157377749 ) ) ;
#32648 = VERTEX_POINT ( 'NONE', #25127 ) ;
#32649 = CARTESIAN_POINT ( 'NONE',  ( -37.24935154739976895, -297.7200014266754806, -193.3815033725163914 ) ) ;
#32650 = CARTESIAN_POINT ( 'NONE',  ( -111.0453187876244243, -292.3360123529516841, -280.8970101591545472 ) ) ;
#32651 = CARTESIAN_POINT ( 'NONE',  ( 23.32580779890089673, -294.5311298411430698, -224.2322362664154412 ) ) ;
#32652 = CARTESIAN_POINT ( 'NONE',  ( -114.0438498160389287, -273.6021560138187851, -270.3744733279939965 ) ) ;
#32653 = CARTESIAN_POINT ( 'NONE',  ( -78.22456173008137625, -290.2692494534612138, -331.0230789929115645 ) ) ;
#32654 = CARTESIAN_POINT ( 'NONE',  ( -48.18343439339648171, -250.1936144431593050, -454.4903112404356307 ) ) ;
#32655 = CARTESIAN_POINT ( 'NONE',  ( -6.369840509506259352, -290.5942145151285558, -201.2019235178256338 ) ) ;
#32656 = CARTESIAN_POINT ( 'NONE',  ( -80.61664344311897423, -297.8163796204223672, -206.6336646993826207 ) ) ;
#32657 = CARTESIAN_POINT ( 'NONE',  ( -60.51858921352709331, -297.4099558805892798, -201.0622787149973760 ) ) ;
#32658 = DIRECTION ( 'NONE',  ( 0.000000000000000000, 1.000000000000000000, 0.000000000000000000 ) ) ;
#32659 = CARTESIAN_POINT ( 'NONE',  ( 195.9246352305470680, 25.72798252258608898, 14.39643678788906378 ) ) ;
#32660 = CARTESIAN_POINT ( 'NONE',  ( -93.07305233325782012, -291.3542938526953208, -322.5594508509145157 ) ) ;
#32661 = CARTESIAN_POINT ( 'NONE',  ( 40.64545035920995986, -295.8376638359844719, -252.5284128619064461 ) ) ;
#32662 = CARTESIAN_POINT ( 'NONE',  ( -96.41971609698404677, -287.1838143107498809, -224.4075638634668621 ) ) ;
#32663 = CARTESIAN_POINT ( 'NONE',  ( -43.61094082968497787, -271.9727322639777753, -195.7388650299787685 ) ) ;
#32664 = CARTESIAN_POINT ( 'NONE',  ( -66.39732374049609120, -275.5888570046891459, -201.8258355646289601 ) ) ;
#32665 = CARTESIAN_POINT ( 'NONE',  ( -37.52951084827729034, -290.1296663984609836, -195.9086612669253213 ) ) ;
#32666 = CARTESIAN_POINT ( 'NONE',  ( -110.2454055409880027, -280.1498624873998438, -290.9852596366845319 ) ) ;
#32667 = AXIS2_PLACEMENT_3D ( 'NONE', #37757, #8426, #1327 ) ;
#32668 = ORIENTED_EDGE ( 'NONE', *, *, #26328, .T. ) ;
#32669 = CARTESIAN_POINT ( 'NONE',  ( 13.99036024220834307, -281.6572649159380148, -322.4795930979910850 ) ) ;
#32670 = CARTESIAN_POINT ( 'NONE',  ( -112.7591302074039845, -279.4561518100393300, -284.3509493984951177 ) ) ;
#32671 = CARTESIAN_POINT ( 'NONE',  ( -19.83199417319972468, -279.0671977339699197, -195.7317056704644642 ) ) ;
#32672 = CARTESIAN_POINT ( 'NONE',  ( 151.8863250319597000, 206.1547615615816369, -215.0904922897478571 ) ) ;
#32673 = CARTESIAN_POINT ( 'NONE',  ( 24.18627271408411517, -277.1058970528413852, -316.2645903081284473 ) ) ;
#32674 = CARTESIAN_POINT ( 'NONE',  ( -60.67766905526730170, -275.2750443224867354, -197.6551726798747666 ) ) ;
#32675 = CARTESIAN_POINT ( 'NONE',  ( -69.91165696735023971, -300.1233781216987495, -202.8022627189028810 ) ) ;
#32676 = ORIENTED_EDGE ( 'NONE', *, *, #32590, .T. ) ;
#32677 = VERTEX_POINT ( 'NONE', #23261 ) ;
#32678 = CARTESIAN_POINT ( 'NONE',  ( 115.2940338803257703, -299.5541904835127980, -195.3611179825600175 ) ) ;
#32679 = CARTESIAN_POINT ( 'NONE',  ( -39.95528097930107236, -290.1653046653184447, -343.6734138299510164 ) ) ;
#32680 = CARTESIAN_POINT ( 'NONE',  ( 15.57720452528313615, -288.5486078092118305, -215.8307269825707806 ) ) ;
#32681 = CARTESIAN_POINT ( 'NONE',  ( -78.23830235994276450, -288.9666328197043867, -331.0138154508651951 ) ) ;
#32682 = CARTESIAN_POINT ( 'NONE',  ( 12.04288400302199236, -286.2249774361969799, -211.2942224539150118 ) ) ;
#32683 = CARTESIAN_POINT ( 'NONE',  ( -18.20453976106250948, -63.49190233628851132, -22.50000000000000000 ) ) ;
#32684 = CARTESIAN_POINT ( 'NONE',  ( 34.71717841895296885, -280.1599667270440932, -286.2971915320982248 ) ) ;
#32685 = CARTESIAN_POINT ( 'NONE',  ( 31.09138531498125957, -289.0313554288577507, -241.4569604033299015 ) ) ;
#32686 = CARTESIAN_POINT ( 'NONE',  ( -74.15982291388664294, -282.0304562259884165, -334.2560491917651007 ) ) ;
#32687 = CARTESIAN_POINT ( 'NONE',  ( -108.0976141132162383, -280.1287721598358758, -250.4437513797489601 ) ) ;
#32688 = CARTESIAN_POINT ( 'NONE',  ( 39.11417577550911773, -288.5796958911892034, -277.2400170453149144 ) ) ;
#32689 = CARTESIAN_POINT ( 'NONE',  ( -72.86644624274327953, -278.0286605184971336, -334.2189201317901848 ) ) ;
#32690 = CARTESIAN_POINT ( 'NONE',  ( -113.8554361869827147, -289.3006209270952809, -274.0566439086643982 ) ) ;
#32691 = CARTESIAN_POINT ( 'NONE',  ( -101.2790848122431697, -284.7918001381394788, -313.0731113635339966 ) ) ;
#32692 = CARTESIAN_POINT ( 'NONE',  ( -10.02168170507467870, -286.8916785981275552, -198.3797964384549743 ) ) ;
#32693 = CARTESIAN_POINT ( 'NONE',  ( -58.94610623450461162, -283.5061290872394011, -340.1440924515371762 ) ) ;
#32694 = ORIENTED_EDGE ( 'NONE', *, *, #75975, .F. ) ;
#32695 = CARTESIAN_POINT ( 'NONE',  ( 207.4724402404594343, 29.73442829110639352, 14.90057469441957672 ) ) ;
#32696 = CARTESIAN_POINT ( 'NONE',  ( -111.9132769292164227, -292.2413997197231765, -283.8277560848690655 ) ) ;
#32697 = CARTESIAN_POINT ( 'NONE',  ( 19.15413177870801320, -292.9436305070307753, -322.0281775360701886 ) ) ;
#32698 = CARTESIAN_POINT ( 'NONE',  ( 33.46663503010690022, -274.8569971919787918, -289.0583937417505922 ) ) ;
#32699 = CARTESIAN_POINT ( 'NONE',  ( -110.2517025824968471, -295.5925449256187107, -294.8037923163639107 ) ) ;
#32700 = CARTESIAN_POINT ( 'NONE',  ( -22.58303012936103826, -290.7243881366661640, -198.1607758059705020 ) ) ;
#32701 = CARTESIAN_POINT ( 'NONE',  ( -23.34892642947344399, -293.1107942557617889, -343.0920182071574231 ) ) ;
#32702 = CARTESIAN_POINT ( 'NONE',  ( -110.6431755441068532, -291.8180519338893077, -265.7257515580950553 ) ) ;
#32703 = CARTESIAN_POINT ( 'NONE',  ( 138.6539576904058606, 250.0000000000000568, 12.50000000000000000 ) ) ;
#32704 = CARTESIAN_POINT ( 'NONE',  ( 36.52837220358623682, -291.3739008384073941, -256.4600085735470429 ) ) ;
#32705 = CARTESIAN_POINT ( 'NONE',  ( 31.16687527362607923, -295.9537693457886576, -301.0088487393136916 ) ) ;
#32706 = CARTESIAN_POINT ( 'NONE',  ( 34.99350743265259212, -288.6449753292862965, -281.8877846085155170 ) ) ;
#32707 = CARTESIAN_POINT ( 'NONE',  ( 19.59440823066776005, -278.2137872534224812, -319.7434591597016151 ) ) ;
#32708 = CARTESIAN_POINT ( 'NONE',  ( -56.83786395635641497, -276.0929264183029090, -344.4963078425350318 ) ) ;
#32709 = ADVANCED_FACE ( 'NONE', ( #60657 ), #26434, .T. ) ;
#32710 = CARTESIAN_POINT ( 'NONE',  ( -91.51442520256379964, -296.5014636604155385, -215.8682314903987276 ) ) ;
#32711 = CARTESIAN_POINT ( 'NONE',  ( 18.18075961690786713, -274.4815289224268895, -319.3213225810429776 ) ) ;
#32712 = CARTESIAN_POINT ( 'NONE',  ( -19.15962067499798849, -278.3676429771831522, -198.1224316850475589 ) ) ;
#32713 = CARTESIAN_POINT ( 'NONE',  ( 33.97598714308885803, -276.9854976929820509, -287.7610961014028135 ) ) ;
#32714 = CARTESIAN_POINT ( 'NONE',  ( -42.76973140434803611, -275.5194496314200023, -346.3675446327143277 ) ) ;
#32715 = FACE_OUTER_BOUND ( 'NONE', #78909, .T. ) ;
#32716 = CARTESIAN_POINT ( 'NONE',  ( -33.81255125181687760, -298.9002774137236997, -197.1991438378180703 ) ) ;
#32717 = DIRECTION ( 'NONE',  ( -0.000000000000000000, -0.000000000000000000, -1.000000000000000000 ) ) ;
#32719 = CARTESIAN_POINT ( 'NONE',  ( -31.33759439226609800, -273.9633785012337626, -197.5958002610799156 ) ) ;
#32718 = CARTESIAN_POINT ( 'NONE',  ( 9.192011959814715638, -286.4372534842286768, -329.6982213110718476 ) ) ;
#32720 = CARTESIAN_POINT ( 'NONE',  ( 35.84903297082797735, -287.2492998703770581, -246.2716405601228189 ) ) ;
#32721 = CARTESIAN_POINT ( 'NONE',  ( -45.96717373674685803, -299.9231724059632143, -195.5011954164149870 ) ) ;
#32722 = CARTESIAN_POINT ( 'NONE',  ( -94.11917273739189227, -295.2291774508144613, -221.5936262951379661 ) ) ;
#32723 = CARTESIAN_POINT ( 'NONE',  ( 6.101395986104649616, -279.8226124486786830, -206.9824447548156172 ) ) ;
#32724 = DIRECTION ( 'NONE',  ( -1.000000000000000000, 0.000000000000000000, 0.000000000000000000 ) ) ;
#32725 = CARTESIAN_POINT ( 'NONE',  ( -10.41089955328140881, -278.4032439015824139, -200.3082946097797787 ) ) ;
#32726 = DIRECTION ( 'NONE',  ( -1.000000000000000000, 0.000000000000000000, 0.000000000000000000 ) ) ;
#32727 = CARTESIAN_POINT ( 'NONE',  ( -109.0539615864481959, -289.1412154093627578, -286.0555242936515015 ) ) ;
#32728 = CARTESIAN_POINT ( 'NONE',  ( 208.4306832106271088, 0.000000000000000000, -7.500000000000012434 ) ) ;
#32729 = CARTESIAN_POINT ( 'NONE',  ( -68.61247857462009847, -289.6410736226715130, -202.1770821698003431 ) ) ;
#32730 = CARTESIAN_POINT ( 'NONE',  ( -57.06563122903368424, -275.3133373570557296, -199.3031485292505920 ) ) ;
#32731 = CARTESIAN_POINT ( 'NONE',  ( -27.43040745016602244, -284.3539821233872544, -346.1793180783183175 ) ) ;
#32732 = CARTESIAN_POINT ( 'NONE',  ( -98.38890591690906717, -271.2352666404831325, -225.7485269746892982 ) ) ;
#32733 = CARTESIAN_POINT ( 'NONE',  ( -63.53326811574574862, -275.1292870704504594, -201.5770503216591294 ) ) ;
#32734 = CARTESIAN_POINT ( 'NONE',  ( -36.74500083477536805, -274.8626726804567397, -197.1896319917300389 ) ) ;
#32735 = CARTESIAN_POINT ( 'NONE',  ( -16.66803297545346751, -284.7853767115535675, -342.5093573545170216 ) ) ;
#32736 = CARTESIAN_POINT ( 'NONE',  ( -87.53497357235173126, -272.2523024649440231, -216.8607253488772528 ) ) ;
#32737 = EDGE_LOOP ( 'NONE', ( #48032, #60302, #85533, #83482 ) ) ;
#32738 = CARTESIAN_POINT ( 'NONE',  ( 204.2025551593094121, 295.5631162206468048, -54.00000000005014300 ) ) ;
#32739 = CARTESIAN_POINT ( 'NONE',  ( 37.09602283697132208, -293.6320802033485506, -290.0594784296054627 ) ) ;
#32740 = CARTESIAN_POINT ( 'NONE',  ( -108.9396684218322804, -286.8072870316539706, -249.0729263399446722 ) ) ;
#32741 = DIRECTION ( 'NONE',  ( 0.000000000000000000, 0.000000000000000000, 1.000000000000000000 ) ) ;
#32742 = CARTESIAN_POINT ( 'NONE',  ( 40.64545035920995986, -273.2666405000204009, -288.1938231032136741 ) ) ;
#32743 = CARTESIAN_POINT ( 'NONE',  ( -109.5884415500002831, -277.4164148835582751, -296.6810596739367725 ) ) ;
#32744 = ADVANCED_FACE ( 'NONE', ( #73916 ), #9033, .T. ) ;
#32745 = CARTESIAN_POINT ( 'NONE',  ( -113.5680287832200719, -288.9773741573943084, -268.3552243968866264 ) ) ;
#32746 = CARTESIAN_POINT ( 'NONE',  ( -0.8923988824507324003, -284.0788635948879346, -334.4091951720478164 ) ) ;
#32747 = CARTESIAN_POINT ( 'NONE',  ( -29.58524501423735131, -278.7128792920361207, -344.0185153731196692 ) ) ;
#32748 = CARTESIAN_POINT ( 'NONE',  ( -95.38098671520711491, -286.6538465493970875, -220.5821669827580251 ) ) ;
#32749 = CARTESIAN_POINT ( 'NONE',  ( 20.35890362660326502, -282.8906745624727819, -222.4283470015218427 ) ) ;
#32750 = CARTESIAN_POINT ( 'NONE',  ( 4.861386396898944362, -274.7716542881061628, -205.8936689348984146 ) ) ;
#32751 = CARTESIAN_POINT ( 'NONE',  ( -87.09681114658178558, -277.5560523220985374, -329.1967657142477606 ) ) ;
#32752 = CARTESIAN_POINT ( 'NONE',  ( -83.22861867451176465, -297.6059734263096743, -329.0417079162932623 ) ) ;
#32753 = CARTESIAN_POINT ( 'NONE',  ( -35.09237171215954731, -122.5496321078137356, 21.50000000000000000 ) ) ;
#32754 = DIRECTION ( 'NONE',  ( 1.000000000000000000, 0.000000000000000000, 0.000000000000000000 ) ) ;
#32755 = CARTESIAN_POINT ( 'NONE',  ( -35.83451943785929927, -296.2104197581550693, -194.5967821684023704 ) ) ;
#32756 = CARTESIAN_POINT ( 'NONE',  ( -110.4535370110471462, -278.0562309456329899, -270.6320298648365110 ) ) ;
#32757 = CARTESIAN_POINT ( 'NONE',  ( -49.67053651609517573, -275.1034798830269779, -194.7032998507759203 ) ) ;
#32758 = CARTESIAN_POINT ( 'NONE',  ( 17.62840567704764183, -288.6121324885496620, -220.7815193943803536 ) ) ;
#32759 = CARTESIAN_POINT ( 'NONE',  ( -103.9878321598168327, -297.5848638617578104, -307.6309074458534951 ) ) ;
#32760 = CARTESIAN_POINT ( 'NONE',  ( -34.85209762121945687, -296.2265970318481436, -346.9235800576190627 ) ) ;
#32761 = CARTESIAN_POINT ( 'NONE',  ( -95.73714348387795781, -293.1976446500661382, -223.5433050743689591 ) ) ;
#32762 = CARTESIAN_POINT ( 'NONE',  ( -82.37124065772339065, -277.4361608060952449, -210.5267691309406359 ) ) ;
#32763 = CARTESIAN_POINT ( 'NONE',  ( 30.27056421462915026, -283.0588207185207352, -239.0945237478530316 ) ) ;
#32764 = CARTESIAN_POINT ( 'NONE',  ( -41.93320808914626951, -296.0736790091700641, -196.0628525008749534 ) ) ;
#32765 = CARTESIAN_POINT ( 'NONE',  ( -38.68648037173607435, -284.9292604148132568, -346.1139862449836642 ) ) ;
#32766 = CARTESIAN_POINT ( 'NONE',  ( 35.75898745660029476, -286.5533904706117028, -276.5209368664935710 ) ) ;
#32767 = CARTESIAN_POINT ( 'NONE',  ( -110.3273273839884610, -271.8591574644645448, -296.2092911942687010 ) ) ;
#32768 = ORIENTED_EDGE ( 'NONE', *, *, #62017, .F. ) ;
#32769 = CARTESIAN_POINT ( 'NONE',  ( -17.16196182006822113, -285.9865137319845303, -200.1308670104079397 ) ) ;
#32770 = ORIENTED_EDGE ( 'NONE', *, *, #27512, .T. ) ;
#32771 = CARTESIAN_POINT ( 'NONE',  ( -38.71317819491038392, -284.1486422036933845, -347.0397431585845993 ) ) ;
#32772 = CARTESIAN_POINT ( 'NONE',  ( -109.9072526409043036, -272.9928396826201720, -262.2169129720123806 ) ) ;
#32773 = CARTESIAN_POINT ( 'NONE',  ( 33.49811567641476984, -285.9731660756377210, -241.0723588670986999 ) ) ;
#32774 = CARTESIAN_POINT ( 'NONE',  ( 18.97935819681732639, -281.7806702549289071, -218.2002264816921411 ) ) ;
#32775 = CARTESIAN_POINT ( 'NONE',  ( 196.5860305738692944, 20.47868439449646161, -13.00974972892932691 ) ) ;
#32776 = CARTESIAN_POINT ( 'NONE',  ( -111.4175745230541850, -280.3040947252583805, -251.9915418739947484 ) ) ;
#32777 = CARTESIAN_POINT ( 'NONE',  ( 32.00057492710987361, -281.4550965857262099, -236.8110679369113996 ) ) ;
#32778 = CARTESIAN_POINT ( 'NONE',  ( -37.30987171927208834, -283.5523547857346784, -200.3611179825600459 ) ) ;
#32779 = CARTESIAN_POINT ( 'NONE',  ( 85.34974711902751210, 82.93338734745742613, -302.3957557721062699 ) ) ;
#32780 = ORIENTED_EDGE ( 'NONE', *, *, #59618, .T. ) ;
#32781 = CARTESIAN_POINT ( 'NONE',  ( 37.41704493807935705, -277.4962935497120498, -266.0075450164081303 ) ) ;
#32782 = CARTESIAN_POINT ( 'NONE',  ( -78.55901433422972957, -208.1269654894091161, -356.8488242329224818 ) ) ;
#32783 = CARTESIAN_POINT ( 'NONE',  ( 19.73613809064724833, -280.2407817075410890, -318.4846638550416174 ) ) ;
#32784 = CARTESIAN_POINT ( 'NONE',  ( 19.60421918333060987, -294.6216950314292262, -220.0310675260219284 ) ) ;
#32785 = CARTESIAN_POINT ( 'NONE',  ( -109.4648368559871017, -295.7436780642699432, -282.2836100399914585 ) ) ;
#32786 = CARTESIAN_POINT ( 'NONE',  ( -2.078451881527334510, -292.0139868680623181, -201.9648466246572127 ) ) ;
#32787 = CARTESIAN_POINT ( 'NONE',  ( 184.7149167944524493, 8.542400036368780647, -9.000000000000001776 ) ) ;
#32789 = CARTESIAN_POINT ( 'NONE',  ( 35.35903407656502395, -285.7826613046892135, -257.3821092042276746 ) ) ;
#32788 = CARTESIAN_POINT ( 'NONE',  ( -99.53953502503475192, -294.5334267876225454, -314.8353484836579810 ) ) ;
#32790 = CARTESIAN_POINT ( 'NONE',  ( 33.94281058225051595, -295.6826424963398381, -291.1284417734622139 ) ) ;
#32791 = CARTESIAN_POINT ( 'NONE',  ( -107.0051002545059333, -286.1781570310841403, -246.7868294666612883 ) ) ;
#32792 = CARTESIAN_POINT ( 'NONE',  ( 23.78058699239112173, -293.8723600156076259, -223.8972019567250413 ) ) ;
#32793 = CARTESIAN_POINT ( 'NONE',  ( -109.5582071353410356, -284.8941864146328840, -281.7654377168906308 ) ) ;
#32794 = CARTESIAN_POINT ( 'NONE',  ( -69.37592593356716009, -294.2592907575341883, -339.9586450198791567 ) ) ;
#32795 = CARTESIAN_POINT ( 'NONE',  ( -112.9725432089030335, -291.1839872414853971, -284.0049950115785578 ) ) ;
#32796 = CARTESIAN_POINT ( 'NONE',  ( -90.74773663520244327, -291.8118055955172281, -214.9037604585546148 ) ) ;
#32797 = CARTESIAN_POINT ( 'NONE',  ( -73.54311925351944979, -289.7135556041953350, -333.7668319371736629 ) ) ;
#32798 = ORIENTED_EDGE ( 'NONE', *, *, #64884, .F. ) ;
#32799 = LINE ( 'NONE', #90984, #60892 ) ;
#32800 = CARTESIAN_POINT ( 'NONE',  ( -33.43809796967462944, -299.9609350218637474, -194.5950889648607358 ) ) ;
#32801 = CARTESIAN_POINT ( 'NONE',  ( -21.42225531884626477, -273.0468653608984368, -195.4306168869844953 ) ) ;
#32802 = CARTESIAN_POINT ( 'NONE',  ( 7.295195307877241575, -279.7361149232996809, -212.2370119380635458 ) ) ;
#32803 = CARTESIAN_POINT ( 'NONE',  ( 18.04965236476250112, -274.3274023508747064, -216.8868334919154677 ) ) ;
#32804 = CARTESIAN_POINT ( 'NONE',  ( -77.87734818954048421, -295.9769508176643171, -208.7565794703882318 ) ) ;
#32805 = CARTESIAN_POINT ( 'NONE',  ( -83.76098006036900756, -279.5571295005846082, -328.3592544500821759 ) ) ;
#32806 = CARTESIAN_POINT ( 'NONE',  ( -1.099232556023643337, -272.6780476209133326, -205.5596091420736400 ) ) ;
#32807 = CARTESIAN_POINT ( 'NONE',  ( -110.7811908363420059, -297.7424968122513178, -271.4844253147840618 ) ) ;
#32808 = CARTESIAN_POINT ( 'NONE',  ( -109.4436631883412332, -297.4568765994258683, -283.6794746251381412 ) ) ;
#32809 = DIRECTION ( 'NONE',  ( -1.000000000000000000, 0.000000000000000000, 0.000000000000000000 ) ) ;
#32810 = CARTESIAN_POINT ( 'NONE',  ( -96.73573769918829157, -298.7987109146243370, -222.6244578587956369 ) ) ;
#32811 = CARTESIAN_POINT ( 'NONE',  ( -15.45078558823529669, -296.3254154660327231, -195.2018851504046779 ) ) ;
#32812 = CARTESIAN_POINT ( 'NONE',  ( 6.130207696522662175, -295.0962149306045035, -329.1956788084126515 ) ) ;
#32813 = CARTESIAN_POINT ( 'NONE',  ( 21.47560178783512086, -291.5108351405484655, -226.1355607345328167 ) ) ;
#32814 = CARTESIAN_POINT ( 'NONE',  ( 209.5027106082920056, 29.50523358103493621, 14.69807322781335834 ) ) ;
#32815 = CARTESIAN_POINT ( 'NONE',  ( 13.91880144552290766, -275.2406749740655982, -212.9149523058738396 ) ) ;
#32816 = CARTESIAN_POINT ( 'NONE',  ( -33.81508741270545926, -298.4307796347532644, -197.3397675358135075 ) ) ;
#32817 = CARTESIAN_POINT ( 'NONE',  ( -1.142926231357398237, -284.5542307995082751, -336.4670071600247070 ) ) ;
#32818 = CARTESIAN_POINT ( 'NONE',  ( -55.60081723594127823, -281.9672368499194590, -344.6571670960450433 ) ) ;
#32819 = CARTESIAN_POINT ( 'NONE',  ( 3.440400404170164794, -275.8681050273172559, -335.6168395218352316 ) ) ;
#32820 = DIRECTION ( 'NONE',  ( 0.000000000000000000, 0.000000000000000000, 1.000000000000000000 ) ) ;
#32821 = CARTESIAN_POINT ( 'NONE',  ( -56.37072695869962757, -282.5008803965488937, -341.0045739027429477 ) ) ;
#32822 = CARTESIAN_POINT ( 'NONE',  ( 25.18243166846312775, -280.1146008824209162, -312.0835504337774751 ) ) ;
#32823 = CARTESIAN_POINT ( 'NONE',  ( 35.20961297883029317, -273.9647282484440893, -257.9702451927489619 ) ) ;
#32824 = CARTESIAN_POINT ( 'NONE',  ( -111.3020683139406373, -280.7130718518005210, -257.8408025537938784 ) ) ;
#32825 = B_SPLINE_CURVE_WITH_KNOTS ( 'NONE', 3,
 ( #77497, #12644, #77982, #21134, #41489, #28255, #70872, #42430, #48126, #78443 ),
 .UNSPECIFIED., .F., .F.,
 ( 4, 2, 2, 2, 4 ),
 ( -1.095445519328078919E-05, 0.001993413916517096894, 0.002494506009444676011, 0.002995598102372255128, 0.003997782288227412495 ),
 .UNSPECIFIED. ) ;
#32826 = CARTESIAN_POINT ( 'NONE',  ( 196.0143093133015384, 73.40565171261609123, 11.99999999999998757 ) ) ;
#32827 = CARTESIAN_POINT ( 'NONE',  ( 52.66432107828247666, -260.8771019122912094, -465.6442049081569508 ) ) ;
#32828 = CARTESIAN_POINT ( 'NONE',  ( -63.26557735654754566, -272.1198406178012874, -198.7064391107515746 ) ) ;
#32829 = CARTESIAN_POINT ( 'NONE',  ( -94.73252445600395788, -279.8821134031131237, -318.9229339386325250 ) ) ;
#32830 = LINE ( 'NONE', #90552, #13601 ) ;
#32831 = CARTESIAN_POINT ( 'NONE',  ( -110.4749258510289422, -286.2294267523125200, -289.4082818517500186 ) ) ;
#32832 = ORIENTED_EDGE ( 'NONE', *, *, #27099, .F. ) ;
#32833 = CARTESIAN_POINT ( 'NONE',  ( 156.4697130957825095, 16.02030068022343201, -10.01540472299836182 ) ) ;
#32834 = CARTESIAN_POINT ( 'NONE',  ( -8.418478753352225397, -286.6733960011205227, -339.5734022241688308 ) ) ;
#32835 = CARTESIAN_POINT ( 'NONE',  ( 207.3685651567432728, 30.41993118425675036, 14.46441793359390005 ) ) ;
#32836 = CARTESIAN_POINT ( 'NONE',  ( -84.74619556927338238, -294.5172605550152412, -326.4630669486883221 ) ) ;
#32837 = CARTESIAN_POINT ( 'NONE',  ( -12.90321945535889725, -286.8707148162086469, -340.4583799957183032 ) ) ;
#32838 = CARTESIAN_POINT ( 'NONE',  ( -107.8893720497363518, -252.3744610414916565, -325.2219058921743908 ) ) ;
#32839 = CARTESIAN_POINT ( 'NONE',  ( -112.3745884092469964, -294.5737924874119358, -268.6628699735679788 ) ) ;
#32840 = CARTESIAN_POINT ( 'NONE',  ( -36.55297794806401868, -284.5417667913201853, -194.0456032211958188 ) ) ;
#32841 = CARTESIAN_POINT ( 'NONE',  ( -14.07578509605410666, -281.9590349963796712, -200.2704108289871954 ) ) ;
#32842 = CARTESIAN_POINT ( 'NONE',  ( -100.5883263543587844, -282.2292397523884802, -312.5725292539780185 ) ) ;
#32843 = CARTESIAN_POINT ( 'NONE',  ( 16.01096319219574582, -288.2694432291956446, -320.2597071249346641 ) ) ;
#32844 = CARTESIAN_POINT ( 'NONE',  ( -93.55193220931684550, -280.6471505415067327, -222.8466261922679053 ) ) ;
#32845 = CARTESIAN_POINT ( 'NONE',  ( 15.36863879043039560, -281.6233061980023535, -219.5519667075348593 ) ) ;
#32846 = EDGE_CURVE ( 'NONE', #33034, #42343, #75779, .T. ) ;
#32847 = CARTESIAN_POINT ( 'NONE',  ( 4.661860201572728180, -290.4680066554457767, -332.9239481646301897 ) ) ;
#32848 = ORIENTED_EDGE ( 'NONE', *, *, #72944, .T. ) ;
#32849 = CARTESIAN_POINT ( 'NONE',  ( -90.16285924102847105, -273.3302529751937868, -214.2621941111483181 ) ) ;
#32850 = CARTESIAN_POINT ( 'NONE',  ( -110.2642716376925591, -292.3256672490841765, -286.3623808589996997 ) ) ;
#32851 = DIRECTION ( 'NONE',  ( 0.000000000000000000, 0.000000000000000000, -1.000000000000000000 ) ) ;
#32852 = CARTESIAN_POINT ( 'NONE',  ( -55.56934967048406548, -297.7662352645559167, -350.3683826091709648 ) ) ;
#32853 = VERTEX_POINT ( 'NONE', #37911 ) ;
#32854 = CARTESIAN_POINT ( 'NONE',  ( 21.19680668337102958, -274.1995948451560707, -317.5330495790701093 ) ) ;
#32855 = CARTESIAN_POINT ( 'NONE',  ( 198.7796172868510496, 65.30644135522835825, 10.61564514751593791 ) ) ;
#32856 = CARTESIAN_POINT ( 'NONE',  ( -67.92400455736233766, -293.8468436901030145, -340.1548359867680915 ) ) ;
#32857 = CARTESIAN_POINT ( 'NONE',  ( 5.242850644267413429, -273.9936478771248858, -210.8809696933471969 ) ) ;
#32858 = CARTESIAN_POINT ( 'NONE',  ( 26.30453471381903441, -289.5785226112020609, -307.6085722133709623 ) ) ;
#32859 = CARTESIAN_POINT ( 'NONE',  ( 18.38236746969534252, -283.9977485967817756, -319.0725366169236850 ) ) ;
#32860 = CARTESIAN_POINT ( 'NONE',  ( -113.4219892818600783, -292.0737960958622352, -262.7141145182393984 ) ) ;
#32861 = CARTESIAN_POINT ( 'NONE',  ( -81.65843981301547672, -292.7777780252258708, -207.9966661266957999 ) ) ;
#32862 = CARTESIAN_POINT ( 'NONE',  ( -32.15516723932170606, -291.9526794001114354, -197.5329781575705965 ) ) ;
#32863 = CARTESIAN_POINT ( 'NONE',  ( -102.7476271547374296, -287.0423280085199167, -233.5522329158753791 ) ) ;
#32864 = CARTESIAN_POINT ( 'NONE',  ( 8.544836518185610075, -280.8276896247477907, -208.4609840811428114 ) ) ;
#32865 = CARTESIAN_POINT ( 'NONE',  ( -93.59616042685664183, -293.9343861330013397, -320.8259167351917540 ) ) ;
#32866 = CARTESIAN_POINT ( 'NONE',  ( -24.53567159286675903, -282.7264971892649896, -346.3428679147873481 ) ) ;
#32867 = CARTESIAN_POINT ( 'NONE',  ( 35.32566966056675284, -277.2148960827357769, -255.1228946097576795 ) ) ;
#32868 = ADVANCED_FACE ( 'NONE', ( #60194 ), #68690, .T. ) ;
#32869 = CARTESIAN_POINT ( 'NONE',  ( 27.36219212280431989, -290.4805209788416391, -301.4846348637938149 ) ) ;
#32870 = CARTESIAN_POINT ( 'NONE',  ( -23.19317750634681730, -275.0127936719401873, -344.8464457043886000 ) ) ;
#32871 = DIRECTION ( 'NONE',  ( 0.000000000000000000, 0.000000000000000000, 1.000000000000000000 ) ) ;
#32872 = CARTESIAN_POINT ( 'NONE',  ( -70.24825271200126053, -283.0055782943686609, -335.6065984688368644 ) ) ;
#32873 = CARTESIAN_POINT ( 'NONE',  ( -103.0787761271877230, -280.2738394017300720, -230.9305307229744244 ) ) ;
#32874 = CARTESIAN_POINT ( 'NONE',  ( 33.81969193680325958, -286.9791436470911776, -299.2928649801286838 ) ) ;
#32875 = CARTESIAN_POINT ( 'NONE',  ( -38.94164880246820104, -293.7919499286405198, -196.3650763302414930 ) ) ;
#32876 = CARTESIAN_POINT ( 'NONE',  ( 38.75411320653979885, -277.0904747896923368, -265.4706009359164796 ) ) ;
#32877 = CARTESIAN_POINT ( 'NONE',  ( 23.98247542316440573, -277.4797586216487275, -316.1065414365120319 ) ) ;
#32878 = CARTESIAN_POINT ( 'NONE',  ( -106.2649104874848831, -278.0636821907446574, -294.5683552148326498 ) ) ;
#32879 = CARTESIAN_POINT ( 'NONE',  ( -35.79291522040858808, -300.0717403666205882, -195.5272464029587240 ) ) ;
#32880 = CARTESIAN_POINT ( 'NONE',  ( -63.17237257271649042, -283.7149093589713402, -200.0719348275429468 ) ) ;
#32881 = CARTESIAN_POINT ( 'NONE',  ( -2.061745773593721243, -292.1730271632944209, -201.9280050367528645 ) ) ;
#32882 = CARTESIAN_POINT ( 'NONE',  ( 28.22585110764876504, -289.6633859786339258, -309.1855515133631229 ) ) ;
#32883 = CARTESIAN_POINT ( 'NONE',  ( 36.01723295166004135, -292.4779153790240116, -270.7753333347918669 ) ) ;
#32884 = ORIENTED_EDGE ( 'NONE', *, *, #57901, .F. ) ;
#32885 = EDGE_CURVE ( 'NONE', #43403, #29794, #41418, .T. ) ;
#32886 = CARTESIAN_POINT ( 'NONE',  ( -64.16482900053965466, -290.2838308103768554, -198.7573126711144198 ) ) ;
#32887 = CARTESIAN_POINT ( 'NONE',  ( -9.715543979829012855, -292.0898342371773992, -202.7138029605008853 ) ) ;
#32888 = ORIENTED_EDGE ( 'NONE', *, *, #43122, .T. ) ;
#32889 = CARTESIAN_POINT ( 'NONE',  ( -4.453108471476115326, -289.7085324850863799, -339.6563682527219044 ) ) ;
#32890 = CARTESIAN_POINT ( 'NONE',  ( -95.63119207124971410, -279.5033083319034972, -226.3582899885431061 ) ) ;
#32891 = CARTESIAN_POINT ( 'NONE',  ( -97.98106593156762756, -296.1020592677214154, -223.3893188395267657 ) ) ;
#32892 = CARTESIAN_POINT ( 'NONE',  ( -46.50159475958982114, -286.5902049458972556, -194.0105507498423094 ) ) ;
#32893 = CARTESIAN_POINT ( 'NONE',  ( -20.99259590879864845, -286.5897177621790206, -195.1384413307527552 ) ) ;
#32894 = CARTESIAN_POINT ( 'NONE',  ( -78.38501105099166466, -283.9548810786728836, -330.7559365947181504 ) ) ;
#32895 = CARTESIAN_POINT ( 'NONE',  ( -113.9562875489731653, -273.5685593820227837, -284.1604309951135861 ) ) ;
#32896 = CARTESIAN_POINT ( 'NONE',  ( 152.1864817686872868, 207.0855559507159853, -216.2993369928966274 ) ) ;
#32897 = CARTESIAN_POINT ( 'NONE',  ( 102.3144949715192240, 114.9274731801767331, -279.5273309297857054 ) ) ;
#32898 = CARTESIAN_POINT ( 'NONE',  ( 5.279096791983114656, -273.8422528797663631, -210.8336381429203925 ) ) ;
#32899 = CARTESIAN_POINT ( 'NONE',  ( 3.294073093163292665, -275.4120145335326129, -331.3771815049728389 ) ) ;
#32900 = CARTESIAN_POINT ( 'NONE',  ( -105.1963761121639465, -296.5301306658017779, -233.9814681441946504 ) ) ;
#32901 = CARTESIAN_POINT ( 'NONE',  ( 190.2888855011954945, 268.0502169937788040, -137.8993104347648284 ) ) ;
#32902 = CARTESIAN_POINT ( 'NONE',  ( 38.43803421264869513, -274.1045306193429383, -259.8382792094398042 ) ) ;
#32903 = CARTESIAN_POINT ( 'NONE',  ( -110.1303768051990346, -274.4903250376994492, -256.6782261879677662 ) ) ;
#32904 = ORIENTED_EDGE ( 'NONE', *, *, #49892, .T. ) ;
#32905 = CARTESIAN_POINT ( 'NONE',  ( -94.86377098310568101, -274.3213539501816740, -219.6392895967927643 ) ) ;
#32906 = CARTESIAN_POINT ( 'NONE',  ( -101.6943818429355133, -290.5718705282404812, -305.0620180383345428 ) ) ;
#32907 = CARTESIAN_POINT ( 'NONE',  ( -81.76998556058332213, -296.4427856299671475, -333.1180936335334763 ) ) ;
#32908 = CARTESIAN_POINT ( 'NONE',  ( -48.96688651821023797, -298.4003302111540279, -194.2523696570733023 ) ) ;
#32909 = CARTESIAN_POINT ( 'NONE',  ( -53.14730905675413908, -295.4270384066023780, -341.6814875082871481 ) ) ;
#32910 = EDGE_LOOP ( 'NONE', ( #8854, #17077, #40225, #31872 ) ) ;
#32911 = CARTESIAN_POINT ( 'NONE',  ( -86.14609995477528059, -279.6425506022802097, -328.1135653219418487 ) ) ;
#32912 = CARTESIAN_POINT ( 'NONE',  ( -39.57918236722738925, -279.5324500610237806, -193.4421573521956361 ) ) ;
#32913 = CARTESIAN_POINT ( 'NONE',  ( 5.544245583410889466, -277.3968768583897599, -329.7887557370479499 ) ) ;
#32914 = CARTESIAN_POINT ( 'NONE',  ( -4.413416606285027299, -278.3843189159451867, -338.8568285454893498 ) ) ;
#32915 = CARTESIAN_POINT ( 'NONE',  ( -110.8848032877358918, -276.3623491326079602, -286.7872795933438965 ) ) ;
#32916 = CARTESIAN_POINT ( 'NONE',  ( -68.31436617887244722, -274.1263777170876779, -204.1757949561956309 ) ) ;
#32917 = CARTESIAN_POINT ( 'NONE',  ( -103.8223008511671992, -271.4580207823357227, -238.5643024504222467 ) ) ;
#32918 = DIRECTION ( 'NONE',  ( 1.000000000000000000, 0.000000000000000000, 0.000000000000000000 ) ) ;
#32919 = CARTESIAN_POINT ( 'NONE',  ( -110.3512522342016382, -278.7511626175920014, -267.9103805241133500 ) ) ;
#32920 = CARTESIAN_POINT ( 'NONE',  ( 2.906367770195225742, -287.2091512239007329, -335.4877739259253531 ) ) ;
#32921 = CARTESIAN_POINT ( 'NONE',  ( -82.39943295479227459, -275.4376479941607840, -210.3394393060066818 ) ) ;
#32922 = DIRECTION ( 'NONE',  ( 1.000000000000000000, 0.000000000000000000, 0.000000000000000000 ) ) ;
#32923 = CARTESIAN_POINT ( 'NONE',  ( -109.3396425958786864, -289.5782552270793531, -283.3571946096433862 ) ) ;
#32924 = CARTESIAN_POINT ( 'NONE',  ( -105.6973469637469947, -283.4448292127206059, -305.7025755731332879 ) ) ;
#32925 = CARTESIAN_POINT ( 'NONE',  ( 33.19024411569889565, -280.0873258821627019, -292.9604114228595790 ) ) ;
#32927 = CARTESIAN_POINT ( 'NONE',  ( -103.5073756568267527, -283.0867316973655647, -236.2522103950360020 ) ) ;
#32926 = CARTESIAN_POINT ( 'NONE',  ( 19.30117814593473113, -279.4657959588715244, -223.3632693802757956 ) ) ;
#32928 = CARTESIAN_POINT ( 'NONE',  ( 36.94504401476538646, -289.6894933170121362, -281.0449711320229085 ) ) ;
#32929 = CARTESIAN_POINT ( 'NONE',  ( -95.11285719183571530, -280.3922774516108234, -225.0681107466438675 ) ) ;
#32930 = CARTESIAN_POINT ( 'NONE',  ( 187.8995604928813918, 43.86402690510830382, 10.50000000000000000 ) ) ;
#32931 = CARTESIAN_POINT ( 'NONE',  ( 17.92422182340621006, -294.8440684992285128, -219.6592588409577900 ) ) ;
#32932 = CARTESIAN_POINT ( 'NONE',  ( -83.92776260473499406, -277.6624315775244440, -210.2636143687693959 ) ) ;
#32933 = CARTESIAN_POINT ( 'NONE',  ( 17.51721007319650525, -276.8926937547817602, -318.6955577907584143 ) ) ;
#32934 = CARTESIAN_POINT ( 'NONE',  ( -8.712978146998754170, -284.6787398160598173, -339.9175775362199374 ) ) ;
#32935 = DIRECTION ( 'NONE',  ( 0.000000000000000000, 0.000000000000000000, 1.000000000000000000 ) ) ;
#32936 = CARTESIAN_POINT ( 'NONE',  ( -36.08578499355250102, -290.9567033222818964, -345.9235485338659259 ) ) ;
#32937 = CARTESIAN_POINT ( 'NONE',  ( -108.4941548511755656, -294.2436177375766988, -294.2359434081013205 ) ) ;
#32938 = CARTESIAN_POINT ( 'NONE',  ( 9.719935063024131239, -285.8786858023773902, -209.6210050987575926 ) ) ;
#32939 = CARTESIAN_POINT ( 'NONE',  ( -103.1133941752558059, -289.4030812291434813, -236.7738166486678608 ) ) ;
#32940 = CARTESIAN_POINT ( 'NONE',  ( 209.0350460744446934, 30.15816704241420609, 14.26380412667063524 ) ) ;
#32941 = CARTESIAN_POINT ( 'NONE',  ( 33.36778002442193269, -274.5006154486709988, -290.4424249614808673 ) ) ;
#32942 = CARTESIAN_POINT ( 'NONE',  ( 18.89287927942060108, -292.3706590574209372, -318.8422044220893667 ) ) ;
#32943 = DIRECTION ( 'NONE',  ( -1.000000000000000000, -0.000000000000000000, -0.000000000000000000 ) ) ;
#32944 = DIRECTION ( 'NONE',  ( 0.000000000000000000, 0.000000000000000000, -1.000000000000000000 ) ) ;
#32945 = CARTESIAN_POINT ( 'NONE',  ( -99.45531900679264936, -289.6244687465124912, -226.0372406331803745 ) ) ;
#32946 = CARTESIAN_POINT ( 'NONE',  ( -62.85839590947979616, -287.3146177171687441, -201.0582291742840368 ) ) ;
#32947 = CARTESIAN_POINT ( 'NONE',  ( 19.79593539477374620, -286.4789882025795009, -320.4732734816473680 ) ) ;
#32948 = CARTESIAN_POINT ( 'NONE',  ( -84.03564565853366730, -286.8214501959630525, -213.4173926578460794 ) ) ;
#32949 = DIRECTION ( 'NONE',  ( 0.9441124463974853720, 0.2938448091926765815, -0.1493550021521704296 ) ) ;
#32950 = CARTESIAN_POINT ( 'NONE',  ( -5.738135339045852490, -287.2814517793841560, -204.3638485644135301 ) ) ;
#32951 = ADVANCED_FACE ( 'NONE', ( #89973 ), #21796, .T. ) ;
#32952 = CARTESIAN_POINT ( 'NONE',  ( 35.11552575134603416, -295.2663892483308814, -249.6173644755602652 ) ) ;
#32953 = CARTESIAN_POINT ( 'NONE',  ( -51.07533709564728497, -275.3062087946598240, -344.6625406541188568 ) ) ;
#32954 = CARTESIAN_POINT ( 'NONE',  ( 33.00216862118396932, -276.2845747779161911, -301.6258652360431256 ) ) ;
#32955 = CARTESIAN_POINT ( 'NONE',  ( -78.78380549637243746, -289.5787495064606105, -207.1173702057132573 ) ) ;
#32956 = CARTESIAN_POINT ( 'NONE',  ( -112.0859179488524688, -278.7842186739925410, -251.8056194856152956 ) ) ;
#32957 = CARTESIAN_POINT ( 'NONE',  ( -111.7363040177364724, -298.4454714529025523, -277.0720548665729552 ) ) ;
#32958 = CARTESIAN_POINT ( 'NONE',  ( -48.18343439339133027, -267.6589013224570976, -503.9656168148090956 ) ) ;
#32959 = CARTESIAN_POINT ( 'NONE',  ( -110.6395504398199847, -271.5021483123970825, -270.3477634379551660 ) ) ;
#32960 = CARTESIAN_POINT ( 'NONE',  ( -111.4024643768992746, -276.6166089877262948, -276.1520395222280513 ) ) ;
#32961 = CARTESIAN_POINT ( 'NONE',  ( 19.56565204599082364, -278.8748759144665428, -221.4892127096036347 ) ) ;
#32962 = PLANE ( 'NONE',  #72925 ) ;
#32963 = CARTESIAN_POINT ( 'NONE',  ( 38.04765561763470316, -274.1850820714405472, -282.4885207786454657 ) ) ;
#32964 = CARTESIAN_POINT ( 'NONE',  ( -108.2648688222162434, -297.8101774558010106, -290.3764095328523922 ) ) ;
#32965 = CARTESIAN_POINT ( 'NONE',  ( 34.29385124588733191, -280.8205643207123217, -297.7443297823715511 ) ) ;
#32966 = CARTESIAN_POINT ( 'NONE',  ( -63.64233483100957756, -296.3447099166472753, -338.7645706657486926 ) ) ;
#32967 = CARTESIAN_POINT ( 'NONE',  ( -113.7402720745773905, -297.8048544962317123, -275.3241799979437019 ) ) ;
#32968 = CARTESIAN_POINT ( 'NONE',  ( -78.86360831991031262, -273.1422962861992687, -210.2329151852054849 ) ) ;
#32969 = CARTESIAN_POINT ( 'NONE',  ( -34.81472691223120108, -294.0840653066950949, -195.4036963493689711 ) ) ;
#32970 = CARTESIAN_POINT ( 'NONE',  ( 20.28533836702271387, -287.0263233882139389, -219.2126126060300635 ) ) ;
#32971 = CARTESIAN_POINT ( 'NONE',  ( 16.06741504395213482, -274.4445769333790395, -324.1723451437799213 ) ) ;
#32972 = CARTESIAN_POINT ( 'NONE',  ( -3.062638987979901639, -288.4451890818139077, -339.3246112860156813 ) ) ;
#32973 = ADVANCED_FACE ( 'NONE', ( #59738 ), #39765, .F. ) ;
#32974 = CARTESIAN_POINT ( 'NONE',  ( 30.18335542718500619, -286.2301384233865065, -241.8788061238064984 ) ) ;
#32975 = VECTOR ( 'NONE', #34627, 1000.000000000000000 ) ;
#32976 = CARTESIAN_POINT ( 'NONE',  ( -111.8303938710173782, -288.4342144574989675, -279.5337173946844018 ) ) ;
#32977 = ORIENTED_EDGE ( 'NONE', *, *, #20803, .T. ) ;
#32978 = CARTESIAN_POINT ( 'NONE',  ( -92.95696114837319612, -243.2523998898738569, -344.1903318997441374 ) ) ;
#32979 = CARTESIAN_POINT ( 'NONE',  ( 28.28028695021345129, -287.4945350023901369, -302.4818784553601176 ) ) ;
#32980 = DIRECTION ( 'NONE',  ( 0.000000000000000000, 1.000000000000000000, 0.000000000000000000 ) ) ;
#32981 = CARTESIAN_POINT ( 'NONE',  ( -88.15678070623398810, -284.6840561578482038, -327.9703128154546334 ) ) ;
#32982 = CARTESIAN_POINT ( 'NONE',  ( -11.22200553736694850, -291.4429814487121462, -198.1208881312806795 ) ) ;
#32983 = CARTESIAN_POINT ( 'NONE',  ( -9.175955734774754902, -282.0144779793837984, -199.5576487280818299 ) ) ;
#32984 = CARTESIAN_POINT ( 'NONE',  ( -39.58965874748531633, -281.3396790128235239, -193.8743323312287714 ) ) ;
#32985 = CARTESIAN_POINT ( 'NONE',  ( -13.53137171193404065, -282.5676868547491267, -339.4224624954598539 ) ) ;
#32986 = CARTESIAN_POINT ( 'NONE',  ( -48.89136816001263952, -279.1992999834397438, -344.5192820844910102 ) ) ;
#32987 = CARTESIAN_POINT ( 'NONE',  ( -85.21641851755950370, -297.4114365667439870, -210.0534788385164973 ) ) ;
#32988 = CARTESIAN_POINT ( 'NONE',  ( -11.33125291576214266, -275.7133156998286267, -201.5702580775294450 ) ) ;
#32989 = CARTESIAN_POINT ( 'NONE',  ( -75.80603253352713011, -289.5564809184724027, -206.3293692086030262 ) ) ;
#32990 = CARTESIAN_POINT ( 'NONE',  ( -52.68642951383230866, -296.7713645377598368, -198.6238324721507240 ) ) ;
#32991 = ORIENTED_EDGE ( 'NONE', *, *, #9108, .T. ) ;
#32992 = DIRECTION ( 'NONE',  ( 0.000000000000000000, 0.000000000000000000, -1.000000000000000000 ) ) ;
#32993 = CARTESIAN_POINT ( 'NONE',  ( -100.2348288785364048, -285.9314933304451642, -310.2792781458679201 ) ) ;
#32994 = CARTESIAN_POINT ( 'NONE',  ( 29.31284564681175198, -295.1275702476369247, -308.3981541184227808 ) ) ;
#32995 = CARTESIAN_POINT ( 'NONE',  ( -94.35931153799546678, -284.5577536097508755, -316.1290841247947014 ) ) ;
#32996 = CARTESIAN_POINT ( 'NONE',  ( 16.78080552286736093, -275.3635927578397968, -324.8740543008594273 ) ) ;
#32997 = CARTESIAN_POINT ( 'NONE',  ( -109.3812667624447528, -291.5459282934968996, -243.3092594025718256 ) ) ;
#32998 = CARTESIAN_POINT ( 'NONE',  ( -96.59926540084762792, -283.3341574241499075, -223.1504577130137648 ) ) ;
#32999 = CARTESIAN_POINT ( 'NONE',  ( -33.54465406605054767, -292.4320021119605144, -193.4759651065400021 ) ) ;
#33000 = CARTESIAN_POINT ( 'NONE',  ( -110.1433600571587448, -290.8026839235597549, -276.6359475161144132 ) ) ;
#33001 = CARTESIAN_POINT ( 'NONE',  ( -57.23711263161519724, -282.8906705383787994, 52.50000000000000711 ) ) ;
#33002 = CARTESIAN_POINT ( 'NONE',  ( 153.8638694011456209, 19.41512922080416459, -11.71395201670714137 ) ) ;
#33003 = CARTESIAN_POINT ( 'NONE',  ( 45.60988505783635105, 10.90853662155476123, -328.4231153613965830 ) ) ;
#33004 = CARTESIAN_POINT ( 'NONE',  ( 19.28214613700657409, -283.7738104452764674, -321.5896715200768199 ) ) ;
#33005 = CARTESIAN_POINT ( 'NONE',  ( 31.95455697924147032, -279.4809262143061233, -303.7686719486574702 ) ) ;
#33006 = ORIENTED_EDGE ( 'NONE', *, *, #35340, .T. ) ;
#33007 = CARTESIAN_POINT ( 'NONE',  ( 26.73566498478314557, -279.9876221794355047, -234.7476745513384628 ) ) ;
#33008 = CARTESIAN_POINT ( 'NONE',  ( -67.70417518725312789, -277.1065510281231354, -341.0991162568871573 ) ) ;
#33009 = CARTESIAN_POINT ( 'NONE',  ( -96.24943387977992870, -281.1872334065592440, -224.1895642735208867 ) ) ;
#33010 = CARTESIAN_POINT ( 'NONE',  ( -20.07155585692473210, -109.6737398891278872, -360.5847716769698650 ) ) ;
#33011 = CARTESIAN_POINT ( 'NONE',  ( 27.79315718508426158, -280.6540538279702446, -310.4120297959395884 ) ) ;
#33012 = CARTESIAN_POINT ( 'NONE',  ( -106.7525104449498770, -282.2114110230291431, -297.9607488108187567 ) ) ;
#33013 = CARTESIAN_POINT ( 'NONE',  ( -112.6377882096997496, -274.5195184050028843, -261.9465711157578198 ) ) ;
#33014 = CARTESIAN_POINT ( 'NONE',  ( -36.98895936933229223, -295.5399337075684798, -343.4342399511824624 ) ) ;
#33015 = ORIENTED_EDGE ( 'NONE', *, *, #53026, .F. ) ;
#33016 = CARTESIAN_POINT ( 'NONE',  ( -19.93925799111839581, -290.9652209968617740, -198.9054221822963768 ) ) ;
#33017 = CARTESIAN_POINT ( 'NONE',  ( -1.507864905510987619, -277.2411026900951470, -338.3997029187212888 ) ) ;
#33018 = CARTESIAN_POINT ( 'NONE',  ( 23.05233286324211761, -274.9816108038741049, -229.3318581168621506 ) ) ;
#33019 = CARTESIAN_POINT ( 'NONE',  ( 38.42438135388979248, -274.3223201608140585, -258.4023092643404311 ) ) ;
#33020 = FACE_OUTER_BOUND ( 'NONE', #66751, .T. ) ;
#33021 = CARTESIAN_POINT ( 'NONE',  ( 33.42917534683050462, -273.2286666227298042, -245.3776858065712076 ) ) ;
#33022 = DIRECTION ( 'NONE',  ( 0.000000000000000000, 0.000000000000000000, -1.000000000000000000 ) ) ;
#33023 = CARTESIAN_POINT ( 'NONE',  ( 197.7129307445136135, 68.09401877029563366, 12.80442219776279522 ) ) ;
#33024 = CARTESIAN_POINT ( 'NONE',  ( 25.83236137166688096, -283.1417034202588638, -307.6537174318929146 ) ) ;
#33025 = CARTESIAN_POINT ( 'NONE',  ( 21.74958287569445758, -283.9615763298186266, -318.1539726874498228 ) ) ;
#33026 = CARTESIAN_POINT ( 'NONE',  ( -108.1252873150857567, -284.1415038273368054, -252.0970424947773267 ) ) ;
#33027 = CARTESIAN_POINT ( 'NONE',  ( -1.094891457369224774, -274.9628548482588712, -334.7043125496806510 ) ) ;
#33028 = CARTESIAN_POINT ( 'NONE',  ( -59.29111986838636028, -285.1995922600401627, -341.3312194994555853 ) ) ;
#33029 = CARTESIAN_POINT ( 'NONE',  ( -79.04011402569013001, -276.1053380077994461, -331.1846851520571136 ) ) ;
#33030 = DIRECTION ( 'NONE',  ( -0.000000000000000000, -1.000000000000000000, -0.000000000000000000 ) ) ;
#33031 = CARTESIAN_POINT ( 'NONE',  ( -21.88219214424944781, -275.3346340096072140, -198.7006010605214499 ) ) ;
#33032 = CARTESIAN_POINT ( 'NONE',  ( -74.94434090351494149, -212.1443419142231051, 22.50000000000000000 ) ) ;
#33033 = CARTESIAN_POINT ( 'NONE',  ( -113.6046712925309805, -279.2320628877154718, -280.1690514530494056 ) ) ;
#33034 = VERTEX_POINT ( 'NONE', #52591 ) ;
#33035 = ORIENTED_EDGE ( 'NONE', *, *, #33481, .T. ) ;
#33036 = CARTESIAN_POINT ( 'NONE',  ( 200.7304780712221088, 15.47998366481819232, 9.999999999999360512 ) ) ;
#33037 = CARTESIAN_POINT ( 'NONE',  ( -80.25835857444245391, -287.3385395835723557, -207.8600831769959427 ) ) ;
#33038 = ADVANCED_FACE ( 'NONE', ( #81472 ), #76256, .T. ) ;
#33039 = CARTESIAN_POINT ( 'NONE',  ( 3.898999922924293315, -293.6779872806772005, -330.7912957574439474 ) ) ;
#33040 = CARTESIAN_POINT ( 'NONE',  ( -99.11774654396798212, -290.5105788848168231, -224.5456910706301983 ) ) ;
#33041 = CARTESIAN_POINT ( 'NONE',  ( 27.26269421424738582, -285.3035601250166451, -234.1418532386952336 ) ) ;
#33043 = CARTESIAN_POINT ( 'NONE',  ( -104.4660478448649741, -289.2071674028874213, -239.1794574350610105 ) ) ;
#33042 = CARTESIAN_POINT ( 'NONE',  ( -25.02548029837719668, -284.7868740185165279, -197.7581421543308977 ) ) ;
#33044 = CARTESIAN_POINT ( 'NONE',  ( -56.40733926150255684, -284.5084655308113497, -341.2387019435893762 ) ) ;
#33045 = CARTESIAN_POINT ( 'NONE',  ( 36.26105334821276216, -273.3669764081778339, -255.9515609998747721 ) ) ;
#33046 = CARTESIAN_POINT ( 'NONE',  ( -12.94040447992797382, -284.7639539793325412, -198.1737424588929457 ) ) ;
#33047 = CARTESIAN_POINT ( 'NONE',  ( -59.58001654263917146, -299.7644559225720400, -198.6798162934733227 ) ) ;
#33048 = CARTESIAN_POINT ( 'NONE',  ( 37.80770594883809110, -285.5313494615251102, -268.7501587031374584 ) ) ;
#33049 = CARTESIAN_POINT ( 'NONE',  ( -46.49772091774341476, -280.8745014589430298, -197.6491612780373544 ) ) ;
#33050 = CARTESIAN_POINT ( 'NONE',  ( -54.06826212402987153, -291.2664552886117804, -343.6965167060329804 ) ) ;
#33051 = DIRECTION ( 'NONE',  ( 0.000000000000000000, 0.000000000000000000, 1.000000000000000000 ) ) ;
#33052 = CARTESIAN_POINT ( 'NONE',  ( 175.2296996224750103, 250.0000000000000568, 0.000000000000000000 ) ) ;
#33053 = CARTESIAN_POINT ( 'NONE',  ( -83.28979008170658460, -297.5958328521694511, -330.4111278821402493 ) ) ;
#33054 =( BOUNDED_SURFACE ( )  B_SPLINE_SURFACE ( 3, 2, ( 
 ( #31900, #54597, #47956 ),
 ( #90109, #75915, #91020 ),
 ( #17701, #46554, #83468 ),
 ( #55083, #24800, #69753 ) ),
 .UNSPECIFIED., .F., .F., .F. ) 
 B_SPLINE_SURFACE_WITH_KNOTS ( ( 4, 4 ),
 ( 3, 3 ),
 ( 4.278565243615663150, 4.712388980384689674 ),
 ( 0.000000000000000000, 1.000000000000000000 ),
 .UNSPECIFIED. ) 
 GEOMETRIC_REPRESENTATION_ITEM ( )  RATIONAL_B_SPLINE_SURFACE ( (
 ( 1.000000000000000000, 0.8168508380123946644, 1.000000000000000000),
 ( 1.000000000000000000, 0.7849082635113637796, 1.000000000000000000),
 ( 1.000000000000000000, 0.7478056585118687538, 1.000000000000000000),
 ( 1.000000000000000000, 0.7071067811865480168, 1.000000000000000000) ) ) 
 REPRESENTATION_ITEM ( '' )  SURFACE ( )  );
#33055 = CARTESIAN_POINT ( 'NONE',  ( -39.74036040608782372, -278.0218940935562273, -195.3866175647039256 ) ) ;
#33056 = CARTESIAN_POINT ( 'NONE',  ( -13.90595589979413305, -291.5457240562551533, -197.1279067728692382 ) ) ;
#33057 = CARTESIAN_POINT ( 'NONE',  ( -107.6374733117404361, -294.6553083425070554, -292.9976750377088592 ) ) ;
#33058 = CARTESIAN_POINT ( 'NONE',  ( 35.18755864084348417, -280.3924270021191205, -282.2249327562059307 ) ) ;
#33059 = CARTESIAN_POINT ( 'NONE',  ( -33.95109675677849737, -272.1749817370911728, -195.9983718758237501 ) ) ;
#33060 = CARTESIAN_POINT ( 'NONE',  ( 34.12340519024993313, -294.6420029240479153, -253.1614981241125406 ) ) ;
#33061 = CARTESIAN_POINT ( 'NONE',  ( -20.25526795762937127, -294.7662352645559167, -195.3538533559490702 ) ) ;
#33062 = CARTESIAN_POINT ( 'NONE',  ( -104.6329770076042962, -295.5025213128503765, -234.2686448545316296 ) ) ;
#33064 = CARTESIAN_POINT ( 'NONE',  ( -1.208053148290874734, -292.8194382752522529, -337.2214004581527433 ) ) ;
#33063 =( BOUNDED_CURVE ( )  B_SPLINE_CURVE ( 3, ( #40346, #34219, #19078, #91954 ),
 .UNSPECIFIED., .F., .F. ) 
 B_SPLINE_CURVE_WITH_KNOTS ( ( 4, 4 ),
 ( 0.7297276562269670031, 1.570796326794896558 ),
 .UNSPECIFIED. ) 
 CURVE ( )  GEOMETRIC_REPRESENTATION_ITEM ( )  RATIONAL_B_SPLINE_CURVE ( ( 1.000000000000000000, 0.9419139527835179715, 0.9419139527835179715, 1.000000000000000000 ) ) 
 REPRESENTATION_ITEM ( '' )  );
#33065 = CARTESIAN_POINT ( 'NONE',  ( -103.3661617519135376, -291.5405758500167508, -302.8595084458196993 ) ) ;
#33066 = DIRECTION ( 'NONE',  ( -0.4467993836324651857, 0.8946341770721982778, 0.000000000000000000 ) ) ;
#33067 = CARTESIAN_POINT ( 'NONE',  ( -33.51018118450576821, -292.9044133253037785, -197.2875196018106294 ) ) ;
#33068 = DIRECTION ( 'NONE',  ( -1.000000000000000000, 0.000000000000000000, 0.000000000000000000 ) ) ;
#33070 = CARTESIAN_POINT ( 'NONE',  ( 1.569833535611802722, -294.5164746057924390, -332.1858019889293132 ) ) ;
#33069 = CARTESIAN_POINT ( 'NONE',  ( -3.651325501374625304, -280.6299759995120553, -337.7799476852829343 ) ) ;
#33071 = CARTESIAN_POINT ( 'NONE',  ( 0.8683584521353456820, -282.5570739756349781, -337.2268656555586404 ) ) ;
#33072 = CARTESIAN_POINT ( 'NONE',  ( -35.90384704330953980, -282.7013356010795633, -347.3396578471469525 ) ) ;
#33073 = CARTESIAN_POINT ( 'NONE',  ( 4.622124544456664985, -286.4845634646821964, -332.3837845326423235 ) ) ;
#33074 = CARTESIAN_POINT ( 'NONE',  ( -114.4693872376281121, -273.8646567567205921, -270.3778293100139081 ) ) ;
#33075 = CARTESIAN_POINT ( 'NONE',  ( -8.320669093651757109, -281.1590257665811237, -340.9897099980346411 ) ) ;
#33076 = CARTESIAN_POINT ( 'NONE',  ( -17.81634514663873858, -287.7263923439008408, -344.5248087062251443 ) ) ;
#33077 = CARTESIAN_POINT ( 'NONE',  ( 205.7381008070598227, 0.000000000000000000, -7.000000000000000888 ) ) ;
#33078 = CARTESIAN_POINT ( 'NONE',  ( 19.07512941299792075, -294.4836231006923413, -222.7840041404752753 ) ) ;
#33079 = CARTESIAN_POINT ( 'NONE',  ( 32.48869680045604724, -277.3763901317145155, -301.3824325282109839 ) ) ;
#33080 = CARTESIAN_POINT ( 'NONE',  ( -35.65805774584396914, -279.7405373823978607, -197.3469799397344957 ) ) ;
#33081 = CARTESIAN_POINT ( 'NONE',  ( -42.05608268446400899, -292.1609478858293869, -193.5055742552185052 ) ) ;
#33082 = CARTESIAN_POINT ( 'NONE',  ( -2.323627262914165215, -280.6722594902389005, -337.3166911144028859 ) ) ;
#33083 = CARTESIAN_POINT ( 'NONE',  ( 32.97273632739031513, -292.8814269949173195, -290.8827005847365399 ) ) ;
#33084 = CARTESIAN_POINT ( 'NONE',  ( -110.6556608729419509, -294.3489524138628894, -286.1745240955714280 ) ) ;
#33085 = EDGE_LOOP ( 'NONE', ( #7167, #69563, #3504, #19299 ) ) ;
#33086 = DIRECTION ( 'NONE',  ( 0.000000000000000000, 0.000000000000000000, -1.000000000000000000 ) ) ;
#33087 = CARTESIAN_POINT ( 'NONE',  ( 6.094495920175158510, -293.9526385777739961, -329.1718042848390269 ) ) ;
#33088 = CARTESIAN_POINT ( 'NONE',  ( 207.2844387419798693, 0.02860196560701895249, -7.415405905516098350 ) ) ;
#33089 = CARTESIAN_POINT ( 'NONE',  ( -92.05005921254146983, -282.6952119285918457, -226.6919474004047572 ) ) ;
#33090 = CARTESIAN_POINT ( 'NONE',  ( -14.88359410320592957, -297.3856292487311066, -193.5998961811205561 ) ) ;
#33091 = CARTESIAN_POINT ( 'NONE',  ( 20.14462282524261028, -279.0145978632019137, -220.9892991889750533 ) ) ;
#33092 = CARTESIAN_POINT ( 'NONE',  ( -73.39552163992144074, -286.8996886490954807, -202.8234010165467680 ) ) ;
#33093 = CARTESIAN_POINT ( 'NONE',  ( -48.06307987884917310, -289.0255318033749177, -342.6205331511768009 ) ) ;
#33094 = CARTESIAN_POINT ( 'NONE',  ( -48.69574212002144264, -278.7193387639670163, -343.2264087052357695 ) ) ;
#33095 = CARTESIAN_POINT ( 'NONE',  ( -70.47636386213999060, -293.5113093754877127, -337.2486419758903367 ) ) ;
#33096 = CARTESIAN_POINT ( 'NONE',  ( -105.1224510126624949, -274.5418370036176157, -241.0388890186827950 ) ) ;
#33097 = ADVANCED_FACE ( 'NONE', ( #45475 ), #33156, .T. ) ;
#33098 = CARTESIAN_POINT ( 'NONE',  ( -71.85439456126579216, -276.3139440544882177, -335.1518687466526103 ) ) ;
#33099 = EDGE_LOOP ( 'NONE', ( #31072, #54676, #23762, #56402 ) ) ;
#33100 = CARTESIAN_POINT ( 'NONE',  ( 76.35222964319555672, -299.1058724536635509, -193.3884058114072388 ) ) ;
#33101 = CARTESIAN_POINT ( 'NONE',  ( -69.35554290129813637, -291.3968966467350583, -337.5654933820780457 ) ) ;
#33102 = CARTESIAN_POINT ( 'NONE',  ( 8.441914161598603528, -296.0370118720466053, -331.2733587559479247 ) ) ;
#33103 = CARTESIAN_POINT ( 'NONE',  ( 143.6449502718966755, 0.000000000000000000, -47.19625681453479871 ) ) ;
#33104 = EDGE_CURVE ( 'NONE', #43740, #70513, #36113, .T. ) ;
#33105 = CARTESIAN_POINT ( 'NONE',  ( -100.3876663733047252, -290.6950065729685662, -307.4621349646194517 ) ) ;
#33106 = CARTESIAN_POINT ( 'NONE',  ( -43.54160339320051065, -248.0334966641291601, -463.3298803830878114 ) ) ;
#33107 = VERTEX_POINT ( 'NONE', #62047 ) ;
#33108 = CARTESIAN_POINT ( 'NONE',  ( -113.2901850105230466, -297.3554776023441377, -258.2302207225033612 ) ) ;
#33109 = CARTESIAN_POINT ( 'NONE',  ( -101.2719468598982928, -288.1490014129813630, -311.1176275136417644 ) ) ;
#33110 = AXIS2_PLACEMENT_3D ( 'NONE', #64091, #65479, #596 ) ;
#33111 = CARTESIAN_POINT ( 'NONE',  ( -68.17288964948761532, -297.9916296626012127, -199.7693638474820830 ) ) ;
#33112 = CARTESIAN_POINT ( 'NONE',  ( 152.4536156746142410, 275.5000000000000568, -14.50000000000000000 ) ) ;
#33113 = DIRECTION ( 'NONE',  ( -0.000000000000000000, 1.000000000000000000, -0.000000000000000000 ) ) ;
#33114 = CARTESIAN_POINT ( 'NONE',  ( -106.6389794118234562, -292.4860736968058745, -238.2884066506962597 ) ) ;
#33115 = CARTESIAN_POINT ( 'NONE',  ( -115.3430155898818299, -287.2662352645559167, -252.5904736702033517 ) ) ;
#33116 = CARTESIAN_POINT ( 'NONE',  ( -106.9090814665903793, -286.1908228946193731, -298.0775466192001772 ) ) ;
#33117 = CARTESIAN_POINT ( 'NONE',  ( 0.3998229562577181873, -272.5559825928079931, -205.7272299721121556 ) ) ;
#33118 = CARTESIAN_POINT ( 'NONE',  ( -100.5152130761826186, -275.0052284895160710, -230.9857264471263250 ) ) ;
#33119 = CARTESIAN_POINT ( 'NONE',  ( -97.91922718657802704, -289.2258106236884032, -227.0110789502120667 ) ) ;
#33120 = CARTESIAN_POINT ( 'NONE',  ( -41.29590191099759267, -278.9618188557272447, -346.0356625295015647 ) ) ;
#33121 = ORIENTED_EDGE ( 'NONE', *, *, #75497, .T. ) ;
#33123 = CARTESIAN_POINT ( 'NONE',  ( 18.04718183035087264, -280.2220641233119522, -222.6348310530956383 ) ) ;
#33122 = CARTESIAN_POINT ( 'NONE',  ( 17.06281253990017532, -280.8557823844755603, -221.6872132557001294 ) ) ;
#33124 = CARTESIAN_POINT ( 'NONE',  ( 10.34464992864179500, -277.4915762735131466, -330.4914449567640418 ) ) ;
#33125 = CARTESIAN_POINT ( 'NONE',  ( -35.33099143948599163, -278.8717622486105370, -193.7715137033361827 ) ) ;
#33126 = CARTESIAN_POINT ( 'NONE',  ( -78.45397945840984733, -207.3402917149092843, -354.1116341293970891 ) ) ;
#33127 = CARTESIAN_POINT ( 'NONE',  ( 37.36566509161409755, -276.7155043873352156, -288.0708150203219589 ) ) ;
#33128 = DIRECTION ( 'NONE',  ( 0.000000000000000000, 0.000000000000000000, -1.000000000000000000 ) ) ;
#33129 = CARTESIAN_POINT ( 'NONE',  ( -36.96279093540193372, -275.5769624299149996, -194.0424553924729310 ) ) ;
#33130 = CARTESIAN_POINT ( 'NONE',  ( -53.35057174420112602, -276.3376638359844719, -200.3683826091709648 ) ) ;
#33131 = ORIENTED_EDGE ( 'NONE', *, *, #88943, .F. ) ;
#33132 = CARTESIAN_POINT ( 'NONE',  ( 200.2349812190172713, 66.43136063442170780, 7.741079165001067963 ) ) ;
#33133 = CARTESIAN_POINT ( 'NONE',  ( 18.89005616163744605, -287.9668141813629632, -223.3073691477756597 ) ) ;
#33134 = CARTESIAN_POINT ( 'NONE',  ( 2.194386335091289109, -288.3341391797164306, -205.4698868318808991 ) ) ;
#33135 = CARTESIAN_POINT ( 'NONE',  ( -106.6653291487429556, -290.2084013814618402, -247.1635507058722112 ) ) ;
#33136 = CARTESIAN_POINT ( 'NONE',  ( -30.88276599135153688, -285.6393417142027147, -193.6809630047584676 ) ) ;
#33137 = DIRECTION ( 'NONE',  ( 0.000000000000000000, 0.000000000000000000, 1.000000000000000000 ) ) ;
#33138 = CARTESIAN_POINT ( 'NONE',  ( 26.23800227585467582, -280.4623352022327367, -307.9328669103387028 ) ) ;
#33139 = CARTESIAN_POINT ( 'NONE',  ( 31.64163917898076051, -289.7750386339739066, -297.9254880904029505 ) ) ;
#33140 = CARTESIAN_POINT ( 'NONE',  ( -48.45213739287968480, -281.6760186174969363, -343.2121024294415292 ) ) ;
#33141 = CARTESIAN_POINT ( 'NONE',  ( -89.83748714940942648, -280.6074712480287872, -218.8551773005068242 ) ) ;
#33142 = CARTESIAN_POINT ( 'NONE',  ( 15.64682387207299818, -276.7689712314507346, -320.6622587843362453 ) ) ;
#33143 = CARTESIAN_POINT ( 'NONE',  ( -112.1807189268762954, -289.1416171884576443, -286.7052296321610356 ) ) ;
#33144 = CARTESIAN_POINT ( 'NONE',  ( -73.54598975211922607, -286.3874300006120848, -202.5274969870066570 ) ) ;
#33145 = CARTESIAN_POINT ( 'NONE',  ( -4.805674683699147742, -286.9616232467326427, -200.6407195914692352 ) ) ;
#33146 = CARTESIAN_POINT ( 'NONE',  ( 9.910312051490468122, -282.5468458581152049, -326.0715290498166610 ) ) ;
#33147 = ORIENTED_EDGE ( 'NONE', *, *, #30544, .T. ) ;
#33148 = DIRECTION ( 'NONE',  ( 0.000000000000000000, 0.000000000000000000, -1.000000000000000000 ) ) ;
#33149 = CARTESIAN_POINT ( 'NONE',  ( -112.4450284264164281, -292.5444324235590443, -259.9863624170432104 ) ) ;
#33150 = CARTESIAN_POINT ( 'NONE',  ( -70.66767281404656842, -290.3066292962160446, -201.4940153883243852 ) ) ;
#33151 = CARTESIAN_POINT ( 'NONE',  ( 3.069734774904482322, -273.6679745993777715, -209.2241232902831314 ) ) ;
#33152 = CARTESIAN_POINT ( 'NONE',  ( -111.1199406074225919, -295.6278934692866756, -292.0890015627458070 ) ) ;
#33153 = CARTESIAN_POINT ( 'NONE',  ( -38.89294845073587226, -290.5122174202311953, -196.6841108303447925 ) ) ;
#33154 = CARTESIAN_POINT ( 'NONE',  ( -58.72208927509728937, -293.5723461906366083, -341.2190954549542425 ) ) ;
#33155 = CARTESIAN_POINT ( 'NONE',  ( -78.38380932092603359, -290.8228228185203648, -331.2719119771732039 ) ) ;
#33156 = CYLINDRICAL_SURFACE ( 'NONE', #634, 1.499999999999999556 ) ;
#33157 = CARTESIAN_POINT ( 'NONE',  ( -110.9012812813950575, -292.3636499936778819, -285.0544567425449145 ) ) ;
#33158 = CARTESIAN_POINT ( 'NONE',  ( -7.884618368823592682, -290.4370185387188599, -201.1928959562539205 ) ) ;
#33159 = CARTESIAN_POINT ( 'NONE',  ( -80.89647905448541110, -297.6431033639914290, -331.4813995521877814 ) ) ;
#33160 = CARTESIAN_POINT ( 'NONE',  ( -5.707835343663168359, -287.4198487686622343, -204.2964989815021681 ) ) ;
#33161 = CARTESIAN_POINT ( 'NONE',  ( -30.02423387210372852, -276.1242252469000391, -195.3620413895717718 ) ) ;
#33162 = CARTESIAN_POINT ( 'NONE',  ( -9.371169638907522526, -275.4894771109472913, -341.6749184898459362 ) ) ;
#33163 = CARTESIAN_POINT ( 'NONE',  ( -97.21408223664178649, -296.3961389958371342, -222.2003800102980904 ) ) ;
#33164 = CARTESIAN_POINT ( 'NONE',  ( -29.62982346885026530, -275.1931643009767754, -344.0231973670973389 ) ) ;
#33165 = CARTESIAN_POINT ( 'NONE',  ( -69.11619310425287210, -277.7107528691086600, -203.0432466714617021 ) ) ;
#33166 = CARTESIAN_POINT ( 'NONE',  ( -68.46484161296314142, -274.8389907444129676, -203.8756922473113775 ) ) ;
#33167 = CARTESIAN_POINT ( 'NONE',  ( -12.15009062969877895, -275.1297510472127783, -342.3318467207231492 ) ) ;
#33168 = LINE ( 'NONE', #55432, #61119 ) ;
#33169 = CARTESIAN_POINT ( 'NONE',  ( -109.2314900355806628, -273.3817762121369697, -256.8330798644309994 ) ) ;
#33170 = AXIS2_PLACEMENT_3D ( 'NONE', #59760, #52159, #80572 ) ;
#33171 = CARTESIAN_POINT ( 'NONE',  ( 208.4306832106270804, -147.7221692137691775, 0.000000000000000000 ) ) ;
#33173 = CARTESIAN_POINT ( 'NONE',  ( 30.17562777812529617, -275.0118763886091529, -242.4721066380130026 ) ) ;
#33172 = CARTESIAN_POINT ( 'NONE',  ( -18.16769952643022634, -286.8263164446934184, -343.2361102695281261 ) ) ;
#33174 = CARTESIAN_POINT ( 'NONE',  ( 20.57290064324190126, -288.2388450483110205, -321.1244443137596249 ) ) ;
#33175 = AXIS2_PLACEMENT_3D ( 'NONE', #82073, #89628, #90106 ) ;
#33176 = CARTESIAN_POINT ( 'NONE',  ( -31.83253012887607980, -288.6512782657153480, -347.1951243307299819 ) ) ;
#33177 = CARTESIAN_POINT ( 'NONE',  ( -32.07894891472518140, -300.0976079745157108, -195.0041440767023744 ) ) ;
#33178 = CARTESIAN_POINT ( 'NONE',  ( 21.96085315542601890, -292.1788802332337127, -316.0245657363597616 ) ) ;
#33179 = CARTESIAN_POINT ( 'NONE',  ( 21.85286100594614567, -280.0893759962342529, -221.3696620610721766 ) ) ;
#33180 = DIRECTION ( 'NONE',  ( 1.040834085586084059E-15, 0.000000000000000000, -1.000000000000000000 ) ) ;
#33181 = CARTESIAN_POINT ( 'NONE',  ( -59.32065368257949700, -277.7676009466405844, -198.6004912461297067 ) ) ;
#33182 = CYLINDRICAL_SURFACE ( 'NONE', #65608, 5.000000000000000888 ) ;
#33183 = CARTESIAN_POINT ( 'NONE',  ( -61.39957090083058944, -288.1666413433127332, -339.7033804084038593 ) ) ;
#33184 = DIRECTION ( 'NONE',  ( 1.000000000000000000, -0.000000000000000000, 0.000000000000000000 ) ) ;
#33185 = DIRECTION ( 'NONE',  ( 0.000000000000000000, -1.000000000000000000, 0.000000000000000000 ) ) ;
#33186 = CARTESIAN_POINT ( 'NONE',  ( -92.20530673716717729, -289.2679089803717147, -219.2052097926309955 ) ) ;
#33187 = CARTESIAN_POINT ( 'NONE',  ( -63.57142563311793282, -275.2241214385912258, -201.4801639173576007 ) ) ;
#33188 = CARTESIAN_POINT ( 'NONE',  ( 6.601100826818031564, -283.8932888353776320, -332.9369214624183542 ) ) ;
#33190 = CARTESIAN_POINT ( 'NONE',  ( -109.9944159237722658, -284.6525547848441988, -262.7500509422749815 ) ) ;
#33189 = CARTESIAN_POINT ( 'NONE',  ( -35.84299033034217530, -296.0909377233871282, -195.0064122322097262 ) ) ;
#33191 = CARTESIAN_POINT ( 'NONE',  ( 20.30584824956651957, -276.3367230657516984, -224.6010986315913840 ) ) ;
#33192 = CARTESIAN_POINT ( 'NONE',  ( 26.77312003911535854, -275.8734086592781409, -235.0150759722817213 ) ) ;
#33193 = CARTESIAN_POINT ( 'NONE',  ( -1.313224155831289597, -284.5744958153852053, -336.1552240957446429 ) ) ;
#33194 = CARTESIAN_POINT ( 'NONE',  ( -35.79735738312007243, -297.1306974705111088, -197.1260763546636383 ) ) ;
#33195 = VERTEX_POINT ( 'NONE', #12814 ) ;
#33196 = DIRECTION ( 'NONE',  ( 0.000000000000000000, 0.000000000000000000, 1.000000000000000000 ) ) ;
#33197 = CARTESIAN_POINT ( 'NONE',  ( 39.50199093484781798, -293.4565105467999047, -276.0412605930700920 ) ) ;
#33198 = CARTESIAN_POINT ( 'NONE',  ( -74.39349363484268451, -287.5368150357599006, -205.5465134418000730 ) ) ;
#33199 = CARTESIAN_POINT ( 'NONE',  ( 175.2296996224750103, 276.0000000000000568, 0.000000000000000000 ) ) ;
#33200 = CARTESIAN_POINT ( 'NONE',  ( 31.09738932201053885, -296.4086741954486115, -195.3901485728259502 ) ) ;
#33201 = CARTESIAN_POINT ( 'NONE',  ( -111.6738409199724629, -277.5045736829874272, -289.8779844555725731 ) ) ;
#33202 = CARTESIAN_POINT ( 'NONE',  ( -98.40045421182952623, -288.3389419493095147, -315.9707378627116441 ) ) ;
#33203 = CARTESIAN_POINT ( 'NONE',  ( -61.74624149085314428, -284.8951274314487705, -339.9499248228096349 ) ) ;
#33204 = CARTESIAN_POINT ( 'NONE',  ( -18.74092857068766094, -278.5694756802828351, -341.9989941966868514 ) ) ;
#33205 = CARTESIAN_POINT ( 'NONE',  ( -1.263912643127763191, -287.9464861505516637, -203.0038648904761089 ) ) ;
#33206 = CARTESIAN_POINT ( 'NONE',  ( -65.59245829820396523, -281.6828876231624577, -200.8852566155559884 ) ) ;
#33207 = CARTESIAN_POINT ( 'NONE',  ( -32.68472395937533292, -274.2759688540571688, -193.4889237914557896 ) ) ;
#33208 = CARTESIAN_POINT ( 'NONE',  ( -112.4848703791476083, -278.1752677026754554, -287.1689723713978424 ) ) ;
#33209 = CARTESIAN_POINT ( 'NONE',  ( -31.46474598745840723, -296.8976669832055109, -344.6198714485938126 ) ) ;
#33210 = DIRECTION ( 'NONE',  ( 0.000000000000000000, 0.000000000000000000, 1.000000000000000000 ) ) ;
#33211 = DIRECTION ( 'NONE',  ( 0.000000000000000000, 0.000000000000000000, 1.000000000000000000 ) ) ;
#33212 = CARTESIAN_POINT ( 'NONE',  ( -104.7001572184116753, -271.2530539699363885, -235.0791172798350033 ) ) ;
#33213 = CARTESIAN_POINT ( 'NONE',  ( 27.91906468313075607, -274.6143612140683672, -237.5126626503203227 ) ) ;
#33214 = CARTESIAN_POINT ( 'NONE',  ( -35.84949538551849457, -299.1500887552125505, -193.6699611145742210 ) ) ;
#33215 = CARTESIAN_POINT ( 'NONE',  ( 35.96713779180102222, -289.4460535570865432, -280.6412464792344394 ) ) ;
#33216 = CARTESIAN_POINT ( 'NONE',  ( -113.5402016165382548, -298.0097694524600342, -275.3138384975532063 ) ) ;
#33217 = CARTESIAN_POINT ( 'NONE',  ( -109.9643658699752393, -297.4487345068091031, -294.7323538720502825 ) ) ;
#33218 = CARTESIAN_POINT ( 'NONE',  ( -111.5208389929369162, -292.6843288237747061, -260.1024113009410144 ) ) ;
#33219 = CARTESIAN_POINT ( 'NONE',  ( -99.50262570966383180, -277.1176352740963580, -228.6032428094024453 ) ) ;
#33220 = CARTESIAN_POINT ( 'NONE',  ( -110.4530485355167997, -280.2903059248055229, -284.4299598767115640 ) ) ;
#33221 = CARTESIAN_POINT ( 'NONE',  ( -84.97793486829843346, -295.4692572898205754, -213.0915344157571951 ) ) ;
#33222 = CARTESIAN_POINT ( 'NONE',  ( -93.46793609787764012, -285.7096954792746715, -321.2738799542651122 ) ) ;
#33223 = CARTESIAN_POINT ( 'NONE',  ( 2.627008637653146295, -285.5224890690780057, -208.9060254940336847 ) ) ;
#33224 = CARTESIAN_POINT ( 'NONE',  ( -111.9030559682143604, -274.5283560713371003, -270.3862797920663752 ) ) ;
#33225 = VERTEX_POINT ( 'NONE', #48757 ) ;
#33226 = CARTESIAN_POINT ( 'NONE',  ( 34.54175682619548837, -287.3881966606786023, -283.2007481613696882 ) ) ;
#33227 = ORIENTED_EDGE ( 'NONE', *, *, #59326, .F. ) ;
#33228 = CARTESIAN_POINT ( 'NONE',  ( 6.758540737419452604, -283.5477435763236826, -333.1688832126113766 ) ) ;
#33229 = CARTESIAN_POINT ( 'NONE',  ( -110.3628441122352086, -272.8853797144980717, -270.3653515045655240 ) ) ;
#33230 = CARTESIAN_POINT ( 'NONE',  ( -40.78319162524128672, -284.8048307975259945, -193.7836104478722064 ) ) ;
#33231 = CARTESIAN_POINT ( 'NONE',  ( -31.10486643115158145, -281.0702406907684576, -193.7976601323755403 ) ) ;
#33232 = CARTESIAN_POINT ( 'NONE',  ( -72.20744052326691076, -281.1195901126344552, -202.4710646483769665 ) ) ;
#33233 = CARTESIAN_POINT ( 'NONE',  ( 27.83118925510074249, -281.3477514490717226, -229.2949179761089624 ) ) ;
#33234 = CIRCLE ( 'NONE', #15141, 2.500000000000002220 ) ;
#33235 = CARTESIAN_POINT ( 'NONE',  ( 27.36219212280433055, -290.6237833571632905, -239.2376011013261916 ) ) ;
#33236 = CARTESIAN_POINT ( 'NONE',  ( -55.75868456242086779, -169.6758193678651025, -364.5828727736617338 ) ) ;
#33237 = ORIENTED_EDGE ( 'NONE', *, *, #88734, .T. ) ;
#33238 = CARTESIAN_POINT ( 'NONE',  ( -84.36181329012404717, -275.4034827085500865, -212.1448197354905005 ) ) ;
#33239 = CARTESIAN_POINT ( 'NONE',  ( 138.2325648905753610, 180.7664419875970623, -241.1855197640491042 ) ) ;
#33240 = AXIS2_PLACEMENT_3D ( 'NONE', #84405, #64087, #34242 ) ;
#33241 = CARTESIAN_POINT ( 'NONE',  ( 35.36815920766267851, -279.3544182253640429, -253.4755276013975163 ) ) ;
#33242 = CARTESIAN_POINT ( 'NONE',  ( 36.12269179020163534, -295.5585899757391530, -289.7765019833174733 ) ) ;
#33243 = CARTESIAN_POINT ( 'NONE',  ( -82.42919066686779672, -295.0348199151614494, -327.9670460734145649 ) ) ;
#33244 = CARTESIAN_POINT ( 'NONE',  ( -81.88964679804441005, -290.9705478309996920, -207.6314810430274918 ) ) ;
#33245 = CARTESIAN_POINT ( 'NONE',  ( -82.08642841123406697, -219.1949203529281647, -349.1242040296514233 ) ) ;
#33247 = CARTESIAN_POINT ( 'NONE',  ( 30.70725159432555884, -285.5713680761861610, -241.6668162570057063 ) ) ;
#33246 = CARTESIAN_POINT ( 'NONE',  ( -113.0711862319940906, -294.9936823940829527, -280.9302372399137653 ) ) ;
#33248 = CARTESIAN_POINT ( 'NONE',  ( 17.63729207669877752, -294.7089755207845201, -220.4041347016804195 ) ) ;
#33249 = CARTESIAN_POINT ( 'NONE',  ( -109.1987232286076193, -285.6644807543817706, -285.8419717287972048 ) ) ;
#33250 = ORIENTED_EDGE ( 'NONE', *, *, #87501, .T. ) ;
#33251 = CARTESIAN_POINT ( 'NONE',  ( 38.37619317294442567, -294.6528920351498186, -283.0749528449060790 ) ) ;
#33252 = CARTESIAN_POINT ( 'NONE',  ( 34.00186220612027199, -282.2521035225376522, -286.1118181365835653 ) ) ;
#33253 = CARTESIAN_POINT ( 'NONE',  ( -112.9949607925361477, -295.4992883555790968, -258.2534469423519567 ) ) ;
#33254 = CARTESIAN_POINT ( 'NONE',  ( -95.32970853143022794, -290.6720971471866051, -320.7749028260804494 ) ) ;
#33255 = CARTESIAN_POINT ( 'NONE',  ( -96.53554474093061799, -291.7060953118628959, -221.1918430935569688 ) ) ;
#33256 = CARTESIAN_POINT ( 'NONE',  ( -0.9896000240085451871, -288.7222066576974271, -333.7243181166660406 ) ) ;
#33257 = ORIENTED_EDGE ( 'NONE', *, *, #58566, .F. ) ;
#33258 = LINE ( 'NONE', #62155, #51812 ) ;
#33259 = CARTESIAN_POINT ( 'NONE',  ( -83.41498438703072793, -297.5361043359898758, -330.5733874343066532 ) ) ;
#33260 = CARTESIAN_POINT ( 'NONE',  ( 18.95429746841130481, -297.4279038174026937, -193.8665315653600203 ) ) ;
#33261 = CARTESIAN_POINT ( 'NONE',  ( -36.99522110494318383, -279.1153423193426306, -197.1266424861778717 ) ) ;
#33262 = ORIENTED_EDGE ( 'NONE', *, *, #30544, .F. ) ;
#33263 = CARTESIAN_POINT ( 'NONE',  ( 15.98889792291381973, -274.2917707236242109, -214.9050613733796240 ) ) ;
#33264 = CARTESIAN_POINT ( 'NONE',  ( -71.97387426953163470, -296.0654448987113483, -205.2981877105294757 ) ) ;
#33265 = CARTESIAN_POINT ( 'NONE',  ( -13.36439972901751183, -278.5980054456549624, -340.6715107450201572 ) ) ;
#33266 = CARTESIAN_POINT ( 'NONE',  ( -35.33356310345696016, -272.2171734265552345, -196.1403635641506469 ) ) ;
#33267 = CARTESIAN_POINT ( 'NONE',  ( 1.794469701624061608, -295.7213561357832532, -332.5139165581019824 ) ) ;
#33268 = CARTESIAN_POINT ( 'NONE',  ( -90.27855973992070915, -298.3612535637203678, -219.5744042969455450 ) ) ;
#33269 = DIRECTION ( 'NONE',  ( 1.000000000000000000, 0.000000000000000000, 0.000000000000000000 ) ) ;
#33270 = CARTESIAN_POINT ( 'NONE',  ( -105.2355543238093105, -297.7007546666828262, -305.0730266092111265 ) ) ;
#33271 = CARTESIAN_POINT ( 'NONE',  ( -34.11881225684701491, -296.0922507526707932, -195.1955383508204989 ) ) ;
#33272 = CARTESIAN_POINT ( 'NONE',  ( -55.04505863320998316, -292.4698269058708888, -199.4352146363740133 ) ) ;
#33273 = CARTESIAN_POINT ( 'NONE',  ( -108.3154105057184324, -289.3817303103195968, -250.9161352504875708 ) ) ;
#33274 = SPHERICAL_SURFACE ( 'NONE', #39690, 1.000000000000000000 ) ;
#33275 = CARTESIAN_POINT ( 'NONE',  ( -24.17631111011271372, -274.7081597337451626, -194.5033055658255137 ) ) ;
#33276 = EDGE_CURVE ( 'NONE', #24966, #2276, #11228, .T. ) ;
#33277 = CARTESIAN_POINT ( 'NONE',  ( -92.91516337080851429, -273.3922917929315304, -223.0069486626450157 ) ) ;
#33278 = EDGE_CURVE ( 'NONE', #79714, #50388, #58090, .T. ) ;
#33279 = CARTESIAN_POINT ( 'NONE',  ( 7.546099883699421085, -282.6406099732241159, -209.7694807524165412 ) ) ;
#33280 = CARTESIAN_POINT ( 'NONE',  ( 0.6090892985368842050, -281.2421122378731297, -336.8069355093072090 ) ) ;
#33281 = CARTESIAN_POINT ( 'NONE',  ( -71.53299156402339065, -276.8405610880930112, -339.2397676284468844 ) ) ;
#33282 = CARTESIAN_POINT ( 'NONE',  ( -108.5848795113629279, -283.5295897961786409, -287.0595393189416882 ) ) ;
#33283 = CARTESIAN_POINT ( 'NONE',  ( 10.31021374610265617, -280.3967150952920520, -328.5604030506088407 ) ) ;
#33284 = CARTESIAN_POINT ( 'NONE',  ( -51.65846654883972633, -272.4402773672729268, -198.1257770416210064 ) ) ;
#33285 = CARTESIAN_POINT ( 'NONE',  ( -100.5170368329778654, -280.0069898695990673, -310.8772668099807674 ) ) ;
#33286 = DIRECTION ( 'NONE',  ( 0.000000000000000000, 0.000000000000000000, 1.000000000000000000 ) ) ;
#33287 = CARTESIAN_POINT ( 'NONE',  ( 209.6287663260175975, 29.00782453271232697, 15.00000000000000000 ) ) ;
#33288 = CARTESIAN_POINT ( 'NONE',  ( -37.23224573514328029, -296.2933724657740981, -194.3737234103267610 ) ) ;
#33289 = CARTESIAN_POINT ( 'NONE',  ( -66.96213998607029794, -279.4396156112838412, -339.4455443851739460 ) ) ;
#33290 = FACE_OUTER_BOUND ( 'NONE', #13464, .T. ) ;
#33291 = CARTESIAN_POINT ( 'NONE',  ( -94.73903062906690309, -287.1486480005538056, -221.1413844251751186 ) ) ;
#33292 = VERTEX_POINT ( 'NONE', #83331 ) ;
#33293 = CARTESIAN_POINT ( 'NONE',  ( 12.07965199447950333, -284.7387967406844496, -213.8789230781245294 ) ) ;
#33294 = CARTESIAN_POINT ( 'NONE',  ( 152.4536156746142410, 250.5000000000000568, -11.99999999999999289 ) ) ;
#33295 = CARTESIAN_POINT ( 'NONE',  ( -95.93051517134986739, -294.7291850124621533, -314.5913427779823337 ) ) ;
#33296 = CARTESIAN_POINT ( 'NONE',  ( -99.89513648522047617, -288.1480376965180312, -310.3352731273910194 ) ) ;
#33297 = CARTESIAN_POINT ( 'NONE',  ( 154.7156223832783724, 20.48904911123736028, -12.57712157663156560 ) ) ;
#33298 = CARTESIAN_POINT ( 'NONE',  ( -93.71022004583248588, -293.8646530673283905, -319.8342481949042053 ) ) ;
#33299 = CARTESIAN_POINT ( 'NONE',  ( -1.279973881134012892, -285.0015678461560924, -203.1133696635105821 ) ) ;
#33300 = CARTESIAN_POINT ( 'NONE',  ( 32.11436023637819659, -283.4826781829265201, -295.4581956494556039 ) ) ;
#33301 = CARTESIAN_POINT ( 'NONE',  ( 36.01273878315765131, -279.5398482319560003, -250.4849618751943012 ) ) ;
#33302 = CARTESIAN_POINT ( 'NONE',  ( -39.95803529557185385, -289.0858085025106448, -343.3637959310983092 ) ) ;
#33303 = CARTESIAN_POINT ( 'NONE',  ( -6.539217865572089394, -281.8900256738776307, -203.5148712634754418 ) ) ;
#33304 = CARTESIAN_POINT ( 'NONE',  ( -14.26762284225651101, -281.1618676301493451, -200.8799844823172975 ) ) ;
#33305 = CARTESIAN_POINT ( 'NONE',  ( 26.07453879285593956, -290.0787510398249651, -311.1610326075498847 ) ) ;
#33306 = CIRCLE ( 'NONE', #36354, 1.000000000000000888 ) ;
#33307 = VERTEX_POINT ( 'NONE', #91371 ) ;
#33308 = CARTESIAN_POINT ( 'NONE',  ( -97.81306561133810362, -273.1897003597648563, -222.6933725293671387 ) ) ;
#33310 = CARTESIAN_POINT ( 'NONE',  ( -98.11486664206425701, -293.1252269755775046, -226.9323422131175789 ) ) ;
#33309 = AXIS2_PLACEMENT_3D ( 'NONE', #86635, #21802, #50676 ) ;
#33311 = PLANE ( 'NONE',  #24242 ) ;
#33312 = CARTESIAN_POINT ( 'NONE',  ( 40.64545035920995986, -289.8376638359844719, -252.5284128619064461 ) ) ;
#33313 = ORIENTED_EDGE ( 'NONE', *, *, #71135, .F. ) ;
#33314 = CARTESIAN_POINT ( 'NONE',  ( -15.15571491175780139, -274.7654898972930368, -342.2335063922344602 ) ) ;
#33315 = DIRECTION ( 'NONE',  ( 1.000000000000000000, 0.000000000000000000, 0.000000000000000000 ) ) ;
#33316 = CARTESIAN_POINT ( 'NONE',  ( -33.49580821277195497, -293.4044070935761965, -346.4769890068221798 ) ) ;
#33317 = CARTESIAN_POINT ( 'NONE',  ( -96.92929790717360561, -296.6496484692112858, -228.0845685411242414 ) ) ;
#33318 = CARTESIAN_POINT ( 'NONE',  ( -78.54620054423907050, -291.1378183172272998, -331.5199785405384318 ) ) ;
#33319 = CARTESIAN_POINT ( 'NONE',  ( -66.94456868883817435, -285.2056502369458713, -338.2102950118643889 ) ) ;
#33320 = CARTESIAN_POINT ( 'NONE',  ( -40.62540460323569391, -293.4369119084665840, -194.0078535165154392 ) ) ;
#33321 = CARTESIAN_POINT ( 'NONE',  ( -53.30289070689140374, -293.1668951046262350, -195.4835838815039040 ) ) ;
#33322 = CARTESIAN_POINT ( 'NONE',  ( -44.23282153925701010, -287.9651449196662725, -195.6783683398700475 ) ) ;
#33323 = CARTESIAN_POINT ( 'NONE',  ( -33.91739589480346240, -280.2607953581726861, -193.4372975818709790 ) ) ;
#33324 = CARTESIAN_POINT ( 'NONE',  ( -91.67877995074051967, -293.8990658326607672, -322.8663172855614221 ) ) ;
#33325 = CARTESIAN_POINT ( 'NONE',  ( -2.894744918062149619, -282.4428947460176573, -339.2409094122591000 ) ) ;
#33326 = CARTESIAN_POINT ( 'NONE',  ( 35.58252660151414659, -277.2323909383133582, -256.4714585798574262 ) ) ;
#33327 = CARTESIAN_POINT ( 'NONE',  ( -37.30987171927208124, -297.5519495502701943, -345.3611179825600175 ) ) ;
#33328 = CARTESIAN_POINT ( 'NONE',  ( -42.74215459161417385, -275.2592040953476271, -345.9332065636634752 ) ) ;
#33329 = CARTESIAN_POINT ( 'NONE',  ( 151.4851178187871312, 15.00000000000000000, 0.000000000000000000 ) ) ;
#33330 = CARTESIAN_POINT ( 'NONE',  ( 19.72801145091433028, -280.4158735269139129, -224.7427394254780211 ) ) ;
#33331 = CARTESIAN_POINT ( 'NONE',  ( -109.3581844763485691, -279.4239997028773246, -296.6243382251321350 ) ) ;
#33332 = CARTESIAN_POINT ( 'NONE',  ( -80.79511299287010218, -284.5373227655552455, -207.0148866303880482 ) ) ;
#33333 = CARTESIAN_POINT ( 'NONE',  ( 21.79006443254570158, -294.6957335035034475, -225.8481037547746837 ) ) ;
#33334 = CARTESIAN_POINT ( 'NONE',  ( 37.15888309450676275, -276.9492518119720330, -254.2962741974701828 ) ) ;
#33335 = CARTESIAN_POINT ( 'NONE',  ( 32.57592333003917417, -277.2663095709509093, -301.4227374096849417 ) ) ;
#33336 = CYLINDRICAL_SURFACE ( 'NONE', #65635, 6.654241149514406040 ) ;
#33337 = CARTESIAN_POINT ( 'NONE',  ( 35.10581063041140482, -275.5090417618965262, -279.7284396159415110 ) ) ;
#33338 = CARTESIAN_POINT ( 'NONE',  ( -56.24235770193362072, -297.2962361136173399, -342.8219490355584753 ) ) ;
#33339 = CARTESIAN_POINT ( 'NONE',  ( -92.86478474100206881, -283.2536745913792515, -220.1131485881716401 ) ) ;
#33340 = CARTESIAN_POINT ( 'NONE',  ( 21.29709704572013607, -292.5461031493408655, -220.4687846005323024 ) ) ;
#33341 = CARTESIAN_POINT ( 'NONE',  ( 38.17965917425229350, -289.0240411683405455, -260.2139654669492757 ) ) ;
#33342 = CARTESIAN_POINT ( 'NONE',  ( 34.52222263106197175, -292.2822080820232031, -255.8765510184112770 ) ) ;
#33343 = ORIENTED_EDGE ( 'NONE', *, *, #50473, .F. ) ;
#33344 = CARTESIAN_POINT ( 'NONE',  ( -53.24879693982099838, -290.4268897770492686, -195.5703648430829276 ) ) ;
#33345 = CARTESIAN_POINT ( 'NONE',  ( -36.20154351210599231, -291.7335187045921430, -197.3363956435701709 ) ) ;
#33346 = ORIENTED_EDGE ( 'NONE', *, *, #35766, .F. ) ;
#33347 = CARTESIAN_POINT ( 'NONE',  ( -71.75538951252248410, -290.5759539253356252, -338.8971704947978765 ) ) ;
#33348 = CARTESIAN_POINT ( 'NONE',  ( -108.5059141385938375, -278.6689131510411812, -286.7793455013163566 ) ) ;
#33349 = CARTESIAN_POINT ( 'NONE',  ( -101.3777752111107446, -294.9142812390116433, -312.6575827542811794 ) ) ;
#33350 = CARTESIAN_POINT ( 'NONE',  ( -103.9563095375059163, -285.7048217864644357, -231.8389788811792585 ) ) ;
#33351 = CARTESIAN_POINT ( 'NONE',  ( -32.31204088466856206, -286.4471958295074501, -193.5335893367187339 ) ) ;
#33352 = CARTESIAN_POINT ( 'NONE',  ( -34.84156663645412522, -283.3532007187520776, -343.3518892696752118 ) ) ;
#33353 = CARTESIAN_POINT ( 'NONE',  ( 167.7576066075372410, 232.6804878302470740, -192.6587424375081241 ) ) ;
#33354 = CARTESIAN_POINT ( 'NONE',  ( -23.37133263859758614, -107.7079578404835019, -361.6456582812304532 ) ) ;
#33355 = CARTESIAN_POINT ( 'NONE',  ( 172.3370473676889389, 241.3813337058840318, -177.2540278754750886 ) ) ;
#33356 = CARTESIAN_POINT ( 'NONE',  ( 28.17055419427044782, -275.1913368517148797, -303.0443929753960788 ) ) ;
#33357 = CARTESIAN_POINT ( 'NONE',  ( -24.28801029419035729, -275.8020263774093905, -342.5503431574682622 ) ) ;
#33358 = CARTESIAN_POINT ( 'NONE',  ( -103.7934878644902739, -296.5659724116084135, -231.4787383676991226 ) ) ;
#33359 = CARTESIAN_POINT ( 'NONE',  ( -37.84230186231246762, -140.7305523473693540, -361.6245629116337454 ) ) ;
#33360 = CARTESIAN_POINT ( 'NONE',  ( 24.09393627825123829, -273.6268531445568897, -224.7654948012895204 ) ) ;
#33361 = CARTESIAN_POINT ( 'NONE',  ( -24.44154745801118267, -275.9790657714007693, -197.4283655155201700 ) ) ;
#33362 = CARTESIAN_POINT ( 'NONE',  ( -36.20080988378119002, -299.0073551978468913, -193.5962329938457174 ) ) ;
#33363 = CARTESIAN_POINT ( 'NONE',  ( 33.76875860297097631, -287.8227272751017267, -253.5353332559716648 ) ) ;
#33364 = CARTESIAN_POINT ( 'NONE',  ( -113.0429952711294419, -297.1861496475119111, -283.8324629488006394 ) ) ;
#33365 = CARTESIAN_POINT ( 'NONE',  ( -107.7192806993222405, -297.4429453158240904, -239.1404177300734659 ) ) ;
#33366 = CARTESIAN_POINT ( 'NONE',  ( -20.84611114343226390, -295.0012953506719100, -341.5250754459366931 ) ) ;
#33367 = EDGE_LOOP ( 'NONE', ( #21365, #84423, #72576, #9380 ) ) ;
#33368 = CARTESIAN_POINT ( 'NONE',  ( 6.381432469543416808, -276.5606396297720835, -208.6722360647949586 ) ) ;
#33369 = EDGE_CURVE ( 'NONE', #63082, #78294, #35443, .T. ) ;
#33370 = VERTEX_POINT ( 'NONE', #48284 ) ;
#33371 = VECTOR ( 'NONE', #77841, 1000.000000000000000 ) ;
#33372 = CARTESIAN_POINT ( 'NONE',  ( -7.555020132883479178, -279.9399520094541458, -199.4082565219720777 ) ) ;
#33373 = CARTESIAN_POINT ( 'NONE',  ( -13.69813227323517779, -277.6789896027577242, -339.7281388262501309 ) ) ;
#33374 = CARTESIAN_POINT ( 'NONE',  ( 33.25128739806281430, -277.6753685026446306, -298.6207676605339998 ) ) ;
#33375 = CARTESIAN_POINT ( 'NONE',  ( -100.7274125782280549, -276.0248484130926840, -311.2075551554477784 ) ) ;
#33376 = CARTESIAN_POINT ( 'NONE',  ( -103.2632956835919629, -273.4701660895620421, -238.8598214874925532 ) ) ;
#33377 = CARTESIAN_POINT ( 'NONE',  ( -109.7249761294971364, -294.9523377310999308, -283.6988825376653836 ) ) ;
#33378 = CARTESIAN_POINT ( 'NONE',  ( 153.1901962297480111, 19.73438857712018901, -11.80184082122067757 ) ) ;
#33379 = EDGE_CURVE ( 'NONE', #46977, #37463, #59652, .T. ) ;
#33380 = CARTESIAN_POINT ( 'NONE',  ( -70.45090325930956965, -277.6680584775729130, -335.4209417799377206 ) ) ;
#33381 = CARTESIAN_POINT ( 'NONE',  ( 28.47094693764329065, -286.7485531986419574, -309.3738563898477310 ) ) ;
#33382 = CARTESIAN_POINT ( 'NONE',  ( -95.40437605516592612, -275.2068316463672772, -222.8676421767180784 ) ) ;
#33383 = CARTESIAN_POINT ( 'NONE',  ( 196.7510731661265595, -141.7221692137691775, 22.50000000000000000 ) ) ;
#33384 = CARTESIAN_POINT ( 'NONE',  ( -97.48747332662306064, -289.1699959026884699, -312.0375157240142130 ) ) ;
#33385 = CARTESIAN_POINT ( 'NONE',  ( -67.14189056295913360, -285.0201669947567780, -199.4720395797210131 ) ) ;
#33386 = CARTESIAN_POINT ( 'NONE',  ( 16.54851465548530598, -280.5131106840119060, -321.1678506186041204 ) ) ;
#33388 = CARTESIAN_POINT ( 'NONE',  ( -111.7594320552299365, -282.5890778349499897, -273.6783914448520250 ) ) ;
#33387 = CARTESIAN_POINT ( 'NONE',  ( 20.63405929242779635, -280.7606380779271831, -315.6842493682204918 ) ) ;
#33389 = CARTESIAN_POINT ( 'NONE',  ( -105.0620966317721212, -286.9778760011843701, -238.0091167032872477 ) ) ;
#33390 = CARTESIAN_POINT ( 'NONE',  ( -104.6293047673641752, -279.3636455854335736, -299.8057892693868780 ) ) ;
#33391 = CARTESIAN_POINT ( 'NONE',  ( 153.7618596668268367, 19.60625832729682827, -12.81530480009370443 ) ) ;
#33392 = CARTESIAN_POINT ( 'NONE',  ( -37.80881650887317136, -294.0464577399726522, -195.3625682920283566 ) ) ;
#33393 = CARTESIAN_POINT ( 'NONE',  ( -73.63287179526206216, -275.7668267350696851, -337.1361288332239496 ) ) ;
#33394 = CARTESIAN_POINT ( 'NONE',  ( 13.80857113568835892, -276.9634322458376232, -322.6575034100913513 ) ) ;
#33395 = CARTESIAN_POINT ( 'NONE',  ( -6.191466573511966942, -284.6439699244017447, -338.7693878016455642 ) ) ;
#33396 = CARTESIAN_POINT ( 'NONE',  ( 196.1824782687554034, 72.66633770555792182, 11.70872282517771623 ) ) ;
#33397 = CARTESIAN_POINT ( 'NONE',  ( -64.89862952135668195, -291.3293071720496528, -340.7721363757398763 ) ) ;
#33398 = CARTESIAN_POINT ( 'NONE',  ( -47.84812007477871987, -293.1854730478466422, -344.6730768276890444 ) ) ;
#33399 = CARTESIAN_POINT ( 'NONE',  ( -3.551126185268555613, -285.6839846275381092, -201.3367944710279858 ) ) ;
#33400 = CARTESIAN_POINT ( 'NONE',  ( -104.2733998130901369, -289.3671544889607503, -239.2711197468755699 ) ) ;
#33401 = CARTESIAN_POINT ( 'NONE',  ( 199.4819116658660221, 63.22432295887224285, -9.188210044104502927 ) ) ;
#33402 = CARTESIAN_POINT ( 'NONE',  ( 35.33180851054449079, -274.0924413248309293, -259.3307870670092825 ) ) ;
#33403 = CARTESIAN_POINT ( 'NONE',  ( -70.29330015517498964, -293.6307662981492967, -336.8822239513026489 ) ) ;
#33404 = LINE ( 'NONE', #5005, #48715 ) ;
#33405 = CARTESIAN_POINT ( 'NONE',  ( 175.2296996224750103, 246.0000000000001137, 0.000000000000000000 ) ) ;
#33406 = CARTESIAN_POINT ( 'NONE',  ( -83.82849895517507832, -289.9071598957123683, -209.7826744868514481 ) ) ;
#33407 = CARTESIAN_POINT ( 'NONE',  ( -109.4509030911634113, -286.3580056145656840, -254.5952550540395691 ) ) ;
#33408 = CARTESIAN_POINT ( 'NONE',  ( -59.75011279072997183, -287.5784065720295644, -342.9685353296794119 ) ) ;
#33409 = CARTESIAN_POINT ( 'NONE',  ( -110.0058226546812534, -286.1306901084002448, -258.6493158258560925 ) ) ;
#33410 = LINE ( 'NONE', #12106, #19932 ) ;
#33411 = CARTESIAN_POINT ( 'NONE',  ( -27.82564950983397978, -286.9789246063949690, -197.8211530850211375 ) ) ;
#33412 = CARTESIAN_POINT ( 'NONE',  ( 30.75471345333757611, -295.9559806990986317, -302.7517930220674316 ) ) ;
#33413 = CARTESIAN_POINT ( 'NONE',  ( -111.6539567952122383, -276.4568111293946231, -284.1072218640710503 ) ) ;
#33414 = CARTESIAN_POINT ( 'NONE',  ( -14.59189161570405879, -277.0985558225172554, -343.9573297104967082 ) ) ;
#33415 = CARTESIAN_POINT ( 'NONE',  ( 18.37075984491076497, -290.9243867938927224, -219.3176462902255537 ) ) ;
#33416 = CARTESIAN_POINT ( 'NONE',  ( -72.88608535875843586, -297.5053259332333937, -336.0144408177023365 ) ) ;
#33417 = PLANE ( 'NONE',  #7625 ) ;
#33418 = DIRECTION ( 'NONE',  ( -0.000000000000000000, -0.000000000000000000, -1.000000000000000000 ) ) ;
#33419 = CARTESIAN_POINT ( 'NONE',  ( -41.33307833562736278, -284.6857060914168756, -196.9638474514909490 ) ) ;
#33420 = CARTESIAN_POINT ( 'NONE',  ( -83.79789167289104057, -275.8368963041938287, -328.3296919027622494 ) ) ;
#33421 = CARTESIAN_POINT ( 'NONE',  ( 37.42014773041214681, -279.4753064729031280, -264.3889532623327341 ) ) ;
#33422 = CARTESIAN_POINT ( 'NONE',  ( 26.36249097817102438, -273.4746662289535379, -228.3553589978261016 ) ) ;
#33423 = CARTESIAN_POINT ( 'NONE',  ( -109.5940716521211158, -277.7543482192563715, -281.4736099366369331 ) ) ;
#33424 = CARTESIAN_POINT ( 'NONE',  ( 35.98316140142789266, -294.9696724109267052, -262.5089811743219457 ) ) ;
#33425 = CARTESIAN_POINT ( 'NONE',  ( 29.02598759336025225, -279.9707319588878249, -231.9316691758452293 ) ) ;
#33426 = CARTESIAN_POINT ( 'NONE',  ( -66.13464146498840535, -296.3797774291025462, -337.6988858231425752 ) ) ;
#33427 = CARTESIAN_POINT ( 'NONE',  ( -36.56380722448715659, -299.3768667954376497, -193.8540952940258251 ) ) ;
#33428 = CARTESIAN_POINT ( 'NONE',  ( -81.94243939126651810, -297.2584655173567967, -212.5062755757392665 ) ) ;
#33429 = CARTESIAN_POINT ( 'NONE',  ( -33.42888667534835889, -294.1015478314944858, -195.4504159624086412 ) ) ;
#33430 = CARTESIAN_POINT ( 'NONE',  ( -23.78799208008210186, -286.3872846946402433, -194.5091640045761778 ) ) ;
#33431 = CARTESIAN_POINT ( 'NONE',  ( 36.96621835176514281, -273.8796806781463715, -285.1475554983709344 ) ) ;
#33432 = CARTESIAN_POINT ( 'NONE',  ( 23.28614635133079247, -288.0201669887010212, -317.8509082516174544 ) ) ;
#33433 = CARTESIAN_POINT ( 'NONE',  ( -110.5043173665690830, -280.7238243642296993, -255.4955348153288242 ) ) ;
#33434 = CARTESIAN_POINT ( 'NONE',  ( 32.50159205227141967, -286.3193089501468762, -248.2890646920061499 ) ) ;
#33435 = CARTESIAN_POINT ( 'NONE',  ( -111.1692149113089130, -288.3814470610126364, -283.6435902144257284 ) ) ;
#33436 = ORIENTED_EDGE ( 'NONE', *, *, #72628, .F. ) ;
#33437 = CARTESIAN_POINT ( 'NONE',  ( 199.4897031045222775, 67.51130003612513519, 8.507168327817714371 ) ) ;
#33438 = CARTESIAN_POINT ( 'NONE',  ( 3.643948319138460956, -287.9921339471291617, -330.9048860672280057 ) ) ;
#33439 = CARTESIAN_POINT ( 'NONE',  ( 208.2200286604726500, 29.14932976030723211, 13.33523498126286455 ) ) ;
#33440 = CARTESIAN_POINT ( 'NONE',  ( -111.4970665104632133, -285.7448970575715634, -250.3167702164104185 ) ) ;
#33441 = CARTESIAN_POINT ( 'NONE',  ( -108.5845629321353982, -289.2469886099032124, -298.9491349106299367 ) ) ;
#33442 = CARTESIAN_POINT ( 'NONE',  ( 38.48421450496085328, -283.2540423829130418, -278.4135232348953082 ) ) ;
#33443 = CARTESIAN_POINT ( 'NONE',  ( -42.41418810748496071, -281.3046040939788668, -194.0226077879337083 ) ) ;
#33444 = CARTESIAN_POINT ( 'NONE',  ( 33.11413949807556634, -281.1325359539231385, -251.2089778662260358 ) ) ;
#33445 = CARTESIAN_POINT ( 'NONE',  ( 34.77629713433318415, -277.2851623698398953, -249.5846316465301413 ) ) ;
#33446 = CARTESIAN_POINT ( 'NONE',  ( -13.78204409039318001, -294.7546166827933121, -343.6682977631642188 ) ) ;
#33447 = CARTESIAN_POINT ( 'NONE',  ( -93.66913903925652107, -287.8886563336205882, -319.4186595398954864 ) ) ;
#33448 = EDGE_CURVE ( 'NONE', #38700, #93199, #74701, .T. ) ;
#33449 = CARTESIAN_POINT ( 'NONE',  ( -105.7809614688212037, -271.7011620353396211, -243.7031169602172156 ) ) ;
#33450 = ORIENTED_EDGE ( 'NONE', *, *, #65327, .F. ) ;
#33451 = EDGE_LOOP ( 'NONE', ( #31191, #25859, #3310, #74688 ) ) ;
#33452 = CARTESIAN_POINT ( 'NONE',  ( -98.70580278528265694, -285.8959690187934370, -312.5906964755948820 ) ) ;
#33453 = CARTESIAN_POINT ( 'NONE',  ( 36.07778864208916758, -294.9131285602464914, -292.7012493243549898 ) ) ;
#33454 = CARTESIAN_POINT ( 'NONE',  ( -21.35785909716079800, -283.4932570154115865, -341.7462929848896920 ) ) ;
#33455 = CARTESIAN_POINT ( 'NONE',  ( -1.587978628988057528, -275.6486949334394012, -338.2911673900875371 ) ) ;
#33456 = CARTESIAN_POINT ( 'NONE',  ( -114.2670865423148143, -291.2285534235827527, -268.3656461346440665 ) ) ;
#33457 = CARTESIAN_POINT ( 'NONE',  ( -113.1202429249092631, -282.6609183111559105, -272.7856826508978543 ) ) ;
#33458 = CARTESIAN_POINT ( 'NONE',  ( 26.47299462915980683, -293.3169465550612927, -227.2158876293997878 ) ) ;
#33459 = CARTESIAN_POINT ( 'NONE',  ( -101.6597603038106712, -290.4128301107849097, -305.0410555933581804 ) ) ;
#33460 = CARTESIAN_POINT ( 'NONE',  ( 184.1778392089217107, 3.000000000000000888, 9.000000000000001776 ) ) ;
#33461 = CARTESIAN_POINT ( 'NONE',  ( 153.2628468892384603, 20.37991841447901820, 11.93555113919330424 ) ) ;
#33462 = CARTESIAN_POINT ( 'NONE',  ( -21.17153989118013158, -109.2489533316710464, -359.0337785304685667 ) ) ;
#33463 = CARTESIAN_POINT ( 'NONE',  ( -64.98282404026691950, -284.9268695719707125, -341.4995623601482748 ) ) ;
#33464 = CARTESIAN_POINT ( 'NONE',  ( -4.829096099716524648, -292.1237833571632905, -337.9475929042657754 ) ) ;
#33465 = VERTEX_POINT ( 'NONE', #84738 ) ;
#33466 = CARTESIAN_POINT ( 'NONE',  ( 35.99694277239871099, -280.4492057680265020, -268.5897685596444262 ) ) ;
#33467 = CARTESIAN_POINT ( 'NONE',  ( 30.52242004692138622, -275.6898842619803531, -306.8082895407610522 ) ) ;
#33468 = CARTESIAN_POINT ( 'NONE',  ( -95.37810012770053447, -281.2045895927852825, -223.1191376488047240 ) ) ;
#33469 = CARTESIAN_POINT ( 'NONE',  ( -45.93041767256378449, -156.1281930031302068, -363.3478848798407626 ) ) ;
#33470 = CARTESIAN_POINT ( 'NONE',  ( 10.46857768926897592, -279.2719313653462336, -210.6880551476552625 ) ) ;
#33471 = CARTESIAN_POINT ( 'NONE',  ( -112.0365078248271260, -282.5653471247208586, -270.8964869736045102 ) ) ;
#33472 = CARTESIAN_POINT ( 'NONE',  ( -95.99516178219309381, -275.0671097645934537, -222.3817486476455372 ) ) ;
#33473 = CARTESIAN_POINT ( 'NONE',  ( -88.54050398348223894, -296.2860443105471973, -322.5539042674809593 ) ) ;
#33474 = VERTEX_POINT ( 'NONE', #5237 ) ;
#33475 = CARTESIAN_POINT ( 'NONE',  ( -100.1242550243702709, -289.7596351732216817, -232.1564811165874573 ) ) ;
#33476 = CARTESIAN_POINT ( 'NONE',  ( -9.241333025187392636, -277.3456664461765513, -341.9410184804669370 ) ) ;
#33477 = CARTESIAN_POINT ( 'NONE',  ( -5.308056246438822789, -274.4858272961020589, -204.7512142507426347 ) ) ;
#33478 = CARTESIAN_POINT ( 'NONE',  ( 35.44097946285869938, -274.1651124572006779, -246.0239343167204140 ) ) ;
#33479 = DIRECTION ( 'NONE',  ( 0.9531768234071980039, -0.3024135303179465439, 1.282457197809570761E-15 ) ) ;
#33480 = CARTESIAN_POINT ( 'NONE',  ( -111.5704608358709891, -270.6942485587154579, -259.2817424984529566 ) ) ;
#33481 = EDGE_CURVE ( 'NONE', #21372, #3443, #34109, .T. ) ;
#33482 = CYLINDRICAL_SURFACE ( 'NONE', #5238, 5.103083949679981579 ) ;
#33483 = CARTESIAN_POINT ( 'NONE',  ( -43.52491939661445031, -249.8948216656541774, -483.9534721554022667 ) ) ;
#33484 = CARTESIAN_POINT ( 'NONE',  ( 35.65880787313304268, -282.5365407540246565, -263.1071437057715912 ) ) ;
#33485 = CARTESIAN_POINT ( 'NONE',  ( 25.11044511923328670, -283.8919668631231161, -313.6703089757065186 ) ) ;
#33486 = CARTESIAN_POINT ( 'NONE',  ( -108.8214824896591892, -283.6982118289224104, -285.7350846272551053 ) ) ;
#33487 = CARTESIAN_POINT ( 'NONE',  ( 21.46215340906459446, -274.5719250932676232, -314.9542477927584514 ) ) ;
#33488 = CARTESIAN_POINT ( 'NONE',  ( 36.92249123114469000, -283.3888200197109768, -268.5298594868648934 ) ) ;
#33489 = CARTESIAN_POINT ( 'NONE',  ( -32.39315626288333050, -275.4686443762308272, -343.9385588584381708 ) ) ;
#33490 = CARTESIAN_POINT ( 'NONE',  ( 185.1905923765118587, 250.0000000000000568, 21.83530662808691147 ) ) ;
#33491 = CARTESIAN_POINT ( 'NONE',  ( 35.95166978979703032, -276.6118735473925767, -268.8419080778610919 ) ) ;
#33492 = DIRECTION ( 'NONE',  ( 0.000000000000000000, 1.000000000000000000, 0.000000000000000000 ) ) ;
#33493 = CARTESIAN_POINT ( 'NONE',  ( -59.26586970594906489, -280.5781960372398771, -196.7167725893437762 ) ) ;
#33494 = ORIENTED_EDGE ( 'NONE', *, *, #59139, .F. ) ;
#33495 = DIRECTION ( 'NONE',  ( -2.265761274745217776E-15, 0.000000000000000000, 1.000000000000000000 ) ) ;
#33496 = CARTESIAN_POINT ( 'NONE',  ( -36.60168210301413438, -287.9217569565474832, -194.5870990019050168 ) ) ;
#33497 = CARTESIAN_POINT ( 'NONE',  ( -42.41109624394971434, -294.3148843736417462, -343.3467532140356298 ) ) ;
#33498 = EDGE_CURVE ( 'NONE', #87978, #44024, #30904, .T. ) ;
#33499 = CARTESIAN_POINT ( 'NONE',  ( -100.6014699525223079, -289.3225988504343036, -314.0819860938323700 ) ) ;
#33500 = CARTESIAN_POINT ( 'NONE',  ( 22.82830041259893150, -285.1968662942176138, -227.1754310312921916 ) ) ;
#33502 = CARTESIAN_POINT ( 'NONE',  ( -92.41235757496139058, -289.4902427952504240, -220.8932383347653570 ) ) ;
#33501 = CARTESIAN_POINT ( 'NONE',  ( -11.80059340024893899, -284.9660469232246669, -201.3464327038570900 ) ) ;
#33503 = CARTESIAN_POINT ( 'NONE',  ( -105.5774482385071451, -285.3958661654552316, -297.5366490133638422 ) ) ;
#33504 = CARTESIAN_POINT ( 'NONE',  ( 17.42490343750725046, -274.2695623518728212, -321.6019199178481358 ) ) ;
#33505 = VECTOR ( 'NONE', #76127, 1000.000000000000000 ) ;
#33506 = CARTESIAN_POINT ( 'NONE',  ( -30.93063966012798360, -284.5317392400209542, -194.4181336177512378 ) ) ;
#33507 = CARTESIAN_POINT ( 'NONE',  ( -40.38528535353915316, -300.0141807748269116, -195.3721238207088504 ) ) ;
#33508 = CARTESIAN_POINT ( 'NONE',  ( 20.96647093977610510, -286.2041736542307149, -317.8174870631714839 ) ) ;
#33509 = CARTESIAN_POINT ( 'NONE',  ( -43.78369384797323249, -280.9101416243232165, -197.3593056544557669 ) ) ;
#33510 = CARTESIAN_POINT ( 'NONE',  ( -31.93265467183951856, -290.9843433520939584, -345.3842212363069279 ) ) ;
#33511 = CARTESIAN_POINT ( 'NONE',  ( 189.4188515237862589, 293.9636489450775798, 13.99999999999999112 ) ) ;
#33512 = CARTESIAN_POINT ( 'NONE',  ( 195.4525831896995953, 39.48772993134988241, 14.00000000000000533 ) ) ;
#33513 = CARTESIAN_POINT ( 'NONE',  ( -91.64479744948833684, -297.7387546211278391, -322.9014626598053042 ) ) ;
#33514 = CIRCLE ( 'NONE', #13872, 5.000000000000000888 ) ;
#33515 = CARTESIAN_POINT ( 'NONE',  ( -46.68092246048014005, -277.9335628596838319, -195.8923586338238181 ) ) ;
#33516 = CARTESIAN_POINT ( 'NONE',  ( 34.31595104981452948, -292.3955499653098400, -242.4770524530541138 ) ) ;
#33517 = CARTESIAN_POINT ( 'NONE',  ( -105.4932675079784872, -295.3276378690839010, -242.0449692854151920 ) ) ;
#33518 = CARTESIAN_POINT ( 'NONE',  ( 33.93795780632670755, -280.0017083555510453, -252.4087159367159927 ) ) ;
#33519 = CARTESIAN_POINT ( 'NONE',  ( 34.91269352859074360, -273.4002870889214591, -252.4553424217140787 ) ) ;
#33520 = CARTESIAN_POINT ( 'NONE',  ( 31.28293176319303015, -294.5183756526157595, -244.0570617375843199 ) ) ;
#33521 = CARTESIAN_POINT ( 'NONE',  ( -69.91165696735023971, -300.1233781216987495, -202.8022627189028810 ) ) ;
#33522 = CARTESIAN_POINT ( 'NONE',  ( -102.5333889694384197, -294.5095055384285843, -310.0190485595027212 ) ) ;
#33523 = CARTESIAN_POINT ( 'NONE',  ( -30.70211858851053321, -293.2091590906264287, -346.0571546714827491 ) ) ;
#33524 = CARTESIAN_POINT ( 'NONE',  ( -94.76198562876894016, -292.6228495563988190, -224.3162502132267946 ) ) ;
#33525 = LINE ( 'NONE', #62431, #41472 ) ;
#33526 = CARTESIAN_POINT ( 'NONE',  ( -98.44001350465183009, -291.9129763238455553, -230.0248489907159239 ) ) ;
#33527 = CARTESIAN_POINT ( 'NONE',  ( 180.6209651459523968, 275.0000000000000568, -24.41176470588238701 ) ) ;
#33529 = CARTESIAN_POINT ( 'NONE',  ( 35.64194322172812690, -293.5934137414293446, -273.4889707359823774 ) ) ;
#33528 = CARTESIAN_POINT ( 'NONE',  ( -100.0643908004630305, -282.0095242350653280, -312.2192592017375432 ) ) ;
#33530 = CARTESIAN_POINT ( 'NONE',  ( 10.82300856513808363, -280.6969743179029706, -210.2164851128124212 ) ) ;
#33531 = CARTESIAN_POINT ( 'NONE',  ( -101.4039048203670745, -283.6558696384626046, -313.1390636979091937 ) ) ;
#33532 = CARTESIAN_POINT ( 'NONE',  ( -85.89337988077159025, -287.7258796903413440, -327.3747957183749691 ) ) ;
#33533 = CARTESIAN_POINT ( 'NONE',  ( -96.92711670422742998, -282.0810474347836134, -314.6380150509479563 ) ) ;
#33534 = CARTESIAN_POINT ( 'NONE',  ( 159.4851178187871312, 3.000000000000000000, -10.00000000000000000 ) ) ;
#33535 = CARTESIAN_POINT ( 'NONE',  ( -50.79817612958569129, -278.3631099662396196, -195.2503264498887461 ) ) ;
#33536 = CARTESIAN_POINT ( 'NONE',  ( 35.55951303419863763, -286.1698025707267448, -246.3814091679362548 ) ) ;
#33537 = CARTESIAN_POINT ( 'NONE',  ( 196.3508760566247418, 41.60265626164483876, 13.80739217974186595 ) ) ;
#33538 = CARTESIAN_POINT ( 'NONE',  ( 26.49475910102298570, -295.6548031923206281, -307.3928190887405094 ) ) ;
#33539 = CARTESIAN_POINT ( 'NONE',  ( 22.19342012054821467, -277.6244730557907587, -318.2793755749885349 ) ) ;
#33540 = CARTESIAN_POINT ( 'NONE',  ( -87.11304259547296169, -277.4355641407343001, -323.7923911819154910 ) ) ;
#33541 = CARTESIAN_POINT ( 'NONE',  ( -58.94071754505114313, -291.9468757793724194, -196.4525092071985739 ) ) ;
#33542 = CARTESIAN_POINT ( 'NONE',  ( -35.95069252803639870, -281.1147194441184638, -345.9211890928669959 ) ) ;
#33543 = CARTESIAN_POINT ( 'NONE',  ( 34.94812936448611396, -292.4556254315568822, -258.5527877890277750 ) ) ;
#33544 = CARTESIAN_POINT ( 'NONE',  ( -105.3634549566303207, -294.1369017799314065, -301.9529130517282738 ) ) ;
#33545 = ORIENTED_EDGE ( 'NONE', *, *, #24191, .F. ) ;
#33546 = DIRECTION ( 'NONE',  ( 0.000000000000000000, 0.000000000000000000, -1.000000000000000000 ) ) ;
#33547 = CARTESIAN_POINT ( 'NONE',  ( 3.845913698009563841, -293.9884226659847855, -330.7065313031921505 ) ) ;
#33548 = DIRECTION ( 'NONE',  ( -0.000000000000000000, -0.000000000000000000, 1.000000000000000000 ) ) ;
#33549 = CARTESIAN_POINT ( 'NONE',  ( -105.5795714935544112, -288.2666405000203440, -254.7536222014695397 ) ) ;
#33550 = CARTESIAN_POINT ( 'NONE',  ( -60.06696186555931405, -296.8235170907243514, -196.9819479541712610 ) ) ;
#33551 = CARTESIAN_POINT ( 'NONE',  ( 37.44471777992286121, -279.8470267678326877, -282.5786095512858651 ) ) ;
#33552 = CARTESIAN_POINT ( 'NONE',  ( 24.29596346786136962, -288.2613957561225106, -225.0389743856972871 ) ) ;
#33553 = CARTESIAN_POINT ( 'NONE',  ( -37.27014957742278511, -288.8845514035576230, -343.3610829487153069 ) ) ;
#33554 = CARTESIAN_POINT ( 'NONE',  ( -107.7735877262127531, -279.7857744234878510, -292.2126405768848372 ) ) ;
#33555 = CARTESIAN_POINT ( 'NONE',  ( -109.5673363045812181, -294.3282902113879800, -289.2612382266176496 ) ) ;
#33556 = CARTESIAN_POINT ( 'NONE',  ( -103.6664114205074299, -297.8717295870629300, -303.3251021515311550 ) ) ;
#33557 = CARTESIAN_POINT ( 'NONE',  ( -97.98551098742142074, -276.7749808841734307, -311.7067188312922212 ) ) ;
#33558 = ORIENTED_EDGE ( 'NONE', *, *, #28307, .F. ) ;
#33559 = CARTESIAN_POINT ( 'NONE',  ( -65.53030855817522138, -297.3603538583422505, -198.6721232773958832 ) ) ;
#33560 = CARTESIAN_POINT ( 'NONE',  ( -70.59414612453876714, -291.4142152710654727, -336.9754656033932747 ) ) ;
#33561 = CARTESIAN_POINT ( 'NONE',  ( 28.77132586717855034, -294.6548244913639678, -232.4730168480541010 ) ) ;
#33562 = PLANE ( 'NONE',  #73301 ) ;
#33563 = ADVANCED_FACE ( 'NONE', ( #33622 ), #77187, .F. ) ;
#33564 = CARTESIAN_POINT ( 'NONE',  ( 1.372587174990538506, -289.1712858943852780, -332.3699611157591676 ) ) ;
#33565 = CARTESIAN_POINT ( 'NONE',  ( -48.18343439339133027, -256.9970711660205325, -450.6082928460551216 ) ) ;
#33566 = ORIENTED_EDGE ( 'NONE', *, *, #78869, .F. ) ;
#33567 = CARTESIAN_POINT ( 'NONE',  ( -113.1019969162496892, -297.0347547378974582, -283.8409921459889915 ) ) ;
#33568 = CARTESIAN_POINT ( 'NONE',  ( -111.6610807558444094, -288.5036978710386961, -285.1556981684919947 ) ) ;
#33569 = CARTESIAN_POINT ( 'NONE',  ( -73.27453619583678801, -297.9225736999538299, -202.2245691154867302 ) ) ;
#33570 = CIRCLE ( 'NONE', #16951, 1.000000000000006439 ) ;
#33571 = CARTESIAN_POINT ( 'NONE',  ( -18.20453976106250948, -63.49190233628851132, 22.50000000000000000 ) ) ;
#33572 = AXIS2_PLACEMENT_3D ( 'NONE', #3361, #2900, #31783 ) ;
#33573 = CARTESIAN_POINT ( 'NONE',  ( 195.4781563537916895, 27.48493576247232895, 15.00000000000008882 ) ) ;
#33574 = CARTESIAN_POINT ( 'NONE',  ( 21.87941867036990828, -289.7238863253596151, -318.5020260311712832 ) ) ;
#33575 = CARTESIAN_POINT ( 'NONE',  ( -88.52914483777347243, -275.9090924074130271, -206.2264541496106460 ) ) ;
#33576 = CARTESIAN_POINT ( 'NONE',  ( 38.15619258392178637, -280.7178121307047718, -255.7535520339510526 ) ) ;
#33577 = CARTESIAN_POINT ( 'NONE',  ( -103.8798540636037586, -287.0064152887067053, -236.1163739430591875 ) ) ;
#33578 = CARTESIAN_POINT ( 'NONE',  ( -23.87180051405622905, -284.7955885954241921, -195.0931656201879605 ) ) ;
#33579 = CARTESIAN_POINT ( 'NONE',  ( -49.13997931962696697, -271.9014379775259727, -196.4112388732575596 ) ) ;
#33580 = CARTESIAN_POINT ( 'NONE',  ( -51.86589950027864404, -275.7851653991967851, -197.2989762936699663 ) ) ;
#33582 = CARTESIAN_POINT ( 'NONE',  ( -92.72854861731995868, -289.3302557942081989, -220.6066478652665523 ) ) ;
#33581 = AXIS2_PLACEMENT_3D ( 'NONE', #79211, #72115, #7231 ) ;
#33583 = CARTESIAN_POINT ( 'NONE',  ( -113.1425260752796902, -280.4326150102098723, -268.7839863158469029 ) ) ;
#33584 = EDGE_LOOP ( 'NONE', ( #55456, #38731, #86592, #87155 ) ) ;
#33586 = CARTESIAN_POINT ( 'NONE',  ( 20.60180239076771258, -280.2741367026085300, -225.7712379358224268 ) ) ;
#33585 = CARTESIAN_POINT ( 'NONE',  ( 2.703984594086757731, -280.6055182956760063, -209.2648739963373998 ) ) ;
#33587 = CARTESIAN_POINT ( 'NONE',  ( 34.91438619334918059, -276.9592642898892905, -296.2189058253874805 ) ) ;
#33588 = CARTESIAN_POINT ( 'NONE',  ( 30.37800443713192777, -279.8810531732180493, -234.4422591463007564 ) ) ;
#33589 = CARTESIAN_POINT ( 'NONE',  ( -109.6225879400218872, -263.9640009610400853, -305.6697541383538237 ) ) ;
#33590 = CARTESIAN_POINT ( 'NONE',  ( 36.35656919146170196, -276.2210926640910884, -248.6955815581138154 ) ) ;
#33591 = ITEM_DEFINED_TRANSFORMATION ( 'NONE', 'NONE', #53680,  #18940 ) ;
#33592 = CARTESIAN_POINT ( 'NONE',  ( -34.80219443597819406, -299.5086240258658563, -193.9497409019863028 ) ) ;
#33593 = EDGE_CURVE ( 'NONE', #9910, #64985, #55100, .T. ) ;
#33594 = CARTESIAN_POINT ( 'NONE',  ( -4.771743288812468897, -285.1233781216987495, -337.9199732462171255 ) ) ;
#33595 = VERTEX_POINT ( 'NONE', #13276 ) ;
#33596 = DIRECTION ( 'NONE',  ( 0.000000000000000000, 0.000000000000000000, 1.000000000000000000 ) ) ;
#33597 = CARTESIAN_POINT ( 'NONE',  ( 3.799404484734379306, -289.5638994157276329, -331.0988193956028454 ) ) ;
#33598 = CARTESIAN_POINT ( 'NONE',  ( 20.72929455207008331, -289.9812843131265936, -319.3686030540673642 ) ) ;
#33599 = CARTESIAN_POINT ( 'NONE',  ( -70.02547447582276163, -288.8430648307809747, -335.7635557315431925 ) ) ;
#33600 = CARTESIAN_POINT ( 'NONE',  ( -40.80741904840011358, -285.5174441916616388, -193.4486014770332929 ) ) ;
#33601 = CARTESIAN_POINT ( 'NONE',  ( -76.76918040625621131, -209.2117619618190929, -357.1497412455196354 ) ) ;
#33602 = CARTESIAN_POINT ( 'NONE',  ( 35.93156225681961757, -280.0722878596320129, -279.5781497160837148 ) ) ;
#33603 = CARTESIAN_POINT ( 'NONE',  ( 36.68558903127784276, -289.4930043250041649, -276.5613092504442534 ) ) ;
#33604 = CARTESIAN_POINT ( 'NONE',  ( 18.11395929613510347, -280.7180154664252427, -318.8933504824460101 ) ) ;
#33605 = CARTESIAN_POINT ( 'NONE',  ( -71.18355912115484330, -280.9108686451132826, -205.1091223539073098 ) ) ;
#33606 = CARTESIAN_POINT ( 'NONE',  ( -8.708786258203033981, -277.1594643278485819, -337.5918182459787431 ) ) ;
#33607 = CARTESIAN_POINT ( 'NONE',  ( -103.4634812553831864, -288.8399084798168133, -309.1431809583249333 ) ) ;
#33608 = CARTESIAN_POINT ( 'NONE',  ( -91.79577878998694018, -286.1021707033149823, -216.1493836683731047 ) ) ;
#33609 = CARTESIAN_POINT ( 'NONE',  ( -111.6634124857076245, -285.2960648011215312, -250.2658429835092306 ) ) ;
#33610 = CARTESIAN_POINT ( 'NONE',  ( 33.94087426313222977, -281.9264890973526008, -286.1026106912966043 ) ) ;
#33611 = VERTEX_POINT ( 'NONE', #91842 ) ;
#33612 = CARTESIAN_POINT ( 'NONE',  ( 169.2494399300530290, 8.542400036368780647, 9.974999999999996092 ) ) ;
#33613 = CARTESIAN_POINT ( 'NONE',  ( -104.0569247897468443, -291.9407146101873423, -306.2691153697310824 ) ) ;
#33614 =( BOUNDED_CURVE ( )  B_SPLINE_CURVE ( 3, ( #32149, #54380, #47259, #3743 ),
 .UNSPECIFIED., .F., .F. ) 
 B_SPLINE_CURVE_WITH_KNOTS ( ( 4, 4 ),
 ( 1.570796326794896558, 3.141592653589793116 ),
 .UNSPECIFIED. ) 
 CURVE ( )  GEOMETRIC_REPRESENTATION_ITEM ( )  RATIONAL_B_SPLINE_CURVE ( ( 1.000000000000000000, 0.8047378541243649375, 0.8047378541243649375, 1.000000000000000000 ) ) 
 REPRESENTATION_ITEM ( '' )  );
#33615 = CARTESIAN_POINT ( 'NONE',  ( 6.229211675588853581, -291.3150797694533480, -207.4733296905254178 ) ) ;
#33616 = CARTESIAN_POINT ( 'NONE',  ( 33.12097590376699685, -274.8744770714257015, -290.3674372353284525 ) ) ;
#33617 = EDGE_CURVE ( 'NONE', #1567, #35945, #38450, .T. ) ;
#33618 = CARTESIAN_POINT ( 'NONE',  ( -93.62053362882431884, -295.1853100060159250, -322.7828581877265606 ) ) ;
#33619 = CARTESIAN_POINT ( 'NONE',  ( -49.78694387216549444, -290.3705441428924132, -197.6744412394347421 ) ) ;
#33620 = CARTESIAN_POINT ( 'NONE',  ( -42.48217194291863308, -293.3577302635454203, -344.1957275069991624 ) ) ;
#33621 = CARTESIAN_POINT ( 'NONE',  ( -88.92930951457302058, -291.0021749139226586, -322.5707824346350776 ) ) ;
#33622 = FACE_OUTER_BOUND ( 'NONE', #60401, .T. ) ;
#33623 = CARTESIAN_POINT ( 'NONE',  ( -93.93204246742143937, -291.8692315442620497, -319.5803602048571292 ) ) ;
#33624 = CARTESIAN_POINT ( 'NONE',  ( 35.31769813155879234, -291.7988961752489558, -289.6131379771490515 ) ) ;
#33625 = CARTESIAN_POINT ( 'NONE',  ( 4.835301026201904051, -296.4830329575373185, -332.4397731466709729 ) ) ;
#33626 = CARTESIAN_POINT ( 'NONE',  ( -73.68277161649744755, -286.4983424837704433, -206.7640687634293499 ) ) ;
#33627 = CARTESIAN_POINT ( 'NONE',  ( 36.00084614671346372, -295.7639170392411074, -286.8783198665047962 ) ) ;
#33628 = CARTESIAN_POINT ( 'NONE',  ( 31.04944341120724616, -277.1169673663370645, -238.5974423883914994 ) ) ;
#33629 = CARTESIAN_POINT ( 'NONE',  ( 25.73116992351905807, -274.9250401541016231, -313.9249831452214039 ) ) ;
#33630 = CARTESIAN_POINT ( 'NONE',  ( -23.38597822280161154, -297.4198807086748957, -193.5244381569562506 ) ) ;
#33631 = CARTESIAN_POINT ( 'NONE',  ( 8.186328144667884388, -274.6599255679947760, -328.7802653937671380 ) ) ;
#33632 = CARTESIAN_POINT ( 'NONE',  ( -97.55640773327610304, -277.2327012847827632, -226.5946560763432558 ) ) ;
#33633 = CARTESIAN_POINT ( 'NONE',  ( 52.40925428718954748, -300.5139553254558109, -196.8474091074338332 ) ) ;
#33634 = ADVANCED_FACE ( 'NONE', ( #85220 ), #4278, .T. ) ;
#33635 = CARTESIAN_POINT ( 'NONE',  ( -86.87328784996806519, -297.1830022178324384, -324.7853472705846798 ) ) ;
#33636 = CARTESIAN_POINT ( 'NONE',  ( 201.2509219215139922, 65.09645894978945080, 0.000000000000000000 ) ) ;
#33637 = CARTESIAN_POINT ( 'NONE',  ( -97.02036411700407825, -297.9446190521592825, -228.0402154435760451 ) ) ;
#33638 = DIRECTION ( 'NONE',  ( 4.095251346825558428E-15, -1.000000000000000000, 0.000000000000000000 ) ) ;
#33639 = AXIS2_PLACEMENT_3D ( 'NONE', #75079, #88337, #53766 ) ;
#33641 = CARTESIAN_POINT ( 'NONE',  ( -104.3788646822989108, -272.7753129095747227, -241.3363363248622591 ) ) ;
#33640 = CARTESIAN_POINT ( 'NONE',  ( -69.95063100753816343, -287.4995286371100747, -338.3095616981197509 ) ) ;
#33642 = CARTESIAN_POINT ( 'NONE',  ( 12.07757810788665331, -286.7172453998858828, -211.2429610981553765 ) ) ;
#33643 = CARTESIAN_POINT ( 'NONE',  ( -5.639080900124533891, -288.3132061691605941, -340.5087353740714775 ) ) ;
#33644 = CARTESIAN_POINT ( 'NONE',  ( -106.2787521760149048, -298.9302509307642595, -239.8002878759974692 ) ) ;
#33645 = CARTESIAN_POINT ( 'NONE',  ( 35.21759690324666536, -291.7876982258098337, -288.6689535812006397 ) ) ;
#33646 = AXIS2_PLACEMENT_3D ( 'NONE', #75225, #10339, #89876 ) ;
#33647 = CARTESIAN_POINT ( 'NONE',  ( 23.26922539889932651, -281.3818258528739307, -317.6102767978092061 ) ) ;
#33648 = DIRECTION ( 'NONE',  ( 0.000000000000000000, 0.000000000000000000, 1.000000000000000000 ) ) ;
#33649 = AXIS2_PLACEMENT_3D ( 'NONE', #15448, #72747, #7868 ) ;
#33650 = CARTESIAN_POINT ( 'NONE',  ( 18.85470292168867346, -278.8607530831927193, -220.6167120060577815 ) ) ;
#33651 = CARTESIAN_POINT ( 'NONE',  ( 197.4046495284674165, 214.9970011440366875, -12.46212327005319587 ) ) ;
#33652 = CARTESIAN_POINT ( 'NONE',  ( -34.57834259461453996, -287.8117194252216109, -343.7560065552784181 ) ) ;
#33653 = CARTESIAN_POINT ( 'NONE',  ( 154.1415209985679269, 20.37991841447902175, 11.45812909362559040 ) ) ;
#33654 = CARTESIAN_POINT ( 'NONE',  ( -92.06913834561316889, -287.8330834980292821, -321.7196185466897873 ) ) ;
#33655 = CARTESIAN_POINT ( 'NONE',  ( -37.16796817485462157, -299.6545001417760545, -196.5581842902400069 ) ) ;
#33656 = CARTESIAN_POINT ( 'NONE',  ( 23.79466047301081844, -283.5921448908923139, -316.1972577293420841 ) ) ;
#33658 = CARTESIAN_POINT ( 'NONE',  ( -38.88507961700194215, -283.0720126773367724, -343.3572918297165302 ) ) ;
#33657 = CARTESIAN_POINT ( 'NONE',  ( -29.25402909278367503, -296.1730293061041266, -195.0086224598954061 ) ) ;
#33659 = CARTESIAN_POINT ( 'NONE',  ( 7.677174245882701697, -276.1059256043942582, -212.1487836749950588 ) ) ;
#33660 = CARTESIAN_POINT ( 'NONE',  ( 35.38546615758858849, -283.3169278407723368, -252.0373646458685073 ) ) ;
#33661 = CARTESIAN_POINT ( 'NONE',  ( -105.6995143030591322, -271.8265461743915239, -243.7365338049869763 ) ) ;
#33662 = ORIENTED_EDGE ( 'NONE', *, *, #91947, .T. ) ;
#33663 = CARTESIAN_POINT ( 'NONE',  ( 204.9607212768056002, 294.2270030158686609, -54.00000000002630429 ) ) ;
#33664 = CARTESIAN_POINT ( 'NONE',  ( 36.28760096717648764, -293.1025409726746602, -247.8283413065005334 ) ) ;
#33665 = CARTESIAN_POINT ( 'NONE',  ( -82.49308156484593724, -287.4118975820412061, -210.9203949553242126 ) ) ;
#33666 = CARTESIAN_POINT ( 'NONE',  ( 156.5191989162425727, 250.0000000000000568, 16.58062614384861178 ) ) ;
#33667 = CARTESIAN_POINT ( 'NONE',  ( -19.11405058567864046, -280.3380690714490129, -350.3683826091709648 ) ) ;
#33668 = CARTESIAN_POINT ( 'NONE',  ( -38.55268814232832852, -276.2641467717829755, -347.1900990328595071 ) ) ;
#33669 = CARTESIAN_POINT ( 'NONE',  ( -70.31157119121917276, -287.8792309234474942, -339.0735480313547896 ) ) ;
#33670 = CARTESIAN_POINT ( 'NONE',  ( -83.21129710071788566, -285.2133120241918505, -328.1040309522289817 ) ) ;
#33671 = CARTESIAN_POINT ( 'NONE',  ( -72.11066116754413713, -279.2786817679706246, -335.7137108542152646 ) ) ;
#33672 = VECTOR ( 'NONE', #49851, 1000.000000000000000 ) ;
#33673 = CARTESIAN_POINT ( 'NONE',  ( -111.7897729462377185, -286.1942796256317934, -253.1538303024127856 ) ) ;
#33674 = CARTESIAN_POINT ( 'NONE',  ( -37.55701601160195935, -281.8498643805666006, -343.7703736456794559 ) ) ;
#33675 = CARTESIAN_POINT ( 'NONE',  ( -69.40069153408602176, -281.6304327578977791, -202.5583029722567403 ) ) ;
#33676 = CARTESIAN_POINT ( 'NONE',  ( 24.47860339448041245, -275.1084676483693556, -224.4563243668394819 ) ) ;
#33677 = CARTESIAN_POINT ( 'NONE',  ( -56.92607864134298268, -277.1311549983469149, -344.8839635698042798 ) ) ;
#33678 = CARTESIAN_POINT ( 'NONE',  ( -4.892113991333567391, -296.5416556103949688, -337.3702674550272604 ) ) ;
#33679 = LINE ( 'NONE', #32753, #65681 ) ;
#33680 = ADVANCED_FACE ( 'NONE', ( #20372 ), #91103, .T. ) ;
#33681 = CARTESIAN_POINT ( 'NONE',  ( 185.4166944662902665, 214.7015631973135044, 22.87680765314684095 ) ) ;
#33682 = CARTESIAN_POINT ( 'NONE',  ( -111.3881803080732311, -294.8963911817058374, -254.2562071646758284 ) ) ;
#33683 = CARTESIAN_POINT ( 'NONE',  ( 32.92093513569110286, -274.7930572003534735, -250.1515436607077447 ) ) ;
#33684 = CARTESIAN_POINT ( 'NONE',  ( -62.75562827202377036, -298.8085967473858204, -198.0035007908743410 ) ) ;
#33685 = CARTESIAN_POINT ( 'NONE',  ( 15.74086640570477158, -288.5767274524653203, -218.7838444669939975 ) ) ;
#33686 = CARTESIAN_POINT ( 'NONE',  ( 6.234087937547879044, -295.9928573833530550, -333.0662213700896928 ) ) ;
#33687 = CARTESIAN_POINT ( 'NONE',  ( 0.3585246579834400760, -295.7666134188271485, -337.0598152207402336 ) ) ;
#33688 = CARTESIAN_POINT ( 'NONE',  ( -93.77798925993877788, -291.8680659363610630, -319.5809047017456237 ) ) ;
#33689 = CARTESIAN_POINT ( 'NONE',  ( -49.41317454312584800, -277.8977340672214495, -196.5078314649684899 ) ) ;
#33690 = CARTESIAN_POINT ( 'NONE',  ( -108.4857575370526064, -280.1857419737564783, -292.4387241674479014 ) ) ;
#33691 = CARTESIAN_POINT ( 'NONE',  ( -109.8747436432718700, -294.8485742719273048, -253.6197978293804454 ) ) ;
#33692 = CARTESIAN_POINT ( 'NONE',  ( -16.45917374120841004, -284.6456546521537234, -343.2456369855314051 ) ) ;
#33693 = CARTESIAN_POINT ( 'NONE',  ( 32.13792627948375014, -286.1631519168715840, -246.9772006941156519 ) ) ;
#33694 = CARTESIAN_POINT ( 'NONE',  ( -111.5752165548071986, -274.2545102287181180, -284.0995610720992772 ) ) ;
#33695 = VERTEX_POINT ( 'NONE', #72403 ) ;
#33696 = CARTESIAN_POINT ( 'NONE',  ( -108.6846531153470607, -284.4249090364280050, -254.7377143622873064 ) ) ;
#33697 = ORIENTED_EDGE ( 'NONE', *, *, #34577, .F. ) ;
#33698 = CARTESIAN_POINT ( 'NONE',  ( 34.30365023913424238, -282.9795592934676165, -297.7186814684547471 ) ) ;
#33700 = CARTESIAN_POINT ( 'NONE',  ( -92.03681255600260158, -273.5764303066907246, -221.9820712441353692 ) ) ;
#33699 = VECTOR ( 'NONE', #35523, 999.9999999999998863 ) ;
#33701 = CARTESIAN_POINT ( 'NONE',  ( -52.08176782460245846, -284.6625701657092122, -195.1356122146114842 ) ) ;
#33702 = CARTESIAN_POINT ( 'NONE',  ( -33.93773580570187676, -281.0352421516735717, -193.6719190019195196 ) ) ;
#33703 = DIRECTION ( 'NONE',  ( 1.000000000000000000, 0.000000000000000000, 0.000000000000000000 ) ) ;
#33704 = CARTESIAN_POINT ( 'NONE',  ( -39.58643605664883580, -281.5445938236794632, -194.0745400995285479 ) ) ;
#33705 = CARTESIAN_POINT ( 'NONE',  ( 17.14502302725733784, -281.4556240429934064, -216.0231233488367479 ) ) ;
#33706 = CARTESIAN_POINT ( 'NONE',  ( -105.5795714935544112, -288.2666405000203440, -254.7536222014695397 ) ) ;
#33707 = CARTESIAN_POINT ( 'NONE',  ( 26.31071593616584181, -23.39576146109087773, -345.1909842725040107 ) ) ;
#33708 = ORIENTED_EDGE ( 'NONE', *, *, #46281, .F. ) ;
#33709 = CARTESIAN_POINT ( 'NONE',  ( -18.84244262916453394, -276.2909034966050399, -197.7966492087222434 ) ) ;
#33710 = CARTESIAN_POINT ( 'NONE',  ( 64.17530680665127818, 48.17049669212057239, -318.6057662566004183 ) ) ;
#33711 = CIRCLE ( 'NONE', #20063, 4.025000000000000355 ) ;
#33712 = CARTESIAN_POINT ( 'NONE',  ( -32.83916367470790476, -278.1292794572481171, -195.8522328115398921 ) ) ;
#33713 = CARTESIAN_POINT ( 'NONE',  ( 10.46364476597024584, -294.4615808310846319, -211.2288719802450032 ) ) ;
#33714 = CARTESIAN_POINT ( 'NONE',  ( -108.6931708251894690, -295.6912616085022592, -286.2626996000261670 ) ) ;
#33715 = CARTESIAN_POINT ( 'NONE',  ( -36.37284023812897260, -291.5716499810744153, -193.4157345928995255 ) ) ;
#33716 = CARTESIAN_POINT ( 'NONE',  ( 196.7510731661265595, -143.7221692137691775, -21.50000000000000000 ) ) ;
#33717 = AXIS2_PLACEMENT_3D ( 'NONE', #50600, #5652, #20325 ) ;
#33719 = CARTESIAN_POINT ( 'NONE',  ( 24.21246393252809170, -285.3922174050144918, -229.5558423132454493 ) ) ;
#33718 = CARTESIAN_POINT ( 'NONE',  ( -105.4408738666261058, -294.6758408404045895, -305.1347442407738413 ) ) ;
#33720 = CARTESIAN_POINT ( 'NONE',  ( 32.71345683582602959, -295.7356792130172494, -295.0740974668204899 ) ) ;
#33721 = CARTESIAN_POINT ( 'NONE',  ( -87.25153948568416240, -285.0801928818528950, -324.3774728692913527 ) ) ;
#33722 = ORIENTED_EDGE ( 'NONE', *, *, #79144, .F. ) ;
#33723 = CARTESIAN_POINT ( 'NONE',  ( -108.1547181753909257, -291.8715086279845536, -240.7243724226984511 ) ) ;
#33724 = CIRCLE ( 'NONE', #54864, 4.500000000000003553 ) ;
#33725 = CARTESIAN_POINT ( 'NONE',  ( 11.96283158980991068, -282.8366508234660159, -324.2781987046529935 ) ) ;
#33726 = CARTESIAN_POINT ( 'NONE',  ( -95.29122354764726310, -294.6668258874401545, -320.4596354743204074 ) ) ;
#33727 = CARTESIAN_POINT ( 'NONE',  ( -111.0800873768386339, -291.6265468158190970, -248.7553533214974379 ) ) ;
#33728 = CARTESIAN_POINT ( 'NONE',  ( -58.92743026163221742, -292.2724904976134894, -196.5127384628947027 ) ) ;
#33729 = CARTESIAN_POINT ( 'NONE',  ( 35.68030624157331943, -287.6917801846342968, -268.3103421497913814 ) ) ;
#33730 = ORIENTED_EDGE ( 'NONE', *, *, #23779, .F. ) ;
#33731 = DIRECTION ( 'NONE',  ( -0.000000000000000000, -0.000000000000000000, 1.000000000000000000 ) ) ;
#33732 = CARTESIAN_POINT ( 'NONE',  ( -66.42798308569273047, -297.2893707665758711, -340.3343179143163866 ) ) ;
#33733 = CIRCLE ( 'NONE', #9511, 8.000000000000000000 ) ;
#33734 = CARTESIAN_POINT ( 'NONE',  ( -23.45422380015054742, -296.9074280743311078, -193.8572936979943790 ) ) ;
#33735 = CARTESIAN_POINT ( 'NONE',  ( -69.83392783122764058, -278.6721572194342684, -204.7144357722766017 ) ) ;
#33736 = CARTESIAN_POINT ( 'NONE',  ( 24.43420870566513869, -274.4495469477350866, -224.4997617970815043 ) ) ;
#33737 = CARTESIAN_POINT ( 'NONE',  ( -106.4493367498670295, -295.3717816249535417, -244.6241461178034058 ) ) ;
#33738 = CARTESIAN_POINT ( 'NONE',  ( -24.08615795874431598, -278.7416405388045746, -343.4555944186350871 ) ) ;
#33739 = CARTESIAN_POINT ( 'NONE',  ( 18.22563593566900764, -272.9994053363270154, -221.0595528862527885 ) ) ;
#33740 = CARTESIAN_POINT ( 'NONE',  ( -95.91196825982326857, -297.1389466710945158, -314.6159008857245567 ) ) ;
#33741 = CARTESIAN_POINT ( 'NONE',  ( -52.71326549373046788, -298.9303599095174491, -198.6295784983753379 ) ) ;
#33742 = CARTESIAN_POINT ( 'NONE',  ( 199.0061125298537377, 275.5000000000000568, -12.72542485937401580 ) ) ;
#33743 = CARTESIAN_POINT ( 'NONE',  ( -11.31113936669362374, -296.3188266206519756, -342.0330977658765050 ) ) ;
#33744 = AXIS2_PLACEMENT_3D ( 'NONE', #23625, #51553, #45368 ) ;
#33745 = CARTESIAN_POINT ( 'NONE',  ( -108.5393859029297943, -270.8902628781388557, -245.6771891607730822 ) ) ;
#33746 = CARTESIAN_POINT ( 'NONE',  ( -81.79760104361372441, -292.0800045337432493, -212.2663282159022344 ) ) ;
#33747 = CARTESIAN_POINT ( 'NONE',  ( -101.6296669525037117, -289.6138784773024781, -234.4454371296471606 ) ) ;
#33748 = DIRECTION ( 'NONE',  ( -0.000000000000000000, 1.000000000000000000, -0.000000000000000000 ) ) ;
#33749 = CARTESIAN_POINT ( 'NONE',  ( 36.43623797249316709, -276.3190514822618979, -292.2328912709730844 ) ) ;
#33750 = CARTESIAN_POINT ( 'NONE',  ( -90.06407026925775483, -297.6149837066819828, -219.7670809749123748 ) ) ;
#33751 = CARTESIAN_POINT ( 'NONE',  ( -34.01369287405827180, -282.0737145102760337, -195.0794391186080361 ) ) ;
#33752 = CARTESIAN_POINT ( 'NONE',  ( 38.17834042626236624, -280.3921806532635514, -282.6911801347736741 ) ) ;
#33753 = AXIS2_PLACEMENT_3D ( 'NONE', #35074, #57802, #78642 ) ;
#33754 = CARTESIAN_POINT ( 'NONE',  ( 5.807221992082605588, -275.8324040408410269, -334.0123811767265920 ) ) ;
#33755 = CARTESIAN_POINT ( 'NONE',  ( -2.360428848575252925, -281.7739240110116725, -334.6320515182482609 ) ) ;
#33756 = CARTESIAN_POINT ( 'NONE',  ( 36.19650027554965988, -279.3518397082912088, -254.7379053054851852 ) ) ;
#33757 = EDGE_CURVE ( 'NONE', #30930, #42782, #21638, .T. ) ;
#33758 = CARTESIAN_POINT ( 'NONE',  ( -8.725072674853340260, -273.0086725489012451, -202.5095404288539100 ) ) ;
#33759 = CARTESIAN_POINT ( 'NONE',  ( -74.71650625273734647, -279.5493441005215232, -335.4433520056854832 ) ) ;
#33760 = DIRECTION ( 'NONE',  ( -1.000000000000000000, 0.000000000000000000, 0.000000000000000000 ) ) ;
#33761 = FACE_BOUND ( 'NONE', #28526, .T. ) ;
#33762 = CARTESIAN_POINT ( 'NONE',  ( -30.57415178395767796, -296.3756381714261465, -194.3764399578238624 ) ) ;
#33763 = CARTESIAN_POINT ( 'NONE',  ( 34.74273139890103579, -277.8266213288238191, -291.7106475035720905 ) ) ;
#33764 = CARTESIAN_POINT ( 'NONE',  ( -75.26321996967618588, -271.5469468724480748, -205.5942532011225694 ) ) ;
#33765 = LINE ( 'NONE', #40831, #25663 ) ;
#33766 = CARTESIAN_POINT ( 'NONE',  ( -112.7691468501050451, -286.4050046173633746, -275.6419655058780904 ) ) ;
#33767 = ORIENTED_EDGE ( 'NONE', *, *, #48884, .F. ) ;
#33768 = CARTESIAN_POINT ( 'NONE',  ( 207.6573036349384438, 36.26995571305734956, 14.90818566952114921 ) ) ;
#33769 = CARTESIAN_POINT ( 'NONE',  ( -24.34095841460435850, -286.8861492431840361, -344.2776954139054055 ) ) ;
#33770 = CARTESIAN_POINT ( 'NONE',  ( 207.0345761854011073, 29.47290414794718671, 13.79342392267523643 ) ) ;
#33771 = CARTESIAN_POINT ( 'NONE',  ( 34.15876571452299260, -292.5652325961062274, -286.9939472881684992 ) ) ;
#33772 = CARTESIAN_POINT ( 'NONE',  ( 31.10977764642794696, -285.3111224219507562, -241.5005440180586049 ) ) ;
#33773 = CARTESIAN_POINT ( 'NONE',  ( -71.74250447947856912, -195.9422791308210492, -360.7315132586310824 ) ) ;
#33774 = CARTESIAN_POINT ( 'NONE',  ( -100.1077446438986129, -295.1069028352944770, -229.2132633096373411 ) ) ;
#33775 = CARTESIAN_POINT ( 'NONE',  ( -54.78712749521336889, -284.3117141781163468, -196.0754207396757636 ) ) ;
#33776 = CARTESIAN_POINT ( 'NONE',  ( -86.02705451083080845, -280.9639830613383538, -214.8978266819527789 ) ) ;
#33777 = CARTESIAN_POINT ( 'NONE',  ( 36.40632889669196715, -289.0187437901540193, -291.1272920222765492 ) ) ;
#33778 = CARTESIAN_POINT ( 'NONE',  ( 19.01666979615950481, -280.4940768126017474, -321.4057884394308076 ) ) ;
#33779 = CARTESIAN_POINT ( 'NONE',  ( -95.76832199553885516, -289.9375932327725991, -314.1464605852987688 ) ) ;
#33780 = CIRCLE ( 'NONE', #35267, 0.4999999999999977796 ) ;
#33781 = CARTESIAN_POINT ( 'NONE',  ( -49.25503182952828496, -281.3226153242526948, -197.7426117766690368 ) ) ;
#33782 = CARTESIAN_POINT ( 'NONE',  ( 27.92082260691312356, -281.9056627253713145, -237.1821436241081926 ) ) ;
#33783 = CARTESIAN_POINT ( 'NONE',  ( 18.42437677322572398, -290.2359783716213428, -321.0612241675873975 ) ) ;
#33784 = ORIENTED_EDGE ( 'NONE', *, *, #72569, .T. ) ;
#33785 = CIRCLE ( 'NONE', #88166, 239.0731808058633590 ) ;
#33786 = CARTESIAN_POINT ( 'NONE',  ( -83.58009169530156157, -273.4378093803254046, -208.7231973228109041 ) ) ;
#33787 = CARTESIAN_POINT ( 'NONE',  ( -87.82360478376411095, -291.7412389053965853, -325.4168866121209476 ) ) ;
#33788 = CARTESIAN_POINT ( 'NONE',  ( -110.4683760289727132, -275.2662352645559167, -253.7030783399848985 ) ) ;
#33789 = ORIENTED_EDGE ( 'NONE', *, *, #53476, .T. ) ;
#33790 = CARTESIAN_POINT ( 'NONE',  ( 14.77468822335568355, -272.7842003558055808, -216.1955339830585672 ) ) ;
#33791 = CARTESIAN_POINT ( 'NONE',  ( 128.9467878515196162, -299.5541904835127980, -195.3611179825600175 ) ) ;
#33792 = CARTESIAN_POINT ( 'NONE',  ( -90.17226282765506085, -294.1836238426474210, -325.3461868356761784 ) ) ;
#33793 = CARTESIAN_POINT ( 'NONE',  ( -103.7719314678626858, -296.4710905878346807, -239.8253461820677899 ) ) ;
#33794 = AXIS2_PLACEMENT_3D ( 'NONE', #70362, #21079, #36216 ) ;
#33795 = CARTESIAN_POINT ( 'NONE',  ( 27.65099010683070802, -289.5426114480258093, -305.2067608044213216 ) ) ;
#33796 = PRODUCT_DEFINITION_SHAPE ( 'NONE', 'NONE',  #91591 ) ;
#33797 = CARTESIAN_POINT ( 'NONE',  ( -3.133372182716995802, -284.3540076357942894, -336.0088801727681016 ) ) ;
#33798 = CARTESIAN_POINT ( 'NONE',  ( -71.62570266975140498, -290.9214989012764931, -338.6488435612252488 ) ) ;
#33799 = CARTESIAN_POINT ( 'NONE',  ( -45.95351796857004700, -290.4742168356576713, -346.4345253226774730 ) ) ;
#33800 = CARTESIAN_POINT ( 'NONE',  ( -78.15830154116531503, -287.5039227347750739, -207.3788564912533445 ) ) ;
#33801 = CARTESIAN_POINT ( 'NONE',  ( -25.39768465061203528, -280.3670567146467079, -194.2931188057497991 ) ) ;
#33802 = CARTESIAN_POINT ( 'NONE',  ( -106.4459739295153042, -295.0308322974671569, -239.6718511773943590 ) ) ;
#33803 = CARTESIAN_POINT ( 'NONE',  ( -76.75971970600521388, -283.3974967842848400, -336.5683819617340191 ) ) ;
#33804 = CIRCLE ( 'NONE', #14157, 24.00000000000000355 ) ;
#33805 = CARTESIAN_POINT ( 'NONE',  ( 29.14719111883521663, -277.8541568506474846, -303.4936299544430653 ) ) ;
#33806 = CARTESIAN_POINT ( 'NONE',  ( -53.35057174420112602, -276.3376638359844719, -200.3683826091709648 ) ) ;
#33807 = CARTESIAN_POINT ( 'NONE',  ( 20.93880890519416127, -274.4569667345166977, -319.1192586699451113 ) ) ;
#33808 = CARTESIAN_POINT ( 'NONE',  ( -39.80257052418234309, -229.5268262511776527, -22.50000000000000000 ) ) ;
#33809 = CARTESIAN_POINT ( 'NONE',  ( 20.56854496768234242, -280.4331769290819807, -225.7942674910315191 ) ) ;
#33810 = CIRCLE ( 'NONE', #45889, 4.999999999999985789 ) ;
#33811 = CARTESIAN_POINT ( 'NONE',  ( -96.73673250947265956, -279.1044642454227755, -318.7576695002701399 ) ) ;
#33812 = CARTESIAN_POINT ( 'NONE',  ( -83.12590738706026627, -284.5014538099298989, -208.6780673984494854 ) ) ;
#33813 = CARTESIAN_POINT ( 'NONE',  ( -28.00036783105862881, -293.9323577414428428, -196.8881875353038424 ) ) ;
#33814 = CARTESIAN_POINT ( 'NONE',  ( 29.84739320970582099, -277.6229826417745699, -306.4179061020159338 ) ) ;
#33815 = EDGE_CURVE ( 'NONE', #33225, #89964, #62021, .T. ) ;
#33816 = CARTESIAN_POINT ( 'NONE',  ( -85.51080777927758447, -274.7169116835381715, -210.9217763012428009 ) ) ;
#33817 = CARTESIAN_POINT ( 'NONE',  ( 158.3135449435333442, 1.828427124746190957, 9.000000000000000000 ) ) ;
#33819 = EDGE_CURVE ( 'NONE', #19834, #64501, #51071, .T. ) ;
#33818 = CARTESIAN_POINT ( 'NONE',  ( 32.09752579143857787, -275.6842649635597695, -292.8820839521200696 ) ) ;
#33820 = CARTESIAN_POINT ( 'NONE',  ( -78.94842737287626733, -297.6142186612916021, -332.6242456462766768 ) ) ;
#33821 = CARTESIAN_POINT ( 'NONE',  ( -111.8163763972752065, -282.6527165834509674, -262.5335868042495804 ) ) ;
#33822 = CARTESIAN_POINT ( 'NONE',  ( 30.88215281240306354, -292.7574512093871135, -234.5917578125729506 ) ) ;
#33823 = CARTESIAN_POINT ( 'NONE',  ( 29.34171850520809244, -273.1270556240142469, -236.8175868777147173 ) ) ;
#33824 = CARTESIAN_POINT ( 'NONE',  ( 37.88852784372399185, -289.3094845643806821, -282.8007369110895866 ) ) ;
#33825 = AXIS2_PLACEMENT_3D ( 'NONE', #85617, #87007, #43007 ) ;
#33826 = CARTESIAN_POINT ( 'NONE',  ( -33.47845432455119408, -291.0222134339394415, -197.1413233305401320 ) ) ;
#33827 = VERTEX_POINT ( 'NONE', #79957 ) ;
#33828 = CARTESIAN_POINT ( 'NONE',  ( -39.17918921479973449, -290.6042829835803900, -193.9595055652978886 ) ) ;
#33829 = CARTESIAN_POINT ( 'NONE',  ( -110.3888421438364418, -290.2439803127227833, -268.4569745040915336 ) ) ;
#33830 = ORIENTED_EDGE ( 'NONE', *, *, #68796, .F. ) ;
#33831 = CARTESIAN_POINT ( 'NONE',  ( 18.11841531099407021, -287.9038540202856211, -217.3159879620078243 ) ) ;
#33832 = CARTESIAN_POINT ( 'NONE',  ( -96.42530883021679244, -279.4857723892326931, -227.4517405743245604 ) ) ;
#33833 = CARTESIAN_POINT ( 'NONE',  ( -74.46881810041973893, -294.4539975366014914, -337.5255108577839565 ) ) ;
#33834 = CARTESIAN_POINT ( 'NONE',  ( -110.8310821718662140, -285.4903081944621022, -247.5406397032579662 ) ) ;
#33835 = CARTESIAN_POINT ( 'NONE',  ( 30.11098635295186909, -287.4036630030869901, -233.1576786375955805 ) ) ;
#33836 = CARTESIAN_POINT ( 'NONE',  ( 21.83156336641219397, -282.4840437742049630, -313.1681846620591045 ) ) ;
#33837 = CARTESIAN_POINT ( 'NONE',  ( 180.0122957173031182, 254.2448111356339666, -166.7447581597871817 ) ) ;
#33838 = CARTESIAN_POINT ( 'NONE',  ( -72.14048337055831439, -195.4227484145153824, -359.3792095499467791 ) ) ;
#33839 = CARTESIAN_POINT ( 'NONE',  ( -77.70721554921161101, -207.5803895343633201, -353.5487745245097244 ) ) ;
#33840 = CARTESIAN_POINT ( 'NONE',  ( 35.80455650795468614, -274.7296725181265060, -268.8688490505106188 ) ) ;
#33841 = CARTESIAN_POINT ( 'NONE',  ( 27.03163580294197388, -274.9505304558853709, -305.5428311301544682 ) ) ;
#33842 = CARTESIAN_POINT ( 'NONE',  ( -54.57528130596574556, -297.3440671449835691, -195.3775825708489435 ) ) ;
#33843 = CARTESIAN_POINT ( 'NONE',  ( -81.64875865379578102, -219.6352840722641702, -349.5921457167885933 ) ) ;
#33844 = CARTESIAN_POINT ( 'NONE',  ( 37.10807293655612682, -274.4594436001175950, -288.0393427025508686 ) ) ;
#33845 = CARTESIAN_POINT ( 'NONE',  ( -77.12757094218183340, -275.2710118047654078, -207.9507142341998644 ) ) ;
#33846 = ORIENTED_EDGE ( 'NONE', *, *, #73031, .T. ) ;
#33847 = CARTESIAN_POINT ( 'NONE',  ( -70.63785974892620345, -298.5649740426521248, -201.1933077759243531 ) ) ;
#33848 = CARTESIAN_POINT ( 'NONE',  ( 8.023052373463098519, -288.9048169349887303, -327.6326438215676262 ) ) ;
#33849 = CARTESIAN_POINT ( 'NONE',  ( -111.0575757302146229, -297.0819044642089466, -292.0899524289468445 ) ) ;
#33850 = CARTESIAN_POINT ( 'NONE',  ( -37.61374168157973941, -298.5411755449079578, -193.4231371344880586 ) ) ;
#33851 = CARTESIAN_POINT ( 'NONE',  ( -9.729445409839209802, -292.5897147347177452, -202.7309814949156817 ) ) ;
#33852 = EDGE_LOOP ( 'NONE', ( #55744, #55923, #54648, #81093 ) ) ;
#33853 = CARTESIAN_POINT ( 'NONE',  ( 22.39492144971670129, -278.1020784981679981, -316.6514331525444845 ) ) ;
#33854 = ORIENTED_EDGE ( 'NONE', *, *, #37113, .F. ) ;
#33855 = CARTESIAN_POINT ( 'NONE',  ( -11.52409435987599196, -279.8871164546936825, -197.8277467623605048 ) ) ;
#33856 = ADVANCED_FACE ( 'NONE', ( #1812 ), #7521, .T. ) ;
#33857 = CARTESIAN_POINT ( 'NONE',  ( -69.34344469044526704, -278.4250853560899372, -336.2483377748475846 ) ) ;
#33858 = CARTESIAN_POINT ( 'NONE',  ( 12.06299619457478123, -278.1361065815718234, -328.0945571029552070 ) ) ;
#33859 = CARTESIAN_POINT ( 'NONE',  ( -48.28068231435913304, -275.2106661057962356, -344.9708581079594296 ) ) ;
#33860 = CARTESIAN_POINT ( 'NONE',  ( -108.5782377095010958, -297.4197250956665926, -253.9523282039501453 ) ) ;
#33861 = CARTESIAN_POINT ( 'NONE',  ( -108.8760524274291299, -294.9002027674437727, -287.6831073336275040 ) ) ;
#33862 = CARTESIAN_POINT ( 'NONE',  ( 37.92315709790361211, -281.8439440636951190, -254.3379082531501183 ) ) ;
#33863 = CARTESIAN_POINT ( 'NONE',  ( -108.2901696014262853, -278.9455652831478005, -253.1763955837307947 ) ) ;
#33864 = TOROIDAL_SURFACE ( 'NONE', #35427, 5.654241149514405151, 0.5000000000000000000 ) ;
#33865 = CARTESIAN_POINT ( 'NONE',  ( -17.86612635525965942, -287.4909276363273420, -344.3476052467601107 ) ) ;
#33866 = CARTESIAN_POINT ( 'NONE',  ( -37.62689429295477339, -300.0487446805060472, -195.1949880053350057 ) ) ;
#33867 = AXIS2_PLACEMENT_3D ( 'NONE', #18392, #68596, #82782 ) ;
#33868 = CARTESIAN_POINT ( 'NONE',  ( -45.39034395246071796, -288.3539005628863947, -343.0785234603453091 ) ) ;
#33869 = CONICAL_SURFACE ( 'NONE', #53537, 1.898405138727909947, 0.09862129276975308001 ) ;
#33870 = CARTESIAN_POINT ( 'NONE',  ( -75.00236733635060205, -277.7834008169206186, -206.5868505137839293 ) ) ;
#33872 = CARTESIAN_POINT ( 'NONE',  ( -7.947696855606018573, -280.7438624002766687, -338.7519563420138979 ) ) ;
#33871 = CARTESIAN_POINT ( 'NONE',  ( -94.38587109222731897, -277.7797112846501477, -223.8709310826332342 ) ) ;
#33873 = CARTESIAN_POINT ( 'NONE',  ( -109.0890889154887446, -286.8359154820719255, -248.3409727001177885 ) ) ;
#33874 = CARTESIAN_POINT ( 'NONE',  ( -83.70035267687553926, -280.6048669847451720, -213.3918459106722310 ) ) ;
#33875 = CARTESIAN_POINT ( 'NONE',  ( 153.9133111279453203, 20.47222690886559704, 13.06183683676577267 ) ) ;
#33876 = CARTESIAN_POINT ( 'NONE',  ( -30.89523986952798751, -294.1336568520080732, -195.5872849274080068 ) ) ;
#33878 = CARTESIAN_POINT ( 'NONE',  ( -64.75075767896055368, -275.6449333277507776, -341.2878047447979384 ) ) ;
#33877 = AXIS2_PLACEMENT_3D ( 'NONE', #69263, #4392, #85790 ) ;
#33879 = CARTESIAN_POINT ( 'NONE',  ( 11.82238302878409009, -276.9992650508387442, -324.5295881254055530 ) ) ;
#33880 = CARTESIAN_POINT ( 'NONE',  ( 20.54221720100352400, -282.8919155636764344, -222.4082187477000900 ) ) ;
#33881 = CARTESIAN_POINT ( 'NONE',  ( -112.5755490930345957, -292.5685981335822703, -262.8057246419418789 ) ) ;
#33882 = CARTESIAN_POINT ( 'NONE',  ( -42.34388622391904988, -293.1150494231443417, -345.2067988781342365 ) ) ;
#33883 = AXIS2_PLACEMENT_3D ( 'NONE', #2482, #60247, #10027 ) ;
#33884 = CARTESIAN_POINT ( 'NONE',  ( -69.71547127027052682, -284.8338905530135321, -200.6610764017653707 ) ) ;
#33885 = CARTESIAN_POINT ( 'NONE',  ( 194.5881128153457098, -26.00396092263537540, 21.50000000000000000 ) ) ;
#33886 = CARTESIAN_POINT ( 'NONE',  ( -67.24291316677461339, -272.3365010762616976, -203.2119416307060931 ) ) ;
#33887 = CARTESIAN_POINT ( 'NONE',  ( 29.86671287470853642, -291.2715533670002515, -238.7136208295203801 ) ) ;
#33888 = LINE ( 'NONE', #4073, #50281 ) ;
#33889 = CARTESIAN_POINT ( 'NONE',  ( 202.9738562182569694, 293.9636489450776367, -54.00000000000000000 ) ) ;
#33890 = CARTESIAN_POINT ( 'NONE',  ( -56.00034568096261012, -290.2961104416397689, -196.3163807350143202 ) ) ;
#33891 = CARTESIAN_POINT ( 'NONE',  ( -95.60101743429282806, -286.7838469390944169, -225.0383577617677417 ) ) ;
#33892 = CARTESIAN_POINT ( 'NONE',  ( 1.029587048623485046, -284.7967053985813664, -204.7592553813738903 ) ) ;
#33893 = CARTESIAN_POINT ( 'NONE',  ( -103.5348021783674142, -285.5442206411549364, -302.6315960910006311 ) ) ;
#33894 = LINE ( 'NONE', #18754, #24526 ) ;
#33895 = CARTESIAN_POINT ( 'NONE',  ( -44.04933666083234556, -286.7680101382247813, -197.5077766789300995 ) ) ;
#33896 = CARTESIAN_POINT ( 'NONE',  ( -6.581915198994430227, -294.4339016418616097, -201.5558411673713124 ) ) ;
#33897 = CARTESIAN_POINT ( 'NONE',  ( 37.94362464737805851, -273.7140342564095477, -276.7980481195375546 ) ) ;
#33898 = CARTESIAN_POINT ( 'NONE',  ( 38.90264903534559693, -275.7527198823302115, -259.7524652803982690 ) ) ;
#33899 = CARTESIAN_POINT ( 'NONE',  ( -72.73710301352454621, -289.6670365382692012, -203.5896292693017244 ) ) ;
#33900 = CARTESIAN_POINT ( 'NONE',  ( -112.9961795060496001, -278.7322726721104686, -255.9588285635283000 ) ) ;
#33901 = CARTESIAN_POINT ( 'NONE',  ( -41.09731186905212041, -297.0795161791457986, -344.9242347159923270 ) ) ;
#33902 = CARTESIAN_POINT ( 'NONE',  ( -48.18343439339133027, -255.7030234860429516, -485.0668374018911777 ) ) ;
#33903 = CARTESIAN_POINT ( 'NONE',  ( 152.4536156746142410, 276.0000000000000568, 12.00000000000000000 ) ) ;
#33904 = CARTESIAN_POINT ( 'NONE',  ( -42.69343914706002607, -284.6680750775250885, -197.0503691397170201 ) ) ;
#33905 = CARTESIAN_POINT ( 'NONE',  ( 15.82382390753229373, -278.8044777029996908, -217.3881010388162451 ) ) ;
#33906 = DIRECTION ( 'NONE',  ( -0.000000000000000000, -1.000000000000000000, -0.000000000000000000 ) ) ;
#33907 = CARTESIAN_POINT ( 'NONE',  ( -10.57254070365111431, -272.8748510113835550, -198.8477803118141765 ) ) ;
#33908 = CARTESIAN_POINT ( 'NONE',  ( -78.69649164067767799, -276.9739068929330301, -330.7027239114034955 ) ) ;
#33909 = CARTESIAN_POINT ( 'NONE',  ( 23.51640978366198453, -295.6461198629912133, -312.0075538529216601 ) ) ;
#33910 = CARTESIAN_POINT ( 'NONE',  ( -7.643943147984653130, -279.3527226730674329, -199.6394757744152173 ) ) ;
#33911 = CARTESIAN_POINT ( 'NONE',  ( -42.39403018035636705, -296.0586874008787390, -343.4219310725983405 ) ) ;
#33912 = CARTESIAN_POINT ( 'NONE',  ( -4.697651776471670537, -295.9462863609767282, -339.5684473380565009 ) ) ;
#33913 = CARTESIAN_POINT ( 'NONE',  ( -44.56697264216801813, -297.7916432804731812, -197.6691815334732212 ) ) ;
#33914 = CARTESIAN_POINT ( 'NONE',  ( -52.80637680195250994, -293.8542785132333961, -196.9194786388742671 ) ) ;
#33915 = CARTESIAN_POINT ( 'NONE',  ( -99.34550382253182477, -285.3263917739964199, -224.6167497834574931 ) ) ;
#33916 = CARTESIAN_POINT ( 'NONE',  ( 36.09394618947436584, -273.4546752615383411, -251.7194621177667386 ) ) ;
#33917 = CARTESIAN_POINT ( 'NONE',  ( -37.50372076829603429, -288.8874127097809037, -347.3740193428915290 ) ) ;
#33918 = CARTESIAN_POINT ( 'NONE',  ( -112.0377693549130385, -280.5280725484354321, -270.6694575696985794 ) ) ;
#33919 = CARTESIAN_POINT ( 'NONE',  ( 32.53451506376017477, -286.9025561681858107, -292.4552068991233114 ) ) ;
#33920 = CARTESIAN_POINT ( 'NONE',  ( -40.52145238496140678, -290.0120326608300161, -195.4157094716535710 ) ) ;
#33921 = CARTESIAN_POINT ( 'NONE',  ( -72.76141013609318975, -193.8959084914727669, -354.0272458012134393 ) ) ;
#33922 = CIRCLE ( 'NONE', #45995, 4.000000000000003553 ) ;
#33923 = CARTESIAN_POINT ( 'NONE',  ( 17.82677097956141310, -286.3775288375660466, -222.4609276129978070 ) ) ;
#33924 = CARTESIAN_POINT ( 'NONE',  ( 204.4182217051425141, 300.0864416745848757, -5.149757974892338552 ) ) ;
#33925 = CARTESIAN_POINT ( 'NONE',  ( 36.96706595943278018, -282.7352201434646304, -289.6231920196497072 ) ) ;
#33926 = CARTESIAN_POINT ( 'NONE',  ( -114.1548182960137154, -289.6002006125409025, -271.2141424905611302 ) ) ;
#33927 = CARTESIAN_POINT ( 'NONE',  ( 34.56590657953351098, -282.8291154953886348, -244.9898298213585122 ) ) ;
#33928 = EDGE_CURVE ( 'NONE', #47026, #65957, #21855, .T. ) ;
#33929 = CARTESIAN_POINT ( 'NONE',  ( -5.166719963894286671, -281.7820234821972463, -200.9488069267982269 ) ) ;
#33930 = CARTESIAN_POINT ( 'NONE',  ( 33.32297546006198274, -281.6278747319022386, -288.7276615407365625 ) ) ;
#33931 = CARTESIAN_POINT ( 'NONE',  ( 4.012042091634596019, -276.6089133121712962, -207.7301516251787632 ) ) ;
#33932 = CARTESIAN_POINT ( 'NONE',  ( -58.85132075442897559, -295.3227910122868138, -344.3513654065019978 ) ) ;
#33933 = CIRCLE ( 'NONE', #29408, 4.000000000000003553 ) ;
#33934 = CARTESIAN_POINT ( 'NONE',  ( -99.65911228022191892, -289.1307003409116874, -229.1772899730015638 ) ) ;
#33935 = CARTESIAN_POINT ( 'NONE',  ( -49.99381059216882051, -296.8072274659227219, -198.1520453282938377 ) ) ;
#33936 = ORIENTED_EDGE ( 'NONE', *, *, #8605, .T. ) ;
#33937 = ORIENTED_EDGE ( 'NONE', *, *, #70497, .T. ) ;
#33938 = CARTESIAN_POINT ( 'NONE',  ( -104.8005769654177470, -286.8905090258740529, -238.7648156088026496 ) ) ;
#33939 = AXIS2_PLACEMENT_3D ( 'NONE', #353, #15028, #43887 ) ;
#33940 = CARTESIAN_POINT ( 'NONE',  ( -6.025790800353265197, -293.5338264351685780, -200.3411290667411890 ) ) ;
#33941 = AXIS2_PLACEMENT_3D ( 'NONE', #41741, #34196, #70654 ) ;
#33942 = CARTESIAN_POINT ( 'NONE',  ( 21.09638085842285449, -282.8196341261192970, -314.3008608180597321 ) ) ;
#33943 = CARTESIAN_POINT ( 'NONE',  ( 22.58222267754217683, -273.9660599147180164, -222.3616934020354563 ) ) ;
#33944 = CARTESIAN_POINT ( 'NONE',  ( -56.17186648268803850, -292.4672961695368372, -195.7492988734259143 ) ) ;
#33945 = CARTESIAN_POINT ( 'NONE',  ( -112.6782060976187125, -282.5894872960722068, -278.4057651175401702 ) ) ;
#33946 = CARTESIAN_POINT ( 'NONE',  ( -36.38289612213738877, -292.3971445684914556, -193.3752045111904465 ) ) ;
#33947 = CARTESIAN_POINT ( 'NONE',  ( 35.67636106844881994, -287.8942844350714836, -271.0321066393260594 ) ) ;
#33948 = CARTESIAN_POINT ( 'NONE',  ( 194.2870706637141325, 27.48493576247232184, 14.58823529411763431 ) ) ;
#33949 = AXIS2_PLACEMENT_3D ( 'NONE', #15558, #59599, #88449 ) ;
#33950 = DIRECTION ( 'NONE',  ( 2.312964634635742267E-15, 0.000000000000000000, 1.000000000000000000 ) ) ;
#33951 = CARTESIAN_POINT ( 'NONE',  ( -30.58931055946544930, -124.9542506483939661, -360.4434141177968058 ) ) ;
#33952 = CARTESIAN_POINT ( 'NONE',  ( -68.88204076869831738, -284.9794498174313730, -339.8585973204147876 ) ) ;
#33953 = CARTESIAN_POINT ( 'NONE',  ( -37.37352853689063181, -286.5523547857347353, -345.3611179825600175 ) ) ;
#33954 = ORIENTED_EDGE ( 'NONE', *, *, #4023, .T. ) ;
#33955 = CARTESIAN_POINT ( 'NONE',  ( 33.75873697741572244, -280.2371728747124280, -252.4507961944683530 ) ) ;
#33956 = CARTESIAN_POINT ( 'NONE',  ( -17.36747659711747716, -276.4679232909452935, -344.7033985890554391 ) ) ;
#33957 = CARTESIAN_POINT ( 'NONE',  ( -110.9396822562341072, -280.7265676173724955, -256.8198678388772578 ) ) ;
#33958 = CARTESIAN_POINT ( 'NONE',  ( -28.99645464915736426, -125.7048492729908844, -362.1742968396590641 ) ) ;
#33959 = CARTESIAN_POINT ( 'NONE',  ( 38.93968215176566616, -280.1933904221051534, -275.6384269944435914 ) ) ;
#33960 = CARTESIAN_POINT ( 'NONE',  ( -111.8687854989046713, -282.6371639646095559, -265.3297698834770699 ) ) ;
#33961 = CARTESIAN_POINT ( 'NONE',  ( 74.50552286126109891, -301.1943555422959093, -194.3414303693253942 ) ) ;
#33962 = CARTESIAN_POINT ( 'NONE',  ( 27.21538126783730505, -294.5114283558988859, -304.6799393237983509 ) ) ;
#33963 = ORIENTED_EDGE ( 'NONE', *, *, #8701, .F. ) ;
#33964 = CARTESIAN_POINT ( 'NONE',  ( -88.26027104274552926, -290.0060137901919575, -217.2951193044740421 ) ) ;
#33965 = CARTESIAN_POINT ( 'NONE',  ( 36.39808021849354702, -276.4780918186856411, -292.2194611461752629 ) ) ;
#33966 = CARTESIAN_POINT ( 'NONE',  ( 34.62565556512682008, -275.3897703403181367, -258.0516880542799640 ) ) ;
#33967 = CARTESIAN_POINT ( 'NONE',  ( -105.3285225304123429, -271.9334142874049007, -234.7599817635760076 ) ) ;
#33968 = CARTESIAN_POINT ( 'NONE',  ( 198.8231951154315880, 63.33276796857077784, 10.00000000000000000 ) ) ;
#33969 = FACE_OUTER_BOUND ( 'NONE', #72818, .T. ) ;
#33970 = CARTESIAN_POINT ( 'NONE',  ( 85.55100297371598117, -296.0521521680024080, -421.1172536214571096 ) ) ;
#33971 = CARTESIAN_POINT ( 'NONE',  ( -32.10997743103977342, -284.0642804638028451, -343.4833112722011492 ) ) ;
#33972 = CARTESIAN_POINT ( 'NONE',  ( 28.39852645911823359, -282.8100872159531605, -232.2534203327600153 ) ) ;
#33973 = CARTESIAN_POINT ( 'NONE',  ( -107.4920760518732124, -283.6285397354857309, -290.9683537902830039 ) ) ;
#33974 = CARTESIAN_POINT ( 'NONE',  ( 16.03938483626188116, -273.2242654959118227, -219.3273305455436741 ) ) ;
#33975 = CARTESIAN_POINT ( 'NONE',  ( 34.29949583178225225, -283.1593043212120051, -250.8599200980146122 ) ) ;
#33976 = CARTESIAN_POINT ( 'NONE',  ( 25.88051309963617186, -273.5149583736509840, -232.3985397861895024 ) ) ;
#33978 = EDGE_CURVE ( 'NONE', #44024, #61775, #87503, .T. ) ;
#33977 = CARTESIAN_POINT ( 'NONE',  ( 222.8344101925596306, 0.000000000000000000, -21.49999999999998579 ) ) ;
#33979 = CARTESIAN_POINT ( 'NONE',  ( 33.19903817164158966, -276.8950740075472368, -290.3627966629713342 ) ) ;
#33980 = CARTESIAN_POINT ( 'NONE',  ( 205.7786681169002350, 32.98517505407394168, 14.49999999999999822 ) ) ;
#33981 = CARTESIAN_POINT ( 'NONE',  ( -7.936953301847952780, -277.4794296980350623, -341.3649480753508669 ) ) ;
#33982 = VERTEX_POINT ( 'NONE', #8901 ) ;
#33983 = CARTESIAN_POINT ( 'NONE',  ( 199.0883366025557848, 17.54655016013997582, 10.45170682515655436 ) ) ;
#33984 = CARTESIAN_POINT ( 'NONE',  ( -112.9215738670834810, -286.4887184956436386, -264.3698898999080029 ) ) ;
#33985 = CARTESIAN_POINT ( 'NONE',  ( -53.19430546647188152, -294.4576817735630812, -341.8365809690592414 ) ) ;
#33986 = CARTESIAN_POINT ( 'NONE',  ( -40.34309663412894054, -288.4375128050641024, -347.2136539543908498 ) ) ;
#33987 = CARTESIAN_POINT ( 'NONE',  ( -54.97635030180521909, -284.0622926803411019, -198.4262982381889913 ) ) ;
#33989 = CARTESIAN_POINT ( 'NONE',  ( -66.75203379905119050, -287.6825588362717099, -338.3350088139837339 ) ) ;
#33988 = CARTESIAN_POINT ( 'NONE',  ( -88.08780951512318325, -283.8996518100920525, -217.0675226988815893 ) ) ;
#33990 = CARTESIAN_POINT ( 'NONE',  ( -73.98177366119345777, -284.7552141577755833, -334.0164782382196904 ) ) ;
#33991 = CARTESIAN_POINT ( 'NONE',  ( 19.29282285170698685, -274.2343777784859640, -319.5489460889735938 ) ) ;
#33992 = CARTESIAN_POINT ( 'NONE',  ( 2.341958187015649173, -284.9744114329763534, -205.3100020999200126 ) ) ;
#33993 = CARTESIAN_POINT ( 'NONE',  ( -109.6994976599125238, -298.8082655502121838, -250.4370192811250035 ) ) ;
#33994 = CARTESIAN_POINT ( 'NONE',  ( 21.57126856253321279, -284.9118906762126358, -223.6577211002585557 ) ) ;
#33995 = CARTESIAN_POINT ( 'NONE',  ( -22.15728714507084263, -281.1925723890024642, -198.6652394722845543 ) ) ;
#33996 = CARTESIAN_POINT ( 'NONE',  ( 13.38570060246112625, -290.3449888207655931, -325.9002156649412996 ) ) ;
#33997 = DIRECTION ( 'NONE',  ( 0.000000000000000000, 1.000000000000000000, 0.000000000000000000 ) ) ;
#33998 = CARTESIAN_POINT ( 'NONE',  ( 195.4387718505159626, 39.61567108744358734, 13.99040197475940772 ) ) ;
#33999 = CARTESIAN_POINT ( 'NONE',  ( -95.38917135227156052, -297.8090270661739964, -318.7527617647824059 ) ) ;
#34000 = CARTESIAN_POINT ( 'NONE',  ( -107.3728874697466864, -276.9026434713559865, -243.3711692907941710 ) ) ;
#34001 = CARTESIAN_POINT ( 'NONE',  ( -39.19752279556439589, -291.2266220305182287, -193.5320000469215529 ) ) ;
#34002 = CARTESIAN_POINT ( 'NONE',  ( -100.8653498173375311, -294.4402680124741210, -308.0275480268938963 ) ) ;
#34003 = CARTESIAN_POINT ( 'NONE',  ( -36.98926432934193542, -278.7414808409349689, -196.8688104348144066 ) ) ;
#34004 = CARTESIAN_POINT ( 'NONE',  ( -24.32098240830451275, -272.2993628225917178, -197.0161142878270937 ) ) ;
#34005 = CARTESIAN_POINT ( 'NONE',  ( 35.69898607080695285, -294.9798952575358157, -278.9516643286306135 ) ) ;
#34006 = CARTESIAN_POINT ( 'NONE',  ( -37.30987171927208124, -291.5519495502701943, -345.3611179825600175 ) ) ;
#34007 = CARTESIAN_POINT ( 'NONE',  ( -113.0842082891596192, -295.1489164937283363, -261.0993573750959627 ) ) ;
#34009 = ADVANCED_FACE ( 'NONE', ( #30700 ), #22651, .F. ) ;
#34008 = CARTESIAN_POINT ( 'NONE',  ( -70.43586177752509059, -289.8617341429207954, -201.9597255801413382 ) ) ;
#34010 = AXIS2_PLACEMENT_3D ( 'NONE', #22766, #74354, #58773 ) ;
#34011 = CARTESIAN_POINT ( 'NONE',  ( -100.2244542782971877, -292.4996399343670532, -232.1363335249015734 ) ) ;
#34012 = DIRECTION ( 'NONE',  ( -0.2456588035076310295, 0.9693563597868428694, 0.000000000000000000 ) ) ;
#34013 = CARTESIAN_POINT ( 'NONE',  ( -102.5581352461478417, -291.8056555447890901, -237.0914645410217361 ) ) ;
#34014 = FACE_OUTER_BOUND ( 'NONE', #6314, .T. ) ;
#34015 = CARTESIAN_POINT ( 'NONE',  ( -79.38935137501394479, -292.7034758802020633, -206.2664310017685807 ) ) ;
#34017 = CARTESIAN_POINT ( 'NONE',  ( 34.90773852373655473, -293.4144154234762709, -259.9199200389712701 ) ) ;
#34016 = CARTESIAN_POINT ( 'NONE',  ( 22.92416737053131826, -280.1875310139956810, -315.5986247710465022 ) ) ;
#34018 = CARTESIAN_POINT ( 'NONE',  ( 34.32442234620443600, -281.1935247373220363, -242.0559225940189947 ) ) ;
#34019 = CARTESIAN_POINT ( 'NONE',  ( -79.15180197502634485, -283.2665206669882991, -334.9959358056071324 ) ) ;
#34020 = CARTESIAN_POINT ( 'NONE',  ( -2.535806182505966788, -286.5909035716658764, -336.6648404453312651 ) ) ;
#34021 = CARTESIAN_POINT ( 'NONE',  ( -68.32107128253467465, -281.6030802125077344, -337.8232854999885149 ) ) ;
#34022 = CARTESIAN_POINT ( 'NONE',  ( -40.95601238282657874, -278.4873620651294459, -194.1270171780464864 ) ) ;
#34023 = CIRCLE ( 'NONE', #76324, 24.00000000000000355 ) ;
#34024 = CARTESIAN_POINT ( 'NONE',  ( -15.48832416722109784, -285.2487406300211887, -196.7945681685554291 ) ) ;
#34025 = CARTESIAN_POINT ( 'NONE',  ( 164.2231345125756263, 264.6571197653884155, -7.500000000000000000 ) ) ;
#34026 = CARTESIAN_POINT ( 'NONE',  ( 30.58417658934985894, -294.7675374175377669, -241.3771148903026642 ) ) ;
#34027 = CARTESIAN_POINT ( 'NONE',  ( 38.96474186452985577, -276.9156468500540882, -265.4593488087880928 ) ) ;
#34028 = CARTESIAN_POINT ( 'NONE',  ( -59.20537098553337074, -277.0098052680232286, -340.0322553591669816 ) ) ;
#34029 = CARTESIAN_POINT ( 'NONE',  ( -114.2511981872462172, -290.6721558643066032, -274.0932906438868031 ) ) ;
#34030 = CARTESIAN_POINT ( 'NONE',  ( -69.87274048461915754, -281.5569754628715486, -338.5738857300366931 ) ) ;
#34031 = EDGE_CURVE ( 'NONE', #12908, #48629, #23597, .T. ) ;
#34032 = CARTESIAN_POINT ( 'NONE',  ( 35.06877942850390895, -292.7593506057716013, -281.6510474007383209 ) ) ;
#34033 = CARTESIAN_POINT ( 'NONE',  ( -108.4575962103301521, -294.2440151453465091, -294.1840055613633353 ) ) ;
#34034 = ORIENTED_EDGE ( 'NONE', *, *, #87889, .F. ) ;
#34035 = DIRECTION ( 'NONE',  ( -5.551115123125781913E-15, 0.000000000000000000, 1.000000000000000000 ) ) ;
#34036 = CARTESIAN_POINT ( 'NONE',  ( 20.23526115831166905, -292.4261569162461001, -225.3644017674343161 ) ) ;
#34037 = PLANE ( 'NONE',  #30783 ) ;
#34038 = CARTESIAN_POINT ( 'NONE',  ( 34.45848030099739390, -285.0523547857347353, -270.3937649182068412 ) ) ;
#34039 = CARTESIAN_POINT ( 'NONE',  ( -103.6405245513603006, -296.1171399088249814, -231.5616079269409795 ) ) ;
#34040 = CARTESIAN_POINT ( 'NONE',  ( -4.176559497390433862, -278.6242926352928180, -202.2265031768656911 ) ) ;
#34041 = CARTESIAN_POINT ( 'NONE',  ( -54.86800706650167569, -287.1465538443983974, -195.8887953618685458 ) ) ;
#34042 = CARTESIAN_POINT ( 'NONE',  ( -22.45776154617337284, -286.0812411442398115, -198.8426827372608727 ) ) ;
#34043 = CARTESIAN_POINT ( 'NONE',  ( -85.54426511926337184, -279.2528950300395536, -326.1711458074203733 ) ) ;
#34044 = CARTESIAN_POINT ( 'NONE',  ( -71.71005442459195933, -293.5286674088560517, -336.6374977733872811 ) ) ;
#34045 = CARTESIAN_POINT ( 'NONE',  ( -110.7441574846909589, -298.4408178982099571, -260.4834188170263474 ) ) ;
#34046 = CARTESIAN_POINT ( 'NONE',  ( -68.21835684903309982, -276.2618711082805589, -336.9614464224553672 ) ) ;
#34047 = ORIENTED_EDGE ( 'NONE', *, *, #61560, .F. ) ;
#34048 = DIRECTION ( 'NONE',  ( -0.000000000000000000, 1.000000000000000000, -0.000000000000000000 ) ) ;
#34049 = CARTESIAN_POINT ( 'NONE',  ( -114.0993797465282000, -296.3000993316945824, -263.8680149877381496 ) ) ;
#34050 = CARTESIAN_POINT ( 'NONE',  ( -56.41134552392333035, -291.2198180045460276, -342.3706854506460218 ) ) ;
#34051 = CARTESIAN_POINT ( 'NONE',  ( -113.9811632769476972, -273.7037598431215883, -270.3757807067846670 ) ) ;
#34052 = EDGE_CURVE ( 'NONE', #78455, #93104, #45051, .T. ) ;
#34053 = CARTESIAN_POINT ( 'NONE',  ( -42.66306414405371328, -289.7723305437850740, -343.3197876190436091 ) ) ;
#34054 = CARTESIAN_POINT ( 'NONE',  ( -48.18343439338448064, -254.8206355561004273, -445.4195540462232543 ) ) ;
#34055 = ORIENTED_EDGE ( 'NONE', *, *, #92271, .F. ) ;
#34056 = CARTESIAN_POINT ( 'NONE',  ( 39.29344655529643404, -280.6773327982243700, -275.6566465591066617 ) ) ;
#34057 = CARTESIAN_POINT ( 'NONE',  ( -97.27212975846579468, -297.8501493462121630, -222.1775482569719600 ) ) ;
#34058 = CARTESIAN_POINT ( 'NONE',  ( -67.80994736009630230, -289.7961396489703247, -200.9784651223534695 ) ) ;
#34059 = CARTESIAN_POINT ( 'NONE',  ( -91.62362531028934143, -297.6373943008153446, -215.7789149307212426 ) ) ;
#34060 = CARTESIAN_POINT ( 'NONE',  ( 22.95284970476897612, -294.4594706035056788, -311.6400159918918575 ) ) ;
#34061 = LINE ( 'NONE', #25995, #38838 ) ;
#34062 = FILL_AREA_STYLE_COLOUR ( '', #59923 ) ;
#34063 = FACE_OUTER_BOUND ( 'NONE', #64380, .T. ) ;
#34064 = CARTESIAN_POINT ( 'NONE',  ( -40.29239099905376520, -290.6086970247865793, -346.6236799829580377 ) ) ;
#34065 = CARTESIAN_POINT ( 'NONE',  ( -115.3430155898818299, -275.2662352645559167, -252.5904736702033517 ) ) ;
#34066 = CARTESIAN_POINT ( 'NONE',  ( 24.16857221796717070, -281.5157951686662159, -316.5108653582693705 ) ) ;
#34067 = CARTESIAN_POINT ( 'NONE',  ( -74.48724569931793837, -287.5570800579903903, -205.3829050902639892 ) ) ;
#34068 = CARTESIAN_POINT ( 'NONE',  ( -30.91518192134769194, -284.7065671193287244, -194.2078817765512326 ) ) ;
#34069 = CARTESIAN_POINT ( 'NONE',  ( -82.14886478029592354, -271.4397368046327301, -210.3599260659470076 ) ) ;
#34070 = CARTESIAN_POINT ( 'NONE',  ( -57.27018824581460166, -275.7133050650101609, -198.5844903303144235 ) ) ;
#34071 = CARTESIAN_POINT ( 'NONE',  ( -109.1343325549277949, -288.8869285131793845, -250.6854444463411085 ) ) ;
#34072 = CARTESIAN_POINT ( 'NONE',  ( -105.2279313368564857, -279.9717745156498268, -304.1207988128684860 ) ) ;
#34073 = VERTEX_POINT ( 'NONE', #67624 ) ;
#34074 = EDGE_CURVE ( 'NONE', #58890, #63355, #11078, .T. ) ;
#34076 = CARTESIAN_POINT ( 'NONE',  ( 0.4597544453736828185, -279.9185308260847478, -207.7330151771021463 ) ) ;
#34075 = CARTESIAN_POINT ( 'NONE',  ( -74.50578879177095359, -279.5432581245993333, -207.4712528357910628 ) ) ;
#34077 = CARTESIAN_POINT ( 'NONE',  ( -41.35446724305695199, -278.1812004345095488, -346.9601094228135025 ) ) ;
#34078 = CARTESIAN_POINT ( 'NONE',  ( -98.25125140309884841, -277.9698254411319454, -223.8850971725964598 ) ) ;
#34079 = CARTESIAN_POINT ( 'NONE',  ( 23.96410439411992144, -22.95231442736623961, -342.3546796976241922 ) ) ;
#34080 = CARTESIAN_POINT ( 'NONE',  ( -31.29060213888120501, -275.0680370213951846, -193.8220356742286867 ) ) ;
#34081 = CARTESIAN_POINT ( 'NONE',  ( -113.6490859602314458, -274.1078910969521871, -267.5387840032006466 ) ) ;
#34082 = CARTESIAN_POINT ( 'NONE',  ( -95.99890600148557951, -287.6948066931273615, -223.6242672951989618 ) ) ;
#34083 = ORIENTED_EDGE ( 'NONE', *, *, #9771, .F. ) ;
#34084 = CARTESIAN_POINT ( 'NONE',  ( 154.7659666677267865, 20.47222690886501439, -12.53936336329526391 ) ) ;
#34085 = CARTESIAN_POINT ( 'NONE',  ( 33.38377129521822440, -288.8878382860228839, -289.8403967537881840 ) ) ;
#34086 = CARTESIAN_POINT ( 'NONE',  ( 37.67825218094539252, -289.4694715674509666, -282.7638406731388159 ) ) ;
#34087 = CARTESIAN_POINT ( 'NONE',  ( -107.8480086104094511, -290.1554643315773774, -251.0543022790026555 ) ) ;
#34088 = AXIS2_PLACEMENT_3D ( 'NONE', #24148, #40206, #75746 ) ;
#34089 = CARTESIAN_POINT ( 'NONE',  ( -94.35776859030636388, -283.3573122073266290, -322.0400717641096549 ) ) ;
#34090 = CARTESIAN_POINT ( 'NONE',  ( -24.71974998225321585, -278.6157439033871697, -197.6484864261477128 ) ) ;
#34091 = CARTESIAN_POINT ( 'NONE',  ( -6.525001032820303415, -288.3216011438467490, -202.8105302942128674 ) ) ;
#34092 = CARTESIAN_POINT ( 'NONE',  ( 21.55244503841817760, -280.6484501256633735, -314.6785487041663032 ) ) ;
#34093 = CARTESIAN_POINT ( 'NONE',  ( -62.49335387163878863, -281.0332462661451132, -201.2520706272952680 ) ) ;
#34094 = CARTESIAN_POINT ( 'NONE',  ( -94.49725744858243104, -278.4021019860585966, -315.8918755371297493 ) ) ;
#34095 = CARTESIAN_POINT ( 'NONE',  ( -110.0491350529586896, -289.6541086403312875, -246.0780596479599467 ) ) ;
#34096 = AXIS2_PLACEMENT_3D ( 'NONE', #25904, #91227, #60988 ) ;
#34097 = CARTESIAN_POINT ( 'NONE',  ( -97.91081248409466298, -284.7218857487312107, -317.6426307511187019 ) ) ;
#34098 = CARTESIAN_POINT ( 'NONE',  ( -70.43795861538282566, -283.9690859577434594, -339.8317737581044184 ) ) ;
#34099 = CARTESIAN_POINT ( 'NONE',  ( 32.73399436149124853, -281.4482396454762920, -249.9063619019148064 ) ) ;
#34100 = ORIENTED_EDGE ( 'NONE', *, *, #50606, .T. ) ;
#34101 = CARTESIAN_POINT ( 'NONE',  ( 206.6195589736935005, 30.30844190587212594, 15.00000000000000000 ) ) ;
#34102 = CARTESIAN_POINT ( 'NONE',  ( -112.5839257842204120, -292.2941684954919879, -279.6763025183694822 ) ) ;
#34103 = CARTESIAN_POINT ( 'NONE',  ( -53.27018935036315384, -290.5369703425506600, -195.4766199927961736 ) ) ;
#34104 = CARTESIAN_POINT ( 'NONE',  ( -5.193986013452473571, -273.5447278070696484, -204.5450220920763513 ) ) ;
#34105 = CARTESIAN_POINT ( 'NONE',  ( -92.62948948336432409, -295.1676020695161924, -323.8080368340068276 ) ) ;
#34106 = CARTESIAN_POINT ( 'NONE',  ( -105.3353714735707456, -289.4112212900803911, -241.8106601527474879 ) ) ;
#34107 = CARTESIAN_POINT ( 'NONE',  ( -92.96686275007328959, -294.1046335545701140, -319.1854489888458488 ) ) ;
#34108 = CARTESIAN_POINT ( 'NONE',  ( -50.80934700523397396, -290.4329906233576253, -342.5639802035804564 ) ) ;
#34109 = LINE ( 'NONE', #11844, #67212 ) ;
#34110 = CARTESIAN_POINT ( 'NONE',  ( -112.0180864730158135, -292.6485916659394775, -262.8629131661964493 ) ) ;
#34111 = CARTESIAN_POINT ( 'NONE',  ( 34.94817831876405023, -291.2869794180836607, -249.7179989626914676 ) ) ;
#34112 = CARTESIAN_POINT ( 'NONE',  ( 0.1456907602883386610, -296.5536393596636344, -335.3792260792246225 ) ) ;
#34113 = CARTESIAN_POINT ( 'NONE',  ( -41.34774620322242811, -286.9417676393394459, -197.2229338460356587 ) ) ;
#34114 = CARTESIAN_POINT ( 'NONE',  ( 18.19280791292056065, -296.2584298847453965, -321.0921382488502900 ) ) ;
#34115 = CARTESIAN_POINT ( 'NONE',  ( -10.94785911146214907, -276.3743007225289716, -199.7239453671863316 ) ) ;
#34116 = CARTESIAN_POINT ( 'NONE',  ( -101.4093944506181231, -296.3087734224329779, -227.9167751567856612 ) ) ;
#34117 = CARTESIAN_POINT ( 'NONE',  ( 34.21625681899154614, -274.0382403512223277, -289.2670115886104441 ) ) ;
#34118 = CARTESIAN_POINT ( 'NONE',  ( -27.34117906137161924, -278.2599127589096497, -196.5437218858108110 ) ) ;
#34119 = CARTESIAN_POINT ( 'NONE',  ( -63.46229987583587473, -274.9091260301817101, -201.7556787663423847 ) ) ;
#34120 = CARTESIAN_POINT ( 'NONE',  ( -73.57685916769965218, -296.9684271807299751, -334.4110060935207116 ) ) ;
#34121 = CARTESIAN_POINT ( 'NONE',  ( 156.4851178187871312, 6.488953147413177264E-16, 8.757359312880714342 ) ) ;
#34122 = CARTESIAN_POINT ( 'NONE',  ( -109.8977365114597831, -297.4836636431418242, -260.5852763454557248 ) ) ;
#34123 = DIRECTION ( 'NONE',  ( 0.000000000000000000, -0.000000000000000000, -1.000000000000000000 ) ) ;
#34125 = CARTESIAN_POINT ( 'NONE',  ( -39.16832825069231205, -298.0286293834245157, -197.3715658859814255 ) ) ;
#34124 = CARTESIAN_POINT ( 'NONE',  ( 6.946997655045254128, -286.4731799766560130, -331.3919821122094618 ) ) ;
#34126 = CARTESIAN_POINT ( 'NONE',  ( -18.18202730792959798, -286.2923489644513779, -195.7278220891037108 ) ) ;
#34127 = CARTESIAN_POINT ( 'NONE',  ( -106.4963837127592114, -289.7831786279602966, -304.2961098652312444 ) ) ;
#34128 = CARTESIAN_POINT ( 'NONE',  ( -101.6974943702453231, -298.0089557341152613, -309.5623749605413195 ) ) ;
#34129 = CARTESIAN_POINT ( 'NONE',  ( 18.43033625258885877, -292.2484930883596235, -320.2754033582658622 ) ) ;
#34130 = CARTESIAN_POINT ( 'NONE',  ( 10.72996806318832697, -279.8942709253076373, -210.3489928628017083 ) ) ;
#34131 = CARTESIAN_POINT ( 'NONE',  ( 35.77081079830085031, -291.2666405000204577, -287.0812184334320705 ) ) ;
#34132 = CARTESIAN_POINT ( 'NONE',  ( -31.99008365135278709, -278.1193823247964474, -195.5011384472874738 ) ) ;
#34133 = DIRECTION ( 'NONE',  ( -0.000000000000000000, -0.000000000000000000, -1.000000000000000000 ) ) ;
#34134 = CARTESIAN_POINT ( 'NONE',  ( -26.43093704204658678, -287.7052756228085855, -342.9940240511675142 ) ) ;
#34135 = DIRECTION ( 'NONE',  ( -1.000000000000000000, -0.000000000000000000, 0.000000000000000000 ) ) ;
#34136 = CARTESIAN_POINT ( 'NONE',  ( -59.29832019713345659, -287.3360734160912671, -342.1294428259476490 ) ) ;
#34137 = CARTESIAN_POINT ( 'NONE',  ( -95.08992131036499984, -298.7941371276687619, -224.4091499278419519 ) ) ;
#34138 = CARTESIAN_POINT ( 'NONE',  ( 26.24172034550992905, -283.5394810421779539, -312.7374667348826165 ) ) ;
#34140 = CARTESIAN_POINT ( 'NONE',  ( -7.253477599204388504, -282.6461819827468958, -336.8857243858190031 ) ) ;
#34139 = CARTESIAN_POINT ( 'NONE',  ( -23.70543015075491766, -296.2421586485600074, -195.0104836624347229 ) ) ;
#34141 = CARTESIAN_POINT ( 'NONE',  ( -100.0072663391817116, -296.1251220170856300, -315.1949358746243206 ) ) ;
#34142 = CARTESIAN_POINT ( 'NONE',  ( -85.71101201707695338, -274.7927557365734970, -214.8334300653035029 ) ) ;
#34143 = CARTESIAN_POINT ( 'NONE',  ( -38.17394810588402265, -282.0418783422173874, -195.3657313487321971 ) ) ;
#34144 = EDGE_CURVE ( 'NONE', #33982, #48324, #89669, .T. ) ;
#34145 = CARTESIAN_POINT ( 'NONE',  ( -65.92102631255339418, -272.5895162221976875, -202.8522430917905979 ) ) ;
#34146 = ORIENTED_EDGE ( 'NONE', *, *, #16095, .F. ) ;
#34147 = LINE ( 'NONE', #91881, #21152 ) ;
#34148 = CARTESIAN_POINT ( 'NONE',  ( -103.7121307357248270, -286.9861502599965775, -236.2024771924168647 ) ) ;
#34149 = DIRECTION ( 'NONE',  ( 0.5941640067486159138, -0.8043439146810467122, 0.000000000000000000 ) ) ;
#34150 = CARTESIAN_POINT ( 'NONE',  ( -88.47809603358389552, -270.9094976428775681, -206.1857440867352693 ) ) ;
#34151 = CARTESIAN_POINT ( 'NONE',  ( 39.54570447168232050, -274.7595855121853674, -271.1801476732283049 ) ) ;
#34152 = CARTESIAN_POINT ( 'NONE',  ( -95.79067256070787550, -288.2870132970578538, -319.2706062192905279 ) ) ;
#34153 = CARTESIAN_POINT ( 'NONE',  ( -89.37021202850928603, -285.3208969136950373, -322.6222017936670454 ) ) ;
#34154 = PRESENTATION_LAYER_ASSIGNMENT (  '', '', ( #26576 ) ) ;
#34155 = CARTESIAN_POINT ( 'NONE',  ( 22.92245501723914103, -276.5638357021172737, -227.7402827711986220 ) ) ;
#34156 = CARTESIAN_POINT ( 'NONE',  ( -68.92619799722855589, -284.8846154903290540, -339.9529003934567868 ) ) ;
#34157 = CARTESIAN_POINT ( 'NONE',  ( -70.40747916372360748, -282.2929650765553902, -335.9021511718655688 ) ) ;
#34158 = CARTESIAN_POINT ( 'NONE',  ( -63.01692027197296397, -281.7181222955002227, -199.8379734364742149 ) ) ;
#34159 = CARTESIAN_POINT ( 'NONE',  ( 22.75701880966415303, -275.0738125612895146, -222.2034882017491668 ) ) ;
#34160 = CARTESIAN_POINT ( 'NONE',  ( 19.87577994980237150, -276.0851004532101456, -321.9090938423320267 ) ) ;
#34161 = CARTESIAN_POINT ( 'NONE',  ( -72.78917252419117290, -297.4455974563690575, -335.8339804502215884 ) ) ;
#34162 = CARTESIAN_POINT ( 'NONE',  ( 202.9738562182569694, 291.4636489450776367, -54.00000000000002132 ) ) ;
#34163 = ADVANCED_FACE ( 'NONE', ( #69020 ), #83668, .T. ) ;
#34164 = DIRECTION ( 'NONE',  ( 1.000000000000000000, -0.000000000000000000, 0.000000000000000000 ) ) ;
#34165 = CARTESIAN_POINT ( 'NONE',  ( -97.31153091690073609, -294.0636545742849535, -316.6636544058733307 ) ) ;
#34166 = CARTESIAN_POINT ( 'NONE',  ( 35.64881279390860414, -275.0041870897437661, -266.1416613042164840 ) ) ;
#34167 = CARTESIAN_POINT ( 'NONE',  ( -112.0594013691240320, -273.9695499620431178, -253.4710664164755940 ) ) ;
#34168 = CARTESIAN_POINT ( 'NONE',  ( -72.88000030762979975, -287.3347175841545322, -205.4236458839362740 ) ) ;
#34169 = CARTESIAN_POINT ( 'NONE',  ( 0.2162673356445698469, -296.0816087897763396, -336.7998545558571095 ) ) ;
#34170 = CARTESIAN_POINT ( 'NONE',  ( -22.16114993015452939, -296.0669233517037355, -345.4448020502308054 ) ) ;
#34171 = CARTESIAN_POINT ( 'NONE',  ( -107.7490710117445047, -292.2229007735709843, -295.7152212084682787 ) ) ;
#34172 = CARTESIAN_POINT ( 'NONE',  ( -32.82759728356906948, -278.1090144360034060, -195.6640544304578384 ) ) ;
#34173 = CARTESIAN_POINT ( 'NONE',  ( -92.37762154732315878, -281.1770942952284713, -220.2376548908851532 ) ) ;
#34174 = CARTESIAN_POINT ( 'NONE',  ( -69.15452005819952319, -293.5536797952444203, -337.6748891966883548 ) ) ;
#34175 = CARTESIAN_POINT ( 'NONE',  ( -105.8780573088721439, -285.9921136731020965, -302.6577621141794339 ) ) ;
#34176 = CARTESIAN_POINT ( 'NONE',  ( -96.81759069273830676, -284.0695546312793454, -227.4812839670699418 ) ) ;
#34177 = CARTESIAN_POINT ( 'NONE',  ( 203.7321165250324668, 291.7437209203117732, -83.00941222436438238 ) ) ;
#34178 = VERTEX_POINT ( 'NONE', #16950 ) ;
#34179 = CARTESIAN_POINT ( 'NONE',  ( -110.4116108969717800, -284.2116931893817764, -270.9052225107727736 ) ) ;
#34180 = VERTEX_POINT ( 'NONE', #31631 ) ;
#34181 = CARTESIAN_POINT ( 'NONE',  ( 23.49367090263939062, -282.0061579582571767, -223.6433084205988848 ) ) ;
#34182 = CARTESIAN_POINT ( 'NONE',  ( -100.7382298977241675, -273.3829978328583366, -234.0245348386029320 ) ) ;
#34183 = CARTESIAN_POINT ( 'NONE',  ( 32.35715484267636555, -285.9372595385578393, -238.4516400640781342 ) ) ;
#34184 = CARTESIAN_POINT ( 'NONE',  ( 24.39535264029694872, -281.8852234763402862, -224.7392314696223252 ) ) ;
#34185 = CARTESIAN_POINT ( 'NONE',  ( -28.66051455370715217, -278.4642198410956553, -346.2254563204683109 ) ) ;
#34186 = CARTESIAN_POINT ( 'NONE',  ( -7.584104958080704506, -281.0835276684457540, -199.4398651030447809 ) ) ;
#34187 = CARTESIAN_POINT ( 'NONE',  ( -82.13390479932374433, -275.1952119285919025, -326.4764044574609443 ) ) ;
#34188 = CARTESIAN_POINT ( 'NONE',  ( 186.3365424865488649, 263.1243791769486506, -153.3719034750679668 ) ) ;
#34189 = ORIENTED_EDGE ( 'NONE', *, *, #66440, .F. ) ;
#34190 = CARTESIAN_POINT ( 'NONE',  ( -8.281836757531388926, -276.4335520200463634, -201.3453464442936536 ) ) ;
#34191 = CARTESIAN_POINT ( 'NONE',  ( -96.00831230668778460, -239.6785672792925084, -341.5384560403468299 ) ) ;
#34192 = CARTESIAN_POINT ( 'NONE',  ( -96.06964175806390926, -277.2078255921074970, -224.2658797213836408 ) ) ;
#34193 = CARTESIAN_POINT ( 'NONE',  ( 37.08269106238812185, -295.5065568923598676, -285.6903062367455277 ) ) ;
#34194 = CARTESIAN_POINT ( 'NONE',  ( -96.49577611763895391, -295.3002576149756351, -313.3323175975022536 ) ) ;
#34195 = CARTESIAN_POINT ( 'NONE',  ( -19.39503787202268725, -291.7845599245733865, -195.4902691391098983 ) ) ;
#34196 = DIRECTION ( 'NONE',  ( 0.000000000000000000, 1.000000000000000000, 0.000000000000000000 ) ) ;
#34198 = CARTESIAN_POINT ( 'NONE',  ( 36.48117793508753692, -285.9252560597526553, -268.3103397172464497 ) ) ;
#34197 = CARTESIAN_POINT ( 'NONE',  ( -69.29815934365844043, -294.0391298202816870, -339.7828701516911565 ) ) ;
#34199 = CARTESIAN_POINT ( 'NONE',  ( 0.5189787395971917627, -294.4229559535997964, -206.5063258683094887 ) ) ;
#34200 = CARTESIAN_POINT ( 'NONE',  ( -100.8187061040173518, -285.3623745025093399, -307.4004644863990166 ) ) ;
#34201 = VERTEX_POINT ( 'NONE', #75187 ) ;
#34202 = CARTESIAN_POINT ( 'NONE',  ( -22.25180916154481636, -293.1819847042034439, -195.0399983904050885 ) ) ;
#34203 = CARTESIAN_POINT ( 'NONE',  ( -10.94769166799071236, -283.1910222452466428, -338.5421615008685876 ) ) ;
#34204 = CARTESIAN_POINT ( 'NONE',  ( -108.0146749630194876, -294.9677151944059688, -300.0507857283180329 ) ) ;
#34205 = CARTESIAN_POINT ( 'NONE',  ( -101.5546552396239832, -291.9119650482858788, -228.0654395753772405 ) ) ;
#34206 = CARTESIAN_POINT ( 'NONE',  ( -54.48180009559617076, -289.7588846097125952, -345.4207441679834574 ) ) ;
#34207 = CARTESIAN_POINT ( 'NONE',  ( 0.1668406292046996364, -286.7329591081249873, -207.6754406805349618 ) ) ;
#34208 = ORIENTED_EDGE ( 'NONE', *, *, #30839, .T. ) ;
#34209 = CARTESIAN_POINT ( 'NONE',  ( 160.5350683151633291, 250.5000000000000568, 20.22542485937379908 ) ) ;
#34210 = CARTESIAN_POINT ( 'NONE',  ( -104.8462350135037298, -297.9610003366339015, -304.8778264340903661 ) ) ;
#34211 = CARTESIAN_POINT ( 'NONE',  ( -107.3151688544295439, -295.6357149952872874, -239.2945897424149280 ) ) ;
#34212 = CARTESIAN_POINT ( 'NONE',  ( -14.22327118428249193, -279.4180640100485675, -200.8168802035525289 ) ) ;
#34213 = CARTESIAN_POINT ( 'NONE',  ( 37.17757660505726847, -275.2995487761617710, -289.5028080494026881 ) ) ;
#34214 = CARTESIAN_POINT ( 'NONE',  ( -63.30579144633913558, -296.1876606117900224, -201.3392190997583953 ) ) ;
#34215 = CARTESIAN_POINT ( 'NONE',  ( 6.139126437467123054, -278.3158928617020820, -330.5933993505445869 ) ) ;
#34216 = CARTESIAN_POINT ( 'NONE',  ( 36.58190275923615786, -273.7798708315560816, -277.1557051578701021 ) ) ;
#34217 = CARTESIAN_POINT ( 'NONE',  ( -34.26929567704836899, -296.2177434910190641, -343.6938585322489530 ) ) ;
#34218 = CARTESIAN_POINT ( 'NONE',  ( -110.6838177606650220, -297.6531287954829281, -268.7397210085400729 ) ) ;
#34219 = CARTESIAN_POINT ( 'NONE',  ( 198.3547199411611928, 26.15070318860490772, 11.03083405179678067 ) ) ;
#34220 = CARTESIAN_POINT ( 'NONE',  ( -93.09014237918928814, -297.4364882774215175, -322.3279147725669986 ) ) ;
#34221 = CARTESIAN_POINT ( 'NONE',  ( -59.58077875099814236, -295.7647791030258304, -198.5054496197738843 ) ) ;
#34222 = CARTESIAN_POINT ( 'NONE',  ( -25.40060182094608621, -292.8596558745691709, -198.1895098453764774 ) ) ;
#34223 = CARTESIAN_POINT ( 'NONE',  ( -41.19492402420804211, -274.8077769369849648, -193.5671185644905847 ) ) ;
#34224 = CARTESIAN_POINT ( 'NONE',  ( -110.9264423610149493, -289.1162361386358839, -271.1739069699857509 ) ) ;
#34225 = CARTESIAN_POINT ( 'NONE',  ( 209.1556935201577119, 29.41729090122338164, 14.69807323163421664 ) ) ;
#34226 = CARTESIAN_POINT ( 'NONE',  ( -83.54814466294099873, -273.9300773406669123, -208.7762142314838911 ) ) ;
#34227 = CARTESIAN_POINT ( 'NONE',  ( -109.3830825664299766, -296.7282134393302613, -282.2828084323656412 ) ) ;
#34228 = CARTESIAN_POINT ( 'NONE',  ( 21.57323429183614039, -282.8890158616968051, -223.3572403919718852 ) ) ;
#34229 = CARTESIAN_POINT ( 'NONE',  ( 39.21705108065572887, -280.2318014078542774, -269.9497440297685671 ) ) ;
#34230 = CARTESIAN_POINT ( 'NONE',  ( -39.96779119002608383, -276.4328925534953783, -347.2273803231823877 ) ) ;
#34231 = CARTESIAN_POINT ( 'NONE',  ( 38.81956285546804253, -279.9827276861665268, -272.7906105686262777 ) ) ;
#34232 = CARTESIAN_POINT ( 'NONE',  ( 36.45962506064223874, -279.3692829259026098, -256.0995321736932624 ) ) ;
#34233 = EDGE_CURVE ( 'NONE', #87290, #1585, #15739, .T. ) ;
#34234 = CARTESIAN_POINT ( 'NONE',  ( 20.32850651146596377, -273.4866402244899746, -224.6296565114017767 ) ) ;
#34235 = CARTESIAN_POINT ( 'NONE',  ( -111.3752657656298624, -280.3942280740383808, -282.6731257642764490 ) ) ;
#34236 = DIRECTION ( 'NONE',  ( 0.000000000000000000, 0.000000000000000000, -1.000000000000000000 ) ) ;
#34237 = CARTESIAN_POINT ( 'NONE',  ( 196.7071296363290855, 19.50333209967907422, 12.79999999999999716 ) ) ;
#34238 = CARTESIAN_POINT ( 'NONE',  ( -88.90401600159579232, -295.5798497753087872, -214.4749743809273923 ) ) ;
#34239 = CARTESIAN_POINT ( 'NONE',  ( 4.141534145870517492, -292.5943028513687523, -205.4277297367769961 ) ) ;
#34240 = CARTESIAN_POINT ( 'NONE',  ( -41.26271802641029751, -279.1015408243997058, -345.4383451556131490 ) ) ;
#34241 = CARTESIAN_POINT ( 'NONE',  ( -82.24870325765969881, -271.4397368065993419, -210.2263269272407626 ) ) ;
#34242 = DIRECTION ( 'NONE',  ( -0.7957555401921969640, -0.6056179655966498210, 0.000000000000000000 ) ) ;
#34243 = CARTESIAN_POINT ( 'NONE',  ( -6.029515109993660360, -284.5639764528982028, -339.1278342830471502 ) ) ;
#34244 = DIRECTION ( 'NONE',  ( 0.000000000000000000, 1.000000000000000000, 0.000000000000000000 ) ) ;
#34245 = CARTESIAN_POINT ( 'NONE',  ( 20.69450262605535329, -284.8969538493076925, -222.8355371794983739 ) ) ;
#34246 = DIRECTION ( 'NONE',  ( -0.8009040723493942027, 0.5987926743825080500, 0.000000000000000000 ) ) ;
#34247 = CARTESIAN_POINT ( 'NONE',  ( -26.16198268392631476, -293.7015660433197581, -342.9017577774432084 ) ) ;
#34248 = CARTESIAN_POINT ( 'NONE',  ( 9.833386922018071630, -284.8494478140071919, -213.0429128530003595 ) ) ;
#34249 = CARTESIAN_POINT ( 'NONE',  ( 158.3977298502259146, 18.03393767897227207, -9.815540976419979913 ) ) ;
#34250 = CARTESIAN_POINT ( 'NONE',  ( -48.10455602610596060, -293.1887845636665020, -344.6375315788861258 ) ) ;
#34251 = CARTESIAN_POINT ( 'NONE',  ( -2.521853637551600968, -284.9840753035919079, -202.4474094002151787 ) ) ;
#34252 = CARTESIAN_POINT ( 'NONE',  ( -52.00604184509451500, -281.4616148127890369, -197.9804177582704767 ) ) ;
#34253 = CARTESIAN_POINT ( 'NONE',  ( -18.29566738581069529, -287.4972307677866183, -196.1088809619367623 ) ) ;
#34254 = CARTESIAN_POINT ( 'NONE',  ( 35.21487320835912982, -279.5046721674019068, -247.7886196831189523 ) ) ;
#34255 = CARTESIAN_POINT ( 'NONE',  ( 22.74990013573843584, -288.1296722827345889, -311.8319100754199553 ) ) ;
#34256 = CARTESIAN_POINT ( 'NONE',  ( -35.66744503607664996, -281.4988063879697506, -196.7784320654212138 ) ) ;
#34257 = CARTESIAN_POINT ( 'NONE',  ( -4.283733509695101027, -281.3022989234690385, -205.0802637488628193 ) ) ;
#34258 = CARTESIAN_POINT ( 'NONE',  ( -49.11320288613227802, -287.8829048438245763, -195.8784366333053981 ) ) ;
#34259 = ORIENTED_EDGE ( 'NONE', *, *, #59920, .T. ) ;
#34260 = CARTESIAN_POINT ( 'NONE',  ( -82.96886876072993289, -297.2806448308252811, -208.2693808175442030 ) ) ;
#34261 = CARTESIAN_POINT ( 'NONE',  ( -112.0138432835007762, -292.5567814594156744, -268.4441217722098827 ) ) ;
#34262 = CARTESIAN_POINT ( 'NONE',  ( 206.3138962770341323, 36.06169532515022524, 14.00000000000000178 ) ) ;
#34263 = CARTESIAN_POINT ( 'NONE',  ( -119.3990491898856732, -299.0519495502701943, -270.3937649182068412 ) ) ;
#34264 = VERTEX_POINT ( 'NONE', #46283 ) ;
#34265 = CARTESIAN_POINT ( 'NONE',  ( -70.56890234192968592, -271.6148902094227537, -202.9372241164959121 ) ) ;
#34266 = PLANE ( 'NONE',  #83578 ) ;
#34267 = CARTESIAN_POINT ( 'NONE',  ( -50.35119816610198740, -293.6153083487474760, -345.4957494738908963 ) ) ;
#34268 = CARTESIAN_POINT ( 'NONE',  ( -108.6324653325803951, -272.1137697879979100, -254.1895545100026368 ) ) ;
#34269 = CARTESIAN_POINT ( 'NONE',  ( -15.62906509933307042, -290.2863070416325968, -340.8365291625216287 ) ) ;
#34270 = CARTESIAN_POINT ( 'NONE',  ( 36.70056719243410726, -283.2885614451192282, -268.5365362954483430 ) ) ;
#34271 = CARTESIAN_POINT ( 'NONE',  ( -80.19502977914541475, -291.0449205970095363, -333.6879584039279507 ) ) ;
#34272 = CARTESIAN_POINT ( 'NONE',  ( -113.6967297589361294, -291.9279614819956237, -265.5436786516995653 ) ) ;
#34273 = CARTESIAN_POINT ( 'NONE',  ( -13.96619434067755350, -288.3554475984544752, -199.0424529753610159 ) ) ;
#34274 = CARTESIAN_POINT ( 'NONE',  ( -64.74431301694771435, -279.8708442395716816, -198.3458938056077443 ) ) ;
#34275 = CARTESIAN_POINT ( 'NONE',  ( -107.0560859384605976, -294.2527519572428787, -299.6379959025505286 ) ) ;
#34276 = CARTESIAN_POINT ( 'NONE',  ( 23.40160874402737434, -282.0178754426440264, -317.7031431070628855 ) ) ;
#34277 = CARTESIAN_POINT ( 'NONE',  ( 1.234442724714710504, -276.4336878167842428, -206.9359913965263615 ) ) ;
#34278 = CARTESIAN_POINT ( 'NONE',  ( -102.0455923789670294, -275.4805209788415823, -239.2376011013261916 ) ) ;
#34279 = CARTESIAN_POINT ( 'NONE',  ( 36.60053765842658891, -274.0145484192714775, -287.9247898054573511 ) ) ;
#34280 = DIRECTION ( 'NONE',  ( 0.000000000000000000, 1.000000000000000000, 0.000000000000000000 ) ) ;
#34281 = CARTESIAN_POINT ( 'NONE',  ( 22.63170659143023755, -281.6409211059499285, -312.0885541389795321 ) ) ;
#34282 = CARTESIAN_POINT ( 'NONE',  ( -45.59152172870372510, -278.3594338719893244, -346.5712997914079665 ) ) ;
#34283 = CARTESIAN_POINT ( 'NONE',  ( -12.76765362462998965, -285.4227241999366242, -197.6360435514263827 ) ) ;
#34284 = CARTESIAN_POINT ( 'NONE',  ( -30.73858418250360458, -293.8969123540449573, -196.6429189189213105 ) ) ;
#34285 = CARTESIAN_POINT ( 'NONE',  ( -104.9091053112616976, -274.6127828019201047, -235.0179643765321771 ) ) ;
#34286 = CARTESIAN_POINT ( 'NONE',  ( -95.66270135784567685, -274.5392951448305894, -220.8236808529613882 ) ) ;
#34287 = DIRECTION ( 'NONE',  ( -0.000000000000000000, -0.000000000000000000, -1.000000000000000000 ) ) ;
#34288 = CARTESIAN_POINT ( 'NONE',  ( 35.64294824802102113, -275.3657226822650159, -268.8640856181839922 ) ) ;
#34289 = CARTESIAN_POINT ( 'NONE',  ( -70.51442155949654023, -297.4907178355592237, -337.4401682410059493 ) ) ;
#34290 = CARTESIAN_POINT ( 'NONE',  ( -98.84862977235592041, -283.1316085380729533, -227.7130625898168148 ) ) ;
#34291 = CARTESIAN_POINT ( 'NONE',  ( -16.62822348594025712, -291.9794000890979646, -196.2214108288478940 ) ) ;
#34292 = CARTESIAN_POINT ( 'NONE',  ( 10.70391374622207792, -274.4042966066276676, -327.4878699216591826 ) ) ;
#34293 = CARTESIAN_POINT ( 'NONE',  ( -38.88334677667683081, -290.6713127872788505, -346.5455241523515042 ) ) ;
#34294 = EDGE_CURVE ( 'NONE', #50747, #34264, #59867, .T. ) ;
#34295 = CARTESIAN_POINT ( 'NONE',  ( -106.8600781465329703, -289.7802122514539178, -247.0926588329597280 ) ) ;
#34296 = VERTEX_POINT ( 'NONE', #88900 ) ;
#34297 = CARTESIAN_POINT ( 'NONE',  ( 20.87341052307266409, -291.4542885754999588, -220.8476162752266703 ) ) ;
#34298 = CARTESIAN_POINT ( 'NONE',  ( -108.3719724519020673, -289.9955164926557245, -287.2959312521699076 ) ) ;
#34299 = ORIENTED_EDGE ( 'NONE', *, *, #36505, .T. ) ;
#34300 = CARTESIAN_POINT ( 'NONE',  ( 31.13957490063481259, -288.1857860432132838, -235.8385531977528728 ) ) ;
#34301 = CARTESIAN_POINT ( 'NONE',  ( -105.5355565345349049, -279.2357093591211310, -244.1103662098799418 ) ) ;
#34302 = EDGE_CURVE ( 'NONE', #12419, #11243, #68549, .T. ) ;
#34303 = CARTESIAN_POINT ( 'NONE',  ( 22.92021083850333341, -293.1096131384330761, -317.8162910149564482 ) ) ;
#34304 = CARTESIAN_POINT ( 'NONE',  ( -30.90067008694625628, -286.7829176031515317, -193.7200004453037536 ) ) ;
#34305 = CARTESIAN_POINT ( 'NONE',  ( -108.2060138686890269, -284.5010842381635712, -300.5639465899043330 ) ) ;
#34306 = CARTESIAN_POINT ( 'NONE',  ( -33.49086671121882119, -283.3356625503565738, -343.2932290516056923 ) ) ;
#34307 = CARTESIAN_POINT ( 'NONE',  ( 161.1277221853654567, 220.4622843307828362, -205.2806313236248172 ) ) ;
#34308 = CARTESIAN_POINT ( 'NONE',  ( -96.32399440117350764, -238.8988692071569346, -340.6895823940229207 ) ) ;
#34309 = CARTESIAN_POINT ( 'NONE',  ( -110.6513661324959799, -268.1078488974698075, -295.2803869936869887 ) ) ;
#34310 = CARTESIAN_POINT ( 'NONE',  ( 33.01813753705873467, -274.4826219557081117, -250.1276976304746995 ) ) ;
#34311 = CARTESIAN_POINT ( 'NONE',  ( 28.30119289759938539, -274.9145425739268376, -303.1134761622107590 ) ) ;
#34312 = CARTESIAN_POINT ( 'NONE',  ( -43.27874660773018434, -297.4868686218536027, -193.5989001875758220 ) ) ;
#34313 = CARTESIAN_POINT ( 'NONE',  ( -61.73251378320581750, -183.4071649071924242, -359.1965488161292797 ) ) ;
#34314 = CARTESIAN_POINT ( 'NONE',  ( 38.00935004060875855, -274.0692830204630468, -257.0378656803317767 ) ) ;
#34315 = CARTESIAN_POINT ( 'NONE',  ( -88.04357619820882519, -275.0916577905791200, -216.3715997071691675 ) ) ;
#34316 = CARTESIAN_POINT ( 'NONE',  ( -22.69223961301342030, -293.3237631074124465, -198.5306273864514992 ) ) ;
#34317 = ORIENTED_EDGE ( 'NONE', *, *, #4507, .T. ) ;
#34318 = CARTESIAN_POINT ( 'NONE',  ( -113.3703997158275314, -297.6276267735301531, -259.6613486210976589 ) ) ;
#34319 = CARTESIAN_POINT ( 'NONE',  ( 34.07216301272951142, -288.2485867149433147, -285.8486415548811692 ) ) ;
#34320 = CARTESIAN_POINT ( 'NONE',  ( -74.51925168996828575, -296.3361975368093226, -337.6664339425890375 ) ) ;
#34321 = CARTESIAN_POINT ( 'NONE',  ( -72.04066619508130032, -295.9910215724125919, -339.0306793425191927 ) ) ;
#34322 = CARTESIAN_POINT ( 'NONE',  ( 14.87402335077873694, -292.9800392262783362, -219.2738369918496346 ) ) ;
#34323 = ORIENTED_EDGE ( 'NONE', *, *, #14640, .F. ) ;
#34324 = CARTESIAN_POINT ( 'NONE',  ( 8.614788117518424215, -276.5964915159101452, -210.3834939606303465 ) ) ;
#34325 = EDGE_LOOP ( 'NONE', ( #31192, #26007, #64112, #19045 ) ) ;
#34326 = CARTESIAN_POINT ( 'NONE',  ( -36.74672813071549626, -279.5670981175811676, -193.4119214969759071 ) ) ;
#34327 = PRODUCT_DEFINITION_CONTEXT ( 'detailed design', #80138, 'design' ) ;
#34328 = B_SPLINE_CURVE_WITH_KNOTS ( 'NONE', 3,
 ( #31329, #53081, #74886, #24683, #82441, #27268, #40498, #76990 ),
 .UNSPECIFIED., .F., .F.,
 ( 4, 2, 2, 4 ),
 ( 0.000000000000000000, 0.001862880473700167768, 0.002794320710550249158, 0.003725760947400331199 ),
 .UNSPECIFIED. ) ;
#34329 = CARTESIAN_POINT ( 'NONE',  ( 7.734620083320801420, -277.3608841345051701, -328.1451861399400514 ) ) ;
#34330 = CARTESIAN_POINT ( 'NONE',  ( -4.287439431814018320, -276.2419815574499466, -201.9261198778575874 ) ) ;
#34331 = CARTESIAN_POINT ( 'NONE',  ( -56.53007240974637426, -275.3182346430110670, -343.2862094483174928 ) ) ;
#34332 = CARTESIAN_POINT ( 'NONE',  ( -66.86810800618894746, -298.3061433685239194, -203.4737768698030322 ) ) ;
#34333 = CARTESIAN_POINT ( 'NONE',  ( -105.2994578507293966, -295.5024658064982077, -242.1278383106127876 ) ) ;
#34334 = CYLINDRICAL_SURFACE ( 'NONE', #42697, 4.000000000000003553 ) ;
#34335 = CARTESIAN_POINT ( 'NONE',  ( 3.783775467739847631, -281.0818629129884698, -205.2734087682872826 ) ) ;
#34336 = CARTESIAN_POINT ( 'NONE',  ( 32.51700731755104101, -275.9998503382088870, -291.5884344696497692 ) ) ;
#34337 = CARTESIAN_POINT ( 'NONE',  ( 95.12341659969116847, -301.7069487475465053, -195.1494023596418401 ) ) ;
#34338 = CYLINDRICAL_SURFACE ( 'NONE', #74747, 8.000000000000000000 ) ;
#34339 = CARTESIAN_POINT ( 'NONE',  ( 25.09383745451428993, -286.2250496370473343, -232.2244509347945325 ) ) ;
#34340 = CARTESIAN_POINT ( 'NONE',  ( 9.940883578797246045, -278.9533739524090379, -213.3528190261110353 ) ) ;
#34342 = CARTESIAN_POINT ( 'NONE',  ( -67.15838207566098106, -281.5259498496460537, -338.5825810328841499 ) ) ;
#34341 = CARTESIAN_POINT ( 'NONE',  ( -62.49341625694517433, -278.2932417685403834, -201.1497904846716551 ) ) ;
#34343 = CARTESIAN_POINT ( 'NONE',  ( 36.36333724091495867, -289.3707106050999300, -256.2159359082284595 ) ) ;
#34344 = CARTESIAN_POINT ( 'NONE',  ( -54.02937501091456340, -278.4761517153036721, -341.8883748483089562 ) ) ;
#34345 = CARTESIAN_POINT ( 'NONE',  ( 153.9133111279456045, 20.47222690886501795, -13.06183683676589702 ) ) ;
#34346 = CARTESIAN_POINT ( 'NONE',  ( -1.775349572001520437, -294.5235961200840507, -204.3305541583093259 ) ) ;
#34347 = CARTESIAN_POINT ( 'NONE',  ( -31.55016583279567044, -275.2199800603388553, -346.1786885303034751 ) ) ;
#34348 = CARTESIAN_POINT ( 'NONE',  ( 33.68754545615291107, -276.4319247689645067, -287.6979399312593841 ) ) ;
#34349 = CARTESIAN_POINT ( 'NONE',  ( 30.74286868156538333, -283.9714973105206468, -302.3353627035035061 ) ) ;
#34350 = EDGE_CURVE ( 'NONE', #57488, #89567, #38247, .T. ) ;
#34351 = EDGE_CURVE ( 'NONE', #62468, #36396, #38245, .T. ) ;
#34352 = CARTESIAN_POINT ( 'NONE',  ( 2.197429475817664013, -229.5268262511776527, 22.50000000000000000 ) ) ;
#34353 = CARTESIAN_POINT ( 'NONE',  ( -41.65347839045332989, -291.0261908240518096, -345.8109723246171825 ) ) ;
#34354 = CARTESIAN_POINT ( 'NONE',  ( -109.3542225294415431, -294.8223437452031135, -249.3586537272184955 ) ) ;
#34355 = CARTESIAN_POINT ( 'NONE',  ( -112.8376330404410623, -283.9319766955698014, -255.7833246669176788 ) ) ;
#34356 = CARTESIAN_POINT ( 'NONE',  ( 208.7492649171146013, 30.13137537953640077, 14.27679763129792789 ) ) ;
#34357 = CARTESIAN_POINT ( 'NONE',  ( -31.28246849525034889, -272.8150698232893774, -197.1054365290772807 ) ) ;
#34358 = CARTESIAN_POINT ( 'NONE',  ( 32.97861392227385124, -291.3790443439824571, -246.4118958209336085 ) ) ;
#34359 = CARTESIAN_POINT ( 'NONE',  ( 169.2744399300530347, 8.542400036368780647, 9.000000000000001776 ) ) ;
#34360 = DIRECTION ( 'NONE',  ( 0.000000000000000000, -1.000000000000000000, 0.000000000000000000 ) ) ;
#34361 = CARTESIAN_POINT ( 'NONE',  ( -106.6227382823926888, -289.4463189894174207, -238.2533404958382448 ) ) ;
#34362 = CARTESIAN_POINT ( 'NONE',  ( -96.55153093812802467, -285.5410322633265991, -314.4137722981006391 ) ) ;
#34363 = CARTESIAN_POINT ( 'NONE',  ( 22.21187373955070399, -285.1518710447642206, -223.1456054474440691 ) ) ;
#34364 = CARTESIAN_POINT ( 'NONE',  ( -93.71811311218314700, -286.6436815332673973, -223.0633910003248559 ) ) ;
#34365 = CARTESIAN_POINT ( 'NONE',  ( -79.41047151466197818, -286.2709442036873497, -210.4422534570611276 ) ) ;
#34366 = CARTESIAN_POINT ( 'NONE',  ( -110.0525177619899608, -292.7858430085201462, -250.5246275286232560 ) ) ;
#34367 = CARTESIAN_POINT ( 'NONE',  ( 38.11783618578413524, -273.5707590769894750, -265.5561813837308591 ) ) ;
#34368 = CARTESIAN_POINT ( 'NONE',  ( 37.26368665711515860, -275.6480175737946183, -251.3932358063823926 ) ) ;
#34369 = CARTESIAN_POINT ( 'NONE',  ( 20.22945842752876189, -290.9594868272411077, -221.4038739008998391 ) ) ;
#34370 = CARTESIAN_POINT ( 'NONE',  ( -112.1751809025142563, -278.3246334919494416, -288.5533267873198611 ) ) ;
#34371 = CARTESIAN_POINT ( 'NONE',  ( -89.63657740796014650, -297.7733496304020377, -323.6980982053268576 ) ) ;
#34372 = CARTESIAN_POINT ( 'NONE',  ( -43.50896817468466793, -251.6512071849481629, -488.1691148443978250 ) ) ;
#34373 = LINE ( 'NONE', #92111, #75290 ) ;
#34374 = CARTESIAN_POINT ( 'NONE',  ( -99.45674586159880448, -282.6966867225173132, -309.7370110110442170 ) ) ;
#34375 = CARTESIAN_POINT ( 'NONE',  ( -105.5883585953012300, -276.9616102259463446, -239.1332106464525395 ) ) ;
#34376 = DIRECTION ( 'NONE',  ( 0.5729786897769825194, 5.686911123206608097E-15, 0.8195702660915978877 ) ) ;
#34377 = CARTESIAN_POINT ( 'NONE',  ( 38.62899887940997701, -273.9349658006638606, -262.6696517351882108 ) ) ;
#34378 = CARTESIAN_POINT ( 'NONE',  ( -29.71102177160464919, -276.3017135885889388, -343.1146765248514612 ) ) ;
#34379 = CARTESIAN_POINT ( 'NONE',  ( -31.52853196405320446, -296.4976994272366824, -343.8754043053045848 ) ) ;
#34380 = CARTESIAN_POINT ( 'NONE',  ( 26.03297098550137534, -279.8995512609359366, -227.0811265355436319 ) ) ;
#34381 = CARTESIAN_POINT ( 'NONE',  ( 14.49125631696822758, -295.2424324232451909, -322.1697811389622643 ) ) ;
#34382 = CARTESIAN_POINT ( 'NONE',  ( -69.30652115517672485, -296.7791327756492024, -339.8847979521177649 ) ) ;
#34383 = CARTESIAN_POINT ( 'NONE',  ( -34.47780499870007986, -297.9223065719783676, -197.3612017988505727 ) ) ;
#34384 = CARTESIAN_POINT ( 'NONE',  ( -111.2520230561674595, -292.7196854557986399, -257.3257027662428982 ) ) ;
#34385 = CARTESIAN_POINT ( 'NONE',  ( -95.81795164386677754, -285.3954585061459852, -220.1859557684366848 ) ) ;
#34386 = CARTESIAN_POINT ( 'NONE',  ( 27.45859864681588647, -273.1698047327267886, -231.0023116163505108 ) ) ;
#34387 = CARTESIAN_POINT ( 'NONE',  ( -6.921879216600030027, -288.4971779233227380, -341.1117311504117424 ) ) ;
#34388 = CARTESIAN_POINT ( 'NONE',  ( -19.15774003294121286, -282.2670616715863048, -197.9115887071694715 ) ) ;
#34389 = CARTESIAN_POINT ( 'NONE',  ( -83.78787137941044705, -284.4553066762796902, -213.6722582427379677 ) ) ;
#34390 = CARTESIAN_POINT ( 'NONE',  ( -15.55813322307565016, -286.7702195599200081, -342.1822380205039735 ) ) ;
#34391 = CARTESIAN_POINT ( 'NONE',  ( 168.8235619055982113, 230.3815547064285738, -190.2228674158758395 ) ) ;
#34392 = CARTESIAN_POINT ( 'NONE',  ( 35.74209824558113979, -287.0328589921418256, -268.3169883584774880 ) ) ;
#34393 = CARTESIAN_POINT ( 'NONE',  ( 157.2348298300756539, 18.48484813927058923, 11.40642999294609083 ) ) ;
#34394 = CARTESIAN_POINT ( 'NONE',  ( -35.89158398408883954, -283.9756625876280509, -347.1252036715262079 ) ) ;
#34395 = CARTESIAN_POINT ( 'NONE',  ( -113.1296680739815486, -289.4577737145420997, -282.5678426761463129 ) ) ;
#34396 = CARTESIAN_POINT ( 'NONE',  ( -110.6651107440872579, -279.8896169866504806, -291.1004012884798726 ) ) ;
#34397 = CARTESIAN_POINT ( 'NONE',  ( -108.0632179359445217, -280.2406374262168924, -241.1761014407339303 ) ) ;
#34398 = CARTESIAN_POINT ( 'NONE',  ( 25.13738525290967019, -280.8646270068728654, -232.5091624251931819 ) ) ;
#34399 = CARTESIAN_POINT ( 'NONE',  ( -27.03999911022992464, -276.1831539452681454, -196.0196911955375185 ) ) ;
#34400 = CARTESIAN_POINT ( 'NONE',  ( -81.87170042775603918, -295.6400822892362044, -333.2440651155099545 ) ) ;
#34401 = CARTESIAN_POINT ( 'NONE',  ( -80.46073557092442741, -289.4850982609135031, -209.3667043154135570 ) ) ;
#34402 = CARTESIAN_POINT ( 'NONE',  ( -105.0424347250891088, -295.8480110624270196, -242.2393006899522732 ) ) ;
#34403 = ORIENTED_EDGE ( 'NONE', *, *, #8766, .F. ) ;
#34404 = ORIENTED_EDGE ( 'NONE', *, *, #87492, .F. ) ;
#34405 = CARTESIAN_POINT ( 'NONE',  ( 1.880424467474606232, -284.4435518456094201, -333.6901038841115792 ) ) ;
#34406 = CARTESIAN_POINT ( 'NONE',  ( -108.1944290656878138, -296.4524985918720859, -252.6470326448538231 ) ) ;
#34407 = CARTESIAN_POINT ( 'NONE',  ( -11.27131494089022112, -293.4635790433106308, -198.1816136454255002 ) ) ;
#34408 = CARTESIAN_POINT ( 'NONE',  ( -92.63079257372240249, -284.5229192956703059, -318.2028465473765095 ) ) ;
#34409 = CARTESIAN_POINT ( 'NONE',  ( 1.088043482133245643, -273.6107938251679457, -203.8930754212499323 ) ) ;
#34410 = CARTESIAN_POINT ( 'NONE',  ( -112.1615808059637516, -290.9804904538661390, -288.1740737290444940 ) ) ;
#34411 = CARTESIAN_POINT ( 'NONE',  ( -77.84185929621585842, -283.6538506491528437, -206.3295430632726379 ) ) ;
#34412 = CARTESIAN_POINT ( 'NONE',  ( -90.77431561969035556, -291.6527652021401877, -214.8732379378299697 ) ) ;
#34413 = CARTESIAN_POINT ( 'NONE',  ( 29.97961654823861011, -287.5044664644527188, -241.9471960021442669 ) ) ;
#34414 = CARTESIAN_POINT ( 'NONE',  ( 157.4970531492008661, 276.0000000000000568, 16.90571646082702983 ) ) ;
#34415 = DIRECTION ( 'NONE',  ( -0.8526555397811730330, 0.000000000000000000, -0.5224734734706408812 ) ) ;
#34416 = CARTESIAN_POINT ( 'NONE',  ( 121.5961377311245286, 147.4458027207525959, -260.2603503459518492 ) ) ;
#34417 = CARTESIAN_POINT ( 'NONE',  ( -52.75843894939779943, -284.7662221351927769, -345.1481875036043334 ) ) ;
#34418 = CARTESIAN_POINT ( 'NONE',  ( -69.91165696735023971, -280.9809262143061233, -337.9199732462171255 ) ) ;
#34419 = ORIENTED_EDGE ( 'NONE', *, *, #43977, .F. ) ;
#34420 = CARTESIAN_POINT ( 'NONE',  ( 35.44498595126895424, -280.5926609329131338, -279.5103997065099861 ) ) ;
#34421 = CARTESIAN_POINT ( 'NONE',  ( 36.47198018288536048, -275.4935564024168002, -292.2544667241347724 ) ) ;
#34422 = CARTESIAN_POINT ( 'NONE',  ( -108.8614118121294183, -280.2657354845103441, -292.5562303587832389 ) ) ;
#34423 = CARTESIAN_POINT ( 'NONE',  ( 191.0641345987445163, 268.5554630237342622, -138.4309074710560310 ) ) ;
#34424 = CARTESIAN_POINT ( 'NONE',  ( 31.49856704163147469, -279.6968260851338073, -237.0787524178924741 ) ) ;
#34425 = CARTESIAN_POINT ( 'NONE',  ( -111.9526466618658986, -282.6012555446652073, -268.1131284285407901 ) ) ;
#34426 = CARTESIAN_POINT ( 'NONE',  ( -99.17073380490339218, -297.7183258460046886, -314.6214715509760254 ) ) ;
#34427 = CARTESIAN_POINT ( 'NONE',  ( 33.17774435946422074, -294.2972247446610368, -289.5135801892748759 ) ) ;
#34429 = ORIENTED_EDGE ( 'NONE', *, *, #53698, .T. ) ;
#34428 = EDGE_CURVE ( 'NONE', #72836, #76418, #33733, .T. ) ;
#34430 = CARTESIAN_POINT ( 'NONE',  ( -92.02899275269409429, -289.9351381479788756, -221.2450139474152309 ) ) ;
#34431 = CARTESIAN_POINT ( 'NONE',  ( 3.454464988765484357, -277.1707214683469260, -335.6080471256983060 ) ) ;
#34432 = CARTESIAN_POINT ( 'NONE',  ( -44.57119715687876038, -298.1249496152082656, -197.6696018032382085 ) ) ;
#34433 = EDGE_LOOP ( 'NONE', ( #5394, #4839 ) ) ;
#34434 = CARTESIAN_POINT ( 'NONE',  ( -111.5157528953660773, -271.7197193927910348, -250.6720555277861422 ) ) ;
#34435 = CARTESIAN_POINT ( 'NONE',  ( 157.4851178187871312, 15.00000000000000000, 10.00000000000000000 ) ) ;
#34436 = CYLINDRICAL_SURFACE ( 'NONE', #35525, 4.999999999999990230 ) ;
#34437 = CARTESIAN_POINT ( 'NONE',  ( 196.0143093133015384, 20.19615242270663913, 11.99999999999998757 ) ) ;
#34438 = CARTESIAN_POINT ( 'NONE',  ( 35.01084741140333989, -282.7868857179768725, -282.1651401161536796 ) ) ;
#34439 = CARTESIAN_POINT ( 'NONE',  ( -45.19128283315919248, -281.7143077829297226, -194.7286812767119102 ) ) ;
#34440 = CARTESIAN_POINT ( 'NONE',  ( -93.61052407174892664, -282.9479289194104581, -317.2357155893429308 ) ) ;
#34441 = CARTESIAN_POINT ( 'NONE',  ( 5.619022418208107439, -282.5014833054891028, -209.8198775243695025 ) ) ;
#34442 = CARTESIAN_POINT ( 'NONE',  ( 30.91294705439283064, -274.4023282231539156, -298.2818951294642602 ) ) ;
#34443 = DIRECTION ( 'NONE',  ( -0.000000000000000000, -0.000000000000000000, -1.000000000000000000 ) ) ;
#34444 = CARTESIAN_POINT ( 'NONE',  ( 175.2296996224750103, 247.0000000000001137, 0.000000000000000000 ) ) ;
#34445 = CARTESIAN_POINT ( 'NONE',  ( -84.75868227401930710, -278.4894663070232355, -330.8918373463444595 ) ) ;
#34446 = ORIENTED_EDGE ( 'NONE', *, *, #61091, .T. ) ;
#34447 = VERTEX_POINT ( 'NONE', #46743 ) ;
#34448 = LINE ( 'NONE', #49117, #20205 ) ;
#34449 = CARTESIAN_POINT ( 'NONE',  ( -108.8199239636463886, -286.7346503857783659, -245.2380410084283255 ) ) ;
#34450 = CARTESIAN_POINT ( 'NONE',  ( 25.92719344400298809, -293.2522292200643506, -307.0986850329196045 ) ) ;
#34451 = CARTESIAN_POINT ( 'NONE',  ( 34.97377452075691195, -287.2331697622225306, -296.6652753883899436 ) ) ;
#34452 = CARTESIAN_POINT ( 'NONE',  ( -38.62023927312097982, -284.2757960434743154, -196.3461698476520496 ) ) ;
#34454 = CARTESIAN_POINT ( 'NONE',  ( -29.08198625561179540, -287.1858934527450060, -343.9121284406027712 ) ) ;
#34453 = CARTESIAN_POINT ( 'NONE',  ( -81.82041076653520406, -284.0072811204997265, -211.7350212728857173 ) ) ;
#34455 = CARTESIAN_POINT ( 'NONE',  ( -76.32509074125809434, -284.7907593140988638, -332.6098479994429908 ) ) ;
#34457 = EDGE_CURVE ( 'NONE', #90280, #76413, #91148, .T. ) ;
#34456 = CARTESIAN_POINT ( 'NONE',  ( -28.85336403914640258, -274.9445047084882390, -344.9314109430496842 ) ) ;
#34458 = CARTESIAN_POINT ( 'NONE',  ( -40.75997245557036308, -284.4098419713503176, -194.1861727472378618 ) ) ;
#34459 = CARTESIAN_POINT ( 'NONE',  ( -88.26942142089335164, -299.3395460229289142, -215.2328837326363384 ) ) ;
#34460 = CARTESIAN_POINT ( 'NONE',  ( -90.58595351819140262, -283.2996294840405085, -217.3038102252114641 ) ) ;
#34461 = CARTESIAN_POINT ( 'NONE',  ( 35.92247115567383275, -282.4698039833236294, -268.5658872690150929 ) ) ;
#34462 = CARTESIAN_POINT ( 'NONE',  ( 37.77361692184092590, -289.6027893320435282, -274.3008295043401290 ) ) ;
#34463 = FACE_OUTER_BOUND ( 'NONE', #30119, .T. ) ;
#34464 = EDGE_CURVE ( 'NONE', #40097, #557, #36767, .T. ) ;
#34465 = EDGE_CURVE ( 'NONE', #1176, #44442, #60522, .T. ) ;
#34466 = CARTESIAN_POINT ( 'NONE',  ( 160.5350683151633291, 215.0000000000000568, 25.22542485937379197 ) ) ;
#34467 = CARTESIAN_POINT ( 'NONE',  ( -14.19939524585035961, -296.6744614328374041, -342.2898877545442247 ) ) ;
#34468 = CARTESIAN_POINT ( 'NONE',  ( -54.93796967040349699, -277.8258897703540811, -197.4008982300556454 ) ) ;
#34469 = CARTESIAN_POINT ( 'NONE',  ( -90.66649956086934026, -290.5168344573802415, -214.9643708368327282 ) ) ;
#34470 = CARTESIAN_POINT ( 'NONE',  ( -0.3746848051724631090, -292.9521636844906425, -334.2933756579137707 ) ) ;
#34471 = CARTESIAN_POINT ( 'NONE',  ( -57.23068963013539445, -278.4749008588608490, -199.6103471502528635 ) ) ;
#34472 = CARTESIAN_POINT ( 'NONE',  ( -40.54800285653801950, -296.1510210072717655, -196.1824271889297790 ) ) ;
#34473 = CARTESIAN_POINT ( 'NONE',  ( 21.37779253009841085, -294.2508382499786990, -226.1653641004419057 ) ) ;
#34474 = CARTESIAN_POINT ( 'NONE',  ( 10.64812456238589888, -290.9090924074130839, -330.4860931364851808 ) ) ;
#34475 = CARTESIAN_POINT ( 'NONE',  ( -113.2554394086487122, -294.9344315055139987, -278.0949359362051609 ) ) ;
#34476 = CARTESIAN_POINT ( 'NONE',  ( -48.15832248838597707, -290.7920557362944578, -343.4157190178026440 ) ) ;
#34477 = CARTESIAN_POINT ( 'NONE',  ( 20.55313342022535039, -291.1194737908845127, -221.1257645571029968 ) ) ;
#34478 = CARTESIAN_POINT ( 'NONE',  ( -109.9979881531174186, -291.8235393901262569, -282.1209556693643776 ) ) ;
#34479 = CYLINDRICAL_SURFACE ( 'NONE', #16894, 4.000000000000003553 ) ;
#34480 = CARTESIAN_POINT ( 'NONE',  ( -96.89875502240515459, -291.9483574705202500, -227.7835419696766621 ) ) ;
#34481 = B_SPLINE_CURVE_WITH_KNOTS ( 'NONE', 3,
 ( #64916, #79562, #71058, #28436, #35057, #28897, #14245, #5723, #63977, #34598 ),
 .UNSPECIFIED., .F., .F.,
 ( 4, 2, 2, 2, 4 ),
 ( -1.095445519331009314E-05, 0.001993413916517070006, 0.002494506009444649557, 0.002995598102372229541, 0.003997782288227388209 ),
 .UNSPECIFIED. ) ;
#34482 = CARTESIAN_POINT ( 'NONE',  ( 128.9467878515196162, -299.5541904835127980, -191.8695490883551713 ) ) ;
#34483 = CARTESIAN_POINT ( 'NONE',  ( -113.4173267146450428, -291.6389339432477072, -279.7708067382703234 ) ) ;
#34485 = CARTESIAN_POINT ( 'NONE',  ( 33.77542244239630520, -293.7701131912468213, -286.8890402137017759 ) ) ;
#34484 = CARTESIAN_POINT ( 'NONE',  ( 16.07534854567625615, -278.8247427304797839, -217.1369527966763258 ) ) ;
#34486 = CARTESIAN_POINT ( 'NONE',  ( 36.59971959299395650, -281.2821715439123977, -248.8274243594463258 ) ) ;
#34487 = CARTESIAN_POINT ( 'NONE',  ( -41.57222159324769706, -282.7706467632410181, -347.2759500177445489 ) ) ;
#34488 = CARTESIAN_POINT ( 'NONE',  ( 20.92532150693828186, -286.1996689714279682, -317.3183604583745705 ) ) ;
#34489 = CARTESIAN_POINT ( 'NONE',  ( 6.299435604253456056, -280.5919680786410026, -330.4137344928267908 ) ) ;
#34490 = CARTESIAN_POINT ( 'NONE',  ( -18.65505521339254358, -284.2925103443244552, -197.6726712581372283 ) ) ;
#34491 = CARTESIAN_POINT ( 'NONE',  ( 156.4851178187871312, 0.000000000000000000, -7.000000000000000888 ) ) ;
#34492 = CARTESIAN_POINT ( 'NONE',  ( -45.18269783257633065, -278.4345733944429071, -194.4058613743342789 ) ) ;
#34493 = CARTESIAN_POINT ( 'NONE',  ( -63.08467999146868976, -284.6449058034670543, -198.1199143853961857 ) ) ;
#34494 = CARTESIAN_POINT ( 'NONE',  ( 196.7540967208871052, 41.83829464925010910, 13.24991213668545775 ) ) ;
#34495 = CARTESIAN_POINT ( 'NONE',  ( -19.90266939806262769, -293.8800543272038226, -198.5983034260257796 ) ) ;
#34496 = CARTESIAN_POINT ( 'NONE',  ( -21.49484026384161695, -275.6767900491931869, -195.6116475915521278 ) ) ;
#34497 = CARTESIAN_POINT ( 'NONE',  ( -56.60983698365105710, -276.9740435781957899, -340.8467662633546524 ) ) ;
#34498 = CARTESIAN_POINT ( 'NONE',  ( -113.8132956795790278, -290.6007056543592171, -279.8063793833225645 ) ) ;
#34499 = CARTESIAN_POINT ( 'NONE',  ( -60.80812581265943351, -281.4340131131065164, -342.2394482817100538 ) ) ;
#34500 = CARTESIAN_POINT ( 'NONE',  ( -95.29325446982903713, -290.2393239521967416, -225.5836035559018171 ) ) ;
#34501 = CARTESIAN_POINT ( 'NONE',  ( -94.99089284043095915, -293.8893466730493742, -318.3557897135404460 ) ) ;
#34502 = ORIENTED_EDGE ( 'NONE', *, *, #68908, .T. ) ;
#34503 = CARTESIAN_POINT ( 'NONE',  ( 175.2296996224750103, 275.5000000000000568, 0.000000000000000000 ) ) ;
#34504 = CARTESIAN_POINT ( 'NONE',  ( 10.97619768048102173, -292.2496508454993887, -215.4905999240959034 ) ) ;
#34505 = CARTESIAN_POINT ( 'NONE',  ( 201.2104617360081704, 15.00000000000000000, 10.00000000000000000 ) ) ;
#34506 = CARTESIAN_POINT ( 'NONE',  ( 17.36665895637873192, -279.6952119285918457, -314.0302885647153062 ) ) ;
#34507 = CARTESIAN_POINT ( 'NONE',  ( -99.72332902484235717, -296.2055648554388085, -225.6246385783369419 ) ) ;
#34508 = CARTESIAN_POINT ( 'NONE',  ( 12.20262674270734671, -278.8726780447990450, -213.0403961371587798 ) ) ;
#34509 = CARTESIAN_POINT ( 'NONE',  ( -107.4807738000744024, -286.2608951435111635, -239.6703052914083969 ) ) ;
#34510 = CARTESIAN_POINT ( 'NONE',  ( 27.65910688053578426, -286.9327292443600754, -237.0247421569294204 ) ) ;
#34511 = CARTESIAN_POINT ( 'NONE',  ( -5.963997703303300923, -278.1521721042677200, -337.0544580163593764 ) ) ;
#34512 = CARTESIAN_POINT ( 'NONE',  ( -53.53011605969862075, -293.2808115628807286, -343.2825283670604790 ) ) ;
#34513 = CARTESIAN_POINT ( 'NONE',  ( -94.71401309191251983, -297.6592379747346513, -317.1398977948419429 ) ) ;
#34514 = CARTESIAN_POINT ( 'NONE',  ( -59.32848412113337133, -276.1381511209346513, -340.3876260613907334 ) ) ;
#34515 = ORIENTED_EDGE ( 'NONE', *, *, #24438, .T. ) ;
#34516 = CARTESIAN_POINT ( 'NONE',  ( 194.7373591563044215, 39.36132622696001704, 13.99999999999999822 ) ) ;
#34517 = CARTESIAN_POINT ( 'NONE',  ( -111.9492066669793502, -295.9809642571930794, -289.3738872927775105 ) ) ;
#34518 = CARTESIAN_POINT ( 'NONE',  ( -12.79032193891064750, -290.6506754433610240, -340.6358931573682867 ) ) ;
#34519 = DIRECTION ( 'NONE',  ( -0.000000000000000000, -1.000000000000000000, -0.000000000000000000 ) ) ;
#34520 = CARTESIAN_POINT ( 'NONE',  ( 20.44313945308228497, -288.8334891937228690, -315.1564373390917808 ) ) ;
#34521 = ORIENTED_EDGE ( 'NONE', *, *, #74260, .F. ) ;
#34522 = CARTESIAN_POINT ( 'NONE',  ( -67.25966938265867157, -278.7280572067947446, -199.6664553196427789 ) ) ;
#34523 = CARTESIAN_POINT ( 'NONE',  ( -92.61796089930656706, -296.4702183842724708, -323.8199599234287120 ) ) ;
#34524 = CARTESIAN_POINT ( 'NONE',  ( -106.6118312258548286, -288.2922316099459863, -301.1815219726607893 ) ) ;
#34525 = CARTESIAN_POINT ( 'NONE',  ( -101.6082741705620975, -296.3270059421107590, -312.8314635531399972 ) ) ;
#34526 = CARTESIAN_POINT ( 'NONE',  ( 30.60679580778791475, -294.2445842736326540, -297.2406384185550223 ) ) ;
#34527 = CYLINDRICAL_SURFACE ( 'NONE', #74466, 5.568361562975243650 ) ;
#34528 = FACE_OUTER_BOUND ( 'NONE', #21481, .T. ) ;
#34529 = CARTESIAN_POINT ( 'NONE',  ( 25.29378254256534220, -289.6544581035109900, -314.0351727633541827 ) ) ;
#34530 = CARTESIAN_POINT ( 'NONE',  ( -37.30987171927208124, -285.5519495502701375, -350.3611179825600175 ) ) ;
#34531 = CARTESIAN_POINT ( 'NONE',  ( 39.42683758538345984, -280.9671249108991447, -275.6621480945013332 ) ) ;
#34532 = CARTESIAN_POINT ( 'NONE',  ( -110.2046653653369219, -286.3321290529585781, -287.4762342893231448 ) ) ;
#34533 = CARTESIAN_POINT ( 'NONE',  ( 38.99009174591972737, -286.0702963164138168, -265.8712515919215207 ) ) ;
#34534 = CARTESIAN_POINT ( 'NONE',  ( -111.6822158206867499, -288.6933252414446542, -265.6200073272600548 ) ) ;
#34535 = CARTESIAN_POINT ( 'NONE',  ( 5.197654779962012306, -278.3438286377333952, -333.0564827436386395 ) ) ;
#34536 = VERTEX_POINT ( 'NONE', #54327 ) ;
#34538 = CARTESIAN_POINT ( 'NONE',  ( 34.32897561111584395, -281.0911912937279453, -284.8187613819188755 ) ) ;
#34537 = CARTESIAN_POINT ( 'NONE',  ( -89.08582096261814343, -277.8045655973551789, -321.9260632020282742 ) ) ;
#34539 = CARTESIAN_POINT ( 'NONE',  ( 27.39531376834699472, -277.1739786188628045, -311.5769053578295029 ) ) ;
#34540 = CARTESIAN_POINT ( 'NONE',  ( -86.53790579271186800, -278.1814631050417574, -211.5745152597847039 ) ) ;
#34541 = CARTESIAN_POINT ( 'NONE',  ( -112.4526163206608231, -268.5066740142938215, -295.6311755849135352 ) ) ;
#34542 = CARTESIAN_POINT ( 'NONE',  ( -55.29026660099994928, -274.7679486200987640, -195.7242023586695439 ) ) ;
#34543 = CARTESIAN_POINT ( 'NONE',  ( -40.43472329958058253, -299.4393855005943692, -193.9612445427866305 ) ) ;
#34544 = CARTESIAN_POINT ( 'NONE',  ( 35.78497577281001440, -290.2662352645559167, -287.0191576251351080 ) ) ;
#34545 = AXIS2_PLACEMENT_3D ( 'NONE', #88363, #23513, #31092 ) ;
#34546 = CARTESIAN_POINT ( 'NONE',  ( 82.67471867677929254, -297.5265350176030097, -193.8629188578358082 ) ) ;
#34547 = CARTESIAN_POINT ( 'NONE',  ( 32.96252191058563596, -288.3575734522253811, -249.5432643330654230 ) ) ;
#34548 = CARTESIAN_POINT ( 'NONE',  ( 23.04234736230505831, -288.6888163792721116, -224.2123508952122108 ) ) ;
#34549 = CARTESIAN_POINT ( 'NONE',  ( 35.75703090533297512, -286.9097485042926792, -271.0453614559516495 ) ) ;
#34550 = CARTESIAN_POINT ( 'NONE',  ( -110.6288418090038590, -283.7646319219435327, -293.8251174885087380 ) ) ;
#34551 = CARTESIAN_POINT ( 'NONE',  ( -68.84651728064750387, -278.0307267494371786, -203.6236703702743682 ) ) ;
#34552 = CARTESIAN_POINT ( 'NONE',  ( -90.56469338685171522, -287.1490864046858746, -218.5362054788905368 ) ) ;
#34553 = CARTESIAN_POINT ( 'NONE',  ( 35.16416309713526545, -280.2051275255844871, -283.6077479225878619 ) ) ;
#34554 = CARTESIAN_POINT ( 'NONE',  ( -110.6590162693105697, -279.7916875897342379, -276.1341863933739660 ) ) ;
#34555 = CARTESIAN_POINT ( 'NONE',  ( 5.437890585134830701, -276.9480443106114649, -329.6510820946421632 ) ) ;
#34556 = CARTESIAN_POINT ( 'NONE',  ( -54.42805809455079924, -288.0617348201380423, -345.0886046087621253 ) ) ;
#34557 = CARTESIAN_POINT ( 'NONE',  ( 13.58143929551368956, -283.1633392131408868, -327.9731760200120902 ) ) ;
#34558 = CARTESIAN_POINT ( 'NONE',  ( -114.2792590192606639, -285.0491637650850407, -269.9883782335236333 ) ) ;
#34559 = CARTESIAN_POINT ( 'NONE',  ( 25.56010813453520569, -282.2288590907139110, -307.5064218809916383 ) ) ;
#34560 = ORIENTED_EDGE ( 'NONE', *, *, #34465, .F. ) ;
#34561 = EDGE_LOOP ( 'NONE', ( #41948, #48478, #58414, #44534 ) ) ;
#34562 = CARTESIAN_POINT ( 'NONE',  ( 201.2509219215139922, 65.09645894978946501, 0.000000000000000000 ) ) ;
#34563 = CARTESIAN_POINT ( 'NONE',  ( -78.93641302016149552, -293.3587105215989936, -206.9723678381691343 ) ) ;
#34564 = CARTESIAN_POINT ( 'NONE',  ( -27.89327738334935702, -290.8544169359388434, -194.3866062035648667 ) ) ;
#34565 = CARTESIAN_POINT ( 'NONE',  ( -6.418763196234174906, -273.5273567616102923, -203.9745197839474429 ) ) ;
#34566 = EDGE_CURVE ( 'NONE', #14772, #27101, #45760, .T. ) ;
#34567 = CARTESIAN_POINT ( 'NONE',  ( 35.38729568571260131, -293.2177794617452378, -295.5003503322957386 ) ) ;
#34568 = CARTESIAN_POINT ( 'NONE',  ( -50.89782268737861415, -287.7082314833911028, -342.8490499431250669 ) ) ;
#34569 = CARTESIAN_POINT ( 'NONE',  ( 36.43273151372589069, -291.8693157479862066, -276.3031081989711311 ) ) ;
#34570 = CARTESIAN_POINT ( 'NONE',  ( -97.66655934481302381, -291.1775800709074247, -312.1927829385695077 ) ) ;
#34571 = CARTESIAN_POINT ( 'NONE',  ( 201.6359441630863500, 62.93935058108146308, -6.999999999999996447 ) ) ;
#34572 = CARTESIAN_POINT ( 'NONE',  ( -107.6092279252722079, -292.8944583273994340, -243.9932327443221141 ) ) ;
#34573 = CARTESIAN_POINT ( 'NONE',  ( -71.32018443880221525, -289.6044789259737513, -203.2984452164165532 ) ) ;
#34574 = CARTESIAN_POINT ( 'NONE',  ( 13.18031646314293326, -294.7580393374967684, -214.8612865770728320 ) ) ;
#34575 = CARTESIAN_POINT ( 'NONE',  ( -62.65541679911248707, -286.6558475602777776, -201.5856806804226267 ) ) ;
#34576 = CARTESIAN_POINT ( 'NONE',  ( 21.65294137701133437, -294.9138446617339469, -223.7609429230506350 ) ) ;
#34577 = EDGE_CURVE ( 'NONE', #23459, #30328, #20149, .T. ) ;
#34578 = DIRECTION ( 'NONE',  ( -0.9510565162951499785, 0.000000000000000000, 0.3090169943749582204 ) ) ;
#34579 = CARTESIAN_POINT ( 'NONE',  ( 14.86887508249319367, -276.7636118066307631, -216.0245498427186703 ) ) ;
#34580 = CARTESIAN_POINT ( 'NONE',  ( -64.21929981884952099, -294.5912615907673171, -342.3455152867368270 ) ) ;
#34581 = CARTESIAN_POINT ( 'NONE',  ( 36.02794479340695943, -273.6652770988968086, -260.6210349547996543 ) ) ;
#34582 = CARTESIAN_POINT ( 'NONE',  ( -109.3596389534653781, -276.8764407357224400, -251.4768180969392120 ) ) ;
#34583 = CARTESIAN_POINT ( 'NONE',  ( -65.98216440058961041, -274.8738942027691223, -202.7826131767733386 ) ) ;
#34584 = CARTESIAN_POINT ( 'NONE',  ( -2.807483554621384769, -273.0743087580672182, -202.1849961944236043 ) ) ;
#34585 = EDGE_CURVE ( 'NONE', #83027, #65034, #9733, .T. ) ;
#34586 = CARTESIAN_POINT ( 'NONE',  ( -71.18576188694183315, -296.9332812589670993, -335.7201018960165015 ) ) ;
#34587 = FACE_OUTER_BOUND ( 'NONE', #81554, .T. ) ;
#34588 = CARTESIAN_POINT ( 'NONE',  ( -90.16952861421962950, -298.0844593871178176, -219.6741583514998126 ) ) ;
#34589 = CARTESIAN_POINT ( 'NONE',  ( -47.80257052418233599, -229.5268262511776527, 22.50000000000000000 ) ) ;
#34591 = CARTESIAN_POINT ( 'NONE',  ( -71.66500064822257343, -297.5853211811107144, -205.9193558477847148 ) ) ;
#34590 = CARTESIAN_POINT ( 'NONE',  ( 25.01086344563809405, -285.0019460666180748, -228.0229928986286438 ) ) ;
#34592 = CARTESIAN_POINT ( 'NONE',  ( -15.41345741595617191, -286.3282382084300366, -196.4941265103896342 ) ) ;
#34593 = CARTESIAN_POINT ( 'NONE',  ( 3.165398693109778616, -288.1908857818256138, -335.8829412456078103 ) ) ;
#34594 = CARTESIAN_POINT ( 'NONE',  ( -98.65518058094846765, -297.9380413146176352, -314.2560900600401510 ) ) ;
#34595 = CARTESIAN_POINT ( 'NONE',  ( -61.63173961456090666, -293.3681722867557369, -341.1975567680864287 ) ) ;
#34596 = CARTESIAN_POINT ( 'NONE',  ( 38.63663579299326045, -280.6013040200209616, -258.5505073246328038 ) ) ;
#34597 = CARTESIAN_POINT ( 'NONE',  ( 10.64812456238590599, -290.1952119285919593, -210.2361428286349394 ) ) ;
#34598 = CARTESIAN_POINT ( 'NONE',  ( 152.4536156746142410, 130.6065089285656313, 11.50000000000000000 ) ) ;
#34599 = CARTESIAN_POINT ( 'NONE',  ( -94.42272174201055179, -288.6980192964061303, -316.5009866179692040 ) ) ;
#34600 = DIRECTION ( 'NONE',  ( 0.000000000000000000, 0.000000000000000000, -1.000000000000000000 ) ) ;
#34601 = CARTESIAN_POINT ( 'NONE',  ( -0.01766084105187968809, -286.5557158181418345, -335.4740706220597417 ) ) ;
#34602 = CARTESIAN_POINT ( 'NONE',  ( -65.90091281252909994, -299.2722726813432814, -202.3110497454203767 ) ) ;
#34603 = CARTESIAN_POINT ( 'NONE',  ( -42.40923899826706389, -281.4146846008261491, -194.1185685564796302 ) ) ;
#34605 = CARTESIAN_POINT ( 'NONE',  ( 31.97660595615275270, -281.2463814598186218, -247.3113535767344047 ) ) ;
#34604 = CARTESIAN_POINT ( 'NONE',  ( -110.6678946213038301, -294.7942415013578739, -252.9922950953641418 ) ) ;
#34606 = CARTESIAN_POINT ( 'NONE',  ( -107.7738903629742993, -297.1173305717759945, -239.1116573494658439 ) ) ;
#34607 = CARTESIAN_POINT ( 'NONE',  ( -60.75434593138362516, -299.2630604455569596, -200.4318485855384893 ) ) ;
#34608 = CARTESIAN_POINT ( 'NONE',  ( 22.14502174142588586, -282.9264981027533281, -224.6637787299186755 ) ) ;
#34610 = CARTESIAN_POINT ( 'NONE',  ( -72.04195674896796220, -272.5025988883462560, -205.7281070642440568 ) ) ;
#34609 = AXIS2_PLACEMENT_3D ( 'NONE', #20967, #14351, #13414 ) ;
#34611 = DIRECTION ( 'NONE',  ( -0.5335274993777825436, 0.8457827187922972723, 0.000000000000000000 ) ) ;
#34612 = CARTESIAN_POINT ( 'NONE',  ( -94.66946032890704998, -285.8686005303220554, -318.1667109234761028 ) ) ;
#34613 = CARTESIAN_POINT ( 'NONE',  ( 209.9972545312790544, 27.55378999303205845, 10.50000000000000000 ) ) ;
#34614 = CARTESIAN_POINT ( 'NONE',  ( -55.63300648810263738, -280.7666405000205145, -350.3538533559490702 ) ) ;
#34615 = CARTESIAN_POINT ( 'NONE',  ( -5.361322481310194732, -275.8391315646637167, -340.2282366200897741 ) ) ;
#34616 = ADVANCED_FACE ( 'NONE', ( #76587 ), #33482, .T. ) ;
#34617 = CARTESIAN_POINT ( 'NONE',  ( 14.87699211465616322, -292.6467328876990450, -219.2768713194639645 ) ) ;
#34618 = CARTESIAN_POINT ( 'NONE',  ( -18.54023596828037057, -284.3258151337365689, -341.6685865295860935 ) ) ;
#34619 = CARTESIAN_POINT ( 'NONE',  ( 35.81083249352388265, -277.0250047296078151, -260.6067658220363796 ) ) ;
#34620 = CARTESIAN_POINT ( 'NONE',  ( -93.95033009541943159, -285.2746220978633573, -321.7037033135929960 ) ) ;
#34621 = CARTESIAN_POINT ( 'NONE',  ( -18.64924441031904223, -281.6010559663841377, -341.3907197522622141 ) ) ;
#34622 = CARTESIAN_POINT ( 'NONE',  ( -92.79221043608397679, -281.2570878009652233, -219.8612015835795717 ) ) ;
#34623 = CARTESIAN_POINT ( 'NONE',  ( 38.49173738510147302, -275.5508976906021417, -256.9332699274085030 ) ) ;
#34624 = CARTESIAN_POINT ( 'NONE',  ( 34.18346728356978304, -275.7488574620611530, -299.0206531995406749 ) ) ;
#34625 = CARTESIAN_POINT ( 'NONE',  ( -85.38926932990192142, -297.6419874583990008, -327.2860134175114695 ) ) ;
#34626 = LINE ( 'NONE', #27525, #8198 ) ;
#34627 = DIRECTION ( 'NONE',  ( 0.000000000000000000, 0.000000000000000000, 1.000000000000000000 ) ) ;
#34628 = CARTESIAN_POINT ( 'NONE',  ( -71.53807847860753100, -293.6386390701184155, -337.9696469675988055 ) ) ;
#34629 = CARTESIAN_POINT ( 'NONE',  ( -7.488238461637044985, -276.1574788842698354, -337.0451435686070454 ) ) ;
#34630 = CARTESIAN_POINT ( 'NONE',  ( 37.39547355830849540, -295.2665764641240571, -285.7579561074740013 ) ) ;
#34631 = CARTESIAN_POINT ( 'NONE',  ( 37.39990805948450259, -294.9689610467435159, -287.2043182988343801 ) ) ;
#34632 = CARTESIAN_POINT ( 'NONE',  ( -91.15187720228725254, -293.2853276991290841, -218.3563752242979206 ) ) ;
#34633 = CARTESIAN_POINT ( 'NONE',  ( -111.9855820056045843, -276.6204681974154482, -265.0395277642510337 ) ) ;
#34634 = CARTESIAN_POINT ( 'NONE',  ( -109.5633322116164692, -280.2382647869965240, -288.4510574660374118 ) ) ;
#34635 = EDGE_CURVE ( 'NONE', #1470, #32542, #83001, .T. ) ;
#34636 = CARTESIAN_POINT ( 'NONE',  ( -95.07457378143783444, -293.9795390896061349, -317.3729614486250625 ) ) ;
#34637 = CARTESIAN_POINT ( 'NONE',  ( -21.95334435352920366, -284.7174162525229235, -344.5467229499233781 ) ) ;
#34638 = CARTESIAN_POINT ( 'NONE',  ( -30.48875328129863860, -285.0610285355732003, -197.3220008573639461 ) ) ;
#34639 = CARTESIAN_POINT ( 'NONE',  ( -101.9332918901048117, -256.7340164629418382, -326.1142880538245095 ) ) ;
#34640 = EDGE_LOOP ( 'NONE', ( #78207, #42943, #71372, #20870 ) ) ;
#34641 = CARTESIAN_POINT ( 'NONE',  ( -89.67504842947793975, -284.9557429666089092, -219.3640283090289245 ) ) ;
#34642 = ORIENTED_EDGE ( 'NONE', *, *, #36169, .T. ) ;
#34643 = CARTESIAN_POINT ( 'NONE',  ( 36.18627904402518425, -282.9084659525177585, -292.3413712554696531 ) ) ;
#34644 = CARTESIAN_POINT ( 'NONE',  ( -110.5420146832385768, -283.6341187876053027, -247.6056614346497895 ) ) ;
#34645 = CARTESIAN_POINT ( 'NONE',  ( -71.14182444028119789, -280.5581162100088477, -201.4381768772905446 ) ) ;
#34646 = CARTESIAN_POINT ( 'NONE',  ( -96.50444023453960085, -279.4194594291496401, -318.5736677799964127 ) ) ;
#34647 = CARTESIAN_POINT ( 'NONE',  ( -74.96531251642167604, -280.2159816878609604, -203.2956531177505610 ) ) ;
#34648 = CARTESIAN_POINT ( 'NONE',  ( -6.998514795304330072, -274.1237833571632905, -333.4427485647536855 ) ) ;
#34649 = CARTESIAN_POINT ( 'NONE',  ( 181.0651834200913015, 253.6962031844424246, -166.7746545555078512 ) ) ;
#34650 = CARTESIAN_POINT ( 'NONE',  ( -82.18959793761349886, -275.4394140274640677, -210.3903658329570305 ) ) ;
#34651 = CARTESIAN_POINT ( 'NONE',  ( 167.2772850727250784, 232.7340772729295963, -192.4600619714121592 ) ) ;
#34652 = CARTESIAN_POINT ( 'NONE',  ( -79.97407639820484349, -277.4922446216823460, -209.0885523938139841 ) ) ;
#34653 = CARTESIAN_POINT ( 'NONE',  ( 36.48095213073637666, -295.5411406815074997, -288.4209080095041600 ) ) ;
#34654 = CARTESIAN_POINT ( 'NONE',  ( 29.95282405094631173, -292.5163581805219906, -241.6774244366818607 ) ) ;
#34655 = CARTESIAN_POINT ( 'NONE',  ( -54.49400215255699464, -288.7743486719640487, -345.4179565856551335 ) ) ;
#34656 = DIRECTION ( 'NONE',  ( -1.000000000000000000, 0.000000000000000000, 0.000000000000000000 ) ) ;
#34658 = CARTESIAN_POINT ( 'NONE',  ( -60.20736029322054605, -284.1505867716117564, -200.1927347946018756 ) ) ;
#34657 = CARTESIAN_POINT ( 'NONE',  ( 26.01297138460396141, -292.6940688904533090, -313.0787009003353205 ) ) ;
#34659 = CARTESIAN_POINT ( 'NONE',  ( -17.11848132108027087, -294.1762869335290134, -198.8801473249683909 ) ) ;
#34660 = CARTESIAN_POINT ( 'NONE',  ( -52.21008618926200029, -284.3381937310760463, -198.1832900402271207 ) ) ;
#34661 = CARTESIAN_POINT ( 'NONE',  ( -101.4295112317074796, -286.3574518255425119, -234.2846269847509006 ) ) ;
#34662 = ORIENTED_EDGE ( 'NONE', *, *, #37291, .T. ) ;
#34663 = CARTESIAN_POINT ( 'NONE',  ( -25.07089793714612824, -293.1462320493814673, -194.5834984239086509 ) ) ;
#34664 = CARTESIAN_POINT ( 'NONE',  ( 34.76530516317772879, -282.1996563480080908, -282.1326187223264697 ) ) ;
#34665 = CARTESIAN_POINT ( 'NONE',  ( 37.04008665724141736, -292.1168062012749829, -252.0483215077572368 ) ) ;
#34666 = CARTESIAN_POINT ( 'NONE',  ( 18.53442655028765884, -289.0767740728888953, -323.1059498418403564 ) ) ;
#34667 = CARTESIAN_POINT ( 'NONE',  ( -108.7390208684525703, -290.6803569414378217, -299.0307795463495495 ) ) ;
#34668 = CARTESIAN_POINT ( 'NONE',  ( 35.12447126759131777, -287.8350800243681533, -279.1732691247583489 ) ) ;
#34669 = ORIENTED_EDGE ( 'NONE', *, *, #1954, .F. ) ;
#34670 = CARTESIAN_POINT ( 'NONE',  ( 201.2104617360081704, 0.000000000000000000, -9.000000000000001776 ) ) ;
#34671 = CARTESIAN_POINT ( 'NONE',  ( -93.29060163430781927, -295.9536642686580308, -218.1013100128574820 ) ) ;
#34672 = CARTESIAN_POINT ( 'NONE',  ( 29.19144475328732469, -280.1978750727375882, -239.6331852562164215 ) ) ;
#34673 = EDGE_CURVE ( 'NONE', #55168, #72836, #65699, .T. ) ;
#34674 = CARTESIAN_POINT ( 'NONE',  ( -36.93375766454642672, -273.5648192455288381, -193.4106959168321964 ) ) ;
#34675 = AXIS2_PLACEMENT_3D ( 'NONE', #6430, #35305, #29949 ) ;
#34676 = CARTESIAN_POINT ( 'NONE',  ( -61.25629503999773107, -293.8481334486833703, -340.1202990492721483 ) ) ;
#34677 = CARTESIAN_POINT ( 'NONE',  ( 23.30892874303929219, -277.8967839646896323, -312.8693635667304989 ) ) ;
#34678 = CARTESIAN_POINT ( 'NONE',  ( -109.1285212950539005, -270.9395726783268969, -251.2560937762742697 ) ) ;
#34679 = CARTESIAN_POINT ( 'NONE',  ( -92.47887531243631543, -297.0693714036058282, -318.8071954112993467 ) ) ;
#34680 = CARTESIAN_POINT ( 'NONE',  ( -104.2129662079976811, -297.2273845813862181, -300.5261238910584893 ) ) ;
#34681 = DIRECTION ( 'NONE',  ( 0.000000000000000000, 0.000000000000000000, 1.000000000000000000 ) ) ;
#34682 = CARTESIAN_POINT ( 'NONE',  ( -96.77057272029354351, -297.5062889878216765, -318.0750478232178580 ) ) ;
#34683 = CARTESIAN_POINT ( 'NONE',  ( -107.6232271891730363, -270.9257671216616359, -243.0346446930340676 ) ) ;
#34684 = CARTESIAN_POINT ( 'NONE',  ( -30.80610952973618311, -292.7883631844863999, -197.5519240320552683 ) ) ;
#34685 = CARTESIAN_POINT ( 'NONE',  ( -97.69260231538486039, -273.9924029724693924, -222.8013931459084915 ) ) ;
#34686 = CARTESIAN_POINT ( 'NONE',  ( -109.7619928982494883, -288.9559160894338561, -283.4254248234242368 ) ) ;
#34687 = CARTESIAN_POINT ( 'NONE',  ( -54.69844564832022371, -275.8292287696853577, -197.3971266540792726 ) ) ;
#34688 = CARTESIAN_POINT ( 'NONE',  ( -71.38122067187319431, -274.1069944372093232, -201.3622923063555277 ) ) ;
#34689 = CARTESIAN_POINT ( 'NONE',  ( -110.2336450172874152, -296.9426953731224330, -266.0192454640999244 ) ) ;
#34690 = CARTESIAN_POINT ( 'NONE',  ( -36.79046225364149336, -282.0389369794589811, -194.9951635931056444 ) ) ;
#34691 = CARTESIAN_POINT ( 'NONE',  ( 24.20505700632235602, -279.6291621945156862, -224.9156015909709083 ) ) ;
#34692 = CARTESIAN_POINT ( 'NONE',  ( -1.522573876527668402, -275.9384868606900341, -338.4074476517554331 ) ) ;
#34693 = CARTESIAN_POINT ( 'NONE',  ( 18.58697806780103789, -279.2397000394237807, -218.6076314252914017 ) ) ;
#34694 = CARTESIAN_POINT ( 'NONE',  ( 21.94090743705303836, -280.1846917446368934, -316.5944711029593464 ) ) ;
#34695 = EDGE_CURVE ( 'NONE', #75996, #59807, #62473, .T. ) ;
#34696 = CARTESIAN_POINT ( 'NONE',  ( 9.876952651512992176, -273.2917661412396910, -213.8517153453059052 ) ) ;
#34697 = CARTESIAN_POINT ( 'NONE',  ( -109.1561632495989329, -280.2731344996082612, -292.0311965347975729 ) ) ;
#34698 = LINE ( 'NONE', #938, #32226 ) ;
#34699 = CARTESIAN_POINT ( 'NONE',  ( 29.69732919578551034, -297.1203304518544428, -194.3941983128116533 ) ) ;
#34700 = CARTESIAN_POINT ( 'NONE',  ( 31.82488681210629622, -291.1828619517745551, -240.4547632895808817 ) ) ;
#34701 = CARTESIAN_POINT ( 'NONE',  ( -79.59441708530674475, -291.4985942665006178, -205.9257428914671948 ) ) ;
#34702 = EDGE_CURVE ( 'NONE', #25984, #40097, #29208, .T. ) ;
#34703 = CARTESIAN_POINT ( 'NONE',  ( -7.283849949174745930, -278.6590430220001053, -339.2702770704161139 ) ) ;
#34704 = CARTESIAN_POINT ( 'NONE',  ( 6.362314196337084837, -272.6451177063137266, -209.3464440268392934 ) ) ;
#34705 = CARTESIAN_POINT ( 'NONE',  ( 200.5559520117673458, 215.0000000000000568, -2.971689740512053035 ) ) ;
#34706 = CARTESIAN_POINT ( 'NONE',  ( -52.60242045280703849, -285.1661898677455724, -344.4174561643111474 ) ) ;
#34707 = CARTESIAN_POINT ( 'NONE',  ( -82.94747669176435068, -281.6754900528038661, -329.9665625475703337 ) ) ;
#34708 = CARTESIAN_POINT ( 'NONE',  ( 159.4851178187871312, 15.00000000000000000, -9.000000000000001776 ) ) ;
#34709 = CARTESIAN_POINT ( 'NONE',  ( -58.53749177896287392, -294.1273222991206353, -340.6310896649588926 ) ) ;
#34710 = CARTESIAN_POINT ( 'NONE',  ( 35.49149907240992263, -285.8788575851584710, -284.7860628873933706 ) ) ;
#34711 = CARTESIAN_POINT ( 'NONE',  ( 159.2635086430407796, 16.43186977800939275, -9.166206881811431728 ) ) ;
#34712 = CARTESIAN_POINT ( 'NONE',  ( -35.62981809008638834, -293.0305454668886114, -345.3544216147785164 ) ) ;
#34713 = CARTESIAN_POINT ( 'NONE',  ( -111.2087277765731415, -282.7897069738754112, -289.5537661668501528 ) ) ;
#34714 = CARTESIAN_POINT ( 'NONE',  ( -77.27164962212818011, -281.1075071840116379, -208.2353873607800097 ) ) ;
#34715 = CARTESIAN_POINT ( 'NONE',  ( -110.3026459722295414, -285.4617810264124387, -293.7433513925200259 ) ) ;
#34716 = CARTESIAN_POINT ( 'NONE',  ( 22.58968403144471537, -280.4246721441599561, -317.0961951208058167 ) ) ;
#34717 = CARTESIAN_POINT ( 'NONE',  ( 16.89061578888612303, -286.8522754880038974, -221.4767638214944441 ) ) ;
#34718 = CARTESIAN_POINT ( 'NONE',  ( -110.8681274788516475, -279.9376550229663962, -273.4007555625579471 ) ) ;
#34719 = CARTESIAN_POINT ( 'NONE',  ( -107.3846605697953152, -279.6341552884568955, -249.2285502331041300 ) ) ;
#34720 = CARTESIAN_POINT ( 'NONE',  ( -54.61264991168798133, -287.8111650511149264, -197.0118092379581185 ) ) ;
#34721 = VERTEX_POINT ( 'NONE', #31894 ) ;
#34722 = CARTESIAN_POINT ( 'NONE',  ( -65.54002848208352816, -297.5269281134641233, -198.6532097947270472 ) ) ;
#34723 = CARTESIAN_POINT ( 'NONE',  ( -110.7930293011079783, -292.3605303445295931, -283.6558179571153460 ) ) ;
#34724 = CARTESIAN_POINT ( 'NONE',  ( 151.9709352735115147, -299.5541904835127980, -193.4639945212225882 ) ) ;
#34725 = CARTESIAN_POINT ( 'NONE',  ( 13.84574458161073096, -296.9090924074130839, -334.4957818155094174 ) ) ;
#34726 = ORIENTED_EDGE ( 'NONE', *, *, #39657, .T. ) ;
#34727 = CARTESIAN_POINT ( 'NONE',  ( 29.62870018981954701, -273.1017076632485328, -236.2291109395855813 ) ) ;
#34728 = CARTESIAN_POINT ( 'NONE',  ( -64.00553827083086844, -293.7940943842461934, -341.7437499775447804 ) ) ;
#34729 = CARTESIAN_POINT ( 'NONE',  ( -37.81663015600997824, -297.5536962934498320, -197.3011228871214939 ) ) ;
#34730 = CARTESIAN_POINT ( 'NONE',  ( 24.83360661913408052, -289.6140798987131006, -309.9204276691947371 ) ) ;
#34731 = CARTESIAN_POINT ( 'NONE',  ( 3.241139586490572100, -282.3653760001507180, -208.4045026555773177 ) ) ;
#34732 = CARTESIAN_POINT ( 'NONE',  ( -65.21503782004542416, -290.8345052616252246, -341.5625315729826070 ) ) ;
#34733 = CARTESIAN_POINT ( 'NONE',  ( -113.8964770739265759, -291.8562635233860760, -271.2399166129128503 ) ) ;
#34734 = CARTESIAN_POINT ( 'NONE',  ( -63.27777232619048675, -287.7145853110660028, -199.9329974921880080 ) ) ;
#34735 = CARTESIAN_POINT ( 'NONE',  ( -45.27548226331739301, -280.1211034760565894, -193.7179512911521613 ) ) ;
#34736 = CARTESIAN_POINT ( 'NONE',  ( 30.91844896985933389, -292.0565619899851981, -302.8846438870362476 ) ) ;
#34737 = CARTESIAN_POINT ( 'NONE',  ( 6.186003030231581157, -280.4586625390465997, -206.8446708034898336 ) ) ;
#34738 = CARTESIAN_POINT ( 'NONE',  ( 31.30820270979395303, -277.0386460713366432, -241.9763546344181862 ) ) ;
#34739 = CARTESIAN_POINT ( 'NONE',  ( -102.0455923789670294, -281.4805209788416960, -239.2376011013261916 ) ) ;
#34740 = AXIS2_PLACEMENT_3D ( 'NONE', #18519, #26569, #19003 ) ;
#34741 = CARTESIAN_POINT ( 'NONE',  ( 154.2407498497630058, 20.33092290645582523, -11.64075539514040081 ) ) ;
#34742 = CARTESIAN_POINT ( 'NONE',  ( 27.83912614869473856, -280.6106913460508849, -237.2421286811087100 ) ) ;
#34743 = CARTESIAN_POINT ( 'NONE',  ( -42.76267528196521539, -278.3242009645552457, -346.7719925168307782 ) ) ;
#34744 = CIRCLE ( 'NONE', #61979, 5.568361562975243650 ) ;
#34745 = CARTESIAN_POINT ( 'NONE',  ( -110.0732731638158413, -274.0101703223464824, -259.4599821788766576 ) ) ;
#34746 = CARTESIAN_POINT ( 'NONE',  ( -21.02226692331584346, -285.3153897219928012, -195.3511432314969909 ) ) ;
#34747 = CARTESIAN_POINT ( 'NONE',  ( -95.93009435832956910, -292.9402799989143773, -225.1353059088673092 ) ) ;
#34748 = CARTESIAN_POINT ( 'NONE',  ( -95.43118985042337954, -274.8242034420152322, -221.0251858657978232 ) ) ;
#34749 = CARTESIAN_POINT ( 'NONE',  ( -113.0587449782604779, -274.0098918034981352, -259.0344129169586722 ) ) ;
#34750 = CARTESIAN_POINT ( 'NONE',  ( 222.8344101925596306, 3.000000000000000000, 10.00000000000000000 ) ) ;
#34751 = CARTESIAN_POINT ( 'NONE',  ( 30.27722583338860574, -275.7555522813397602, -298.0034445799832952 ) ) ;
#34752 = CARTESIAN_POINT ( 'NONE',  ( -101.7312792821809211, -298.0399770336214260, -308.5945826886912187 ) ) ;
#34753 = CARTESIAN_POINT ( 'NONE',  ( -86.07449729940954342, -281.7294940858326413, -327.1514596211674188 ) ) ;
#34754 = CARTESIAN_POINT ( 'NONE',  ( -73.42004688929604583, -291.2536529461331156, -202.3455080813807854 ) ) ;
#34755 = CARTESIAN_POINT ( 'NONE',  ( 6.339335130137395247, -274.4762028274008117, -330.9543790818390789 ) ) ;
#34756 = CARTESIAN_POINT ( 'NONE',  ( 32.14380682227470487, -289.5559589520439090, -301.6373827419291729 ) ) ;
#34757 = CARTESIAN_POINT ( 'NONE',  ( -108.9676805778728408, -289.2665994215886940, -286.0382648058151176 ) ) ;
#34758 = ORIENTED_EDGE ( 'NONE', *, *, #2889, .T. ) ;
#34759 = CARTESIAN_POINT ( 'NONE',  ( -113.4183534413896126, -289.2237107660537276, -262.6780196637561176 ) ) ;
#34760 = CARTESIAN_POINT ( 'NONE',  ( -91.68605695289608093, -290.9168724163483262, -221.5696955242788704 ) ) ;
#34761 = ORIENTED_EDGE ( 'NONE', *, *, #70954, .T. ) ;
#34762 = CARTESIAN_POINT ( 'NONE',  ( 26.87139715829713893, -288.0787222663853981, -228.4305724765549428 ) ) ;
#34763 = CARTESIAN_POINT ( 'NONE',  ( -99.48795644756521028, -279.4150983156598613, -231.9249773438579609 ) ) ;
#34764 = EDGE_CURVE ( 'NONE', #27188, #31159, #813, .T. ) ;
#34765 = CARTESIAN_POINT ( 'NONE',  ( -99.76494437933996551, -294.8789718650247664, -315.0020282840965251 ) ) ;
#34766 = CARTESIAN_POINT ( 'NONE',  ( -67.83329611510730217, -284.0933995540761430, -340.9555608303939493 ) ) ;
#34767 = CARTESIAN_POINT ( 'NONE',  ( -54.96389174355455509, -286.1648190338543145, -195.4264620875560752 ) ) ;
#34768 = CARTESIAN_POINT ( 'NONE',  ( 7.810364288832802870, -282.7494330902450201, -327.8136630376168910 ) ) ;
#34769 = CARTESIAN_POINT ( 'NONE',  ( -22.11190715825497932, -108.2714217967105412, -362.7848814367727641 ) ) ;
#34770 = CARTESIAN_POINT ( 'NONE',  ( 137.5487510745606983, 180.6726423773487227, -240.5649509146122398 ) ) ;
#34771 = CARTESIAN_POINT ( 'NONE',  ( 166.3627146848736515, 230.6933907105903927, -190.1005024542335491 ) ) ;
#34772 = CARTESIAN_POINT ( 'NONE',  ( 35.26502700774396715, -274.8729917950416848, -279.7571910365083454 ) ) ;
#34773 = CARTESIAN_POINT ( 'NONE',  ( -31.30058955305620216, -273.0505344411276951, -197.2886374975107060 ) ) ;
#34774 = CARTESIAN_POINT ( 'NONE',  ( -5.828644376177721576, -294.1564680192196874, -340.5498223488882559 ) ) ;
#34775 = CARTESIAN_POINT ( 'NONE',  ( -104.6679026044236309, -261.1202776925566127, -315.8143883333635245 ) ) ;
#34776 = CARTESIAN_POINT ( 'NONE',  ( 20.43675060126592413, -274.9192535372062594, -320.5302067277217475 ) ) ;
#34777 = CARTESIAN_POINT ( 'NONE',  ( -66.07227665129953209, -299.5325181877643672, -201.9109941376503627 ) ) ;
#34778 = CARTESIAN_POINT ( 'NONE',  ( -20.01237063769642077, -293.3596810881329020, -199.0771729337055262 ) ) ;
#34779 = ORIENTED_EDGE ( 'NONE', *, *, #51522, .T. ) ;
#34780 = CARTESIAN_POINT ( 'NONE',  ( -110.1188164666183980, -297.1849533066197182, -294.7806091769484169 ) ) ;
#34781 = CARTESIAN_POINT ( 'NONE',  ( 34.05480907052476169, -287.8400844654296975, -254.8521877769566686 ) ) ;
#34782 = CARTESIAN_POINT ( 'NONE',  ( -112.9819640328105805, -297.5243853509301175, -256.8441176792582610 ) ) ;
#34783 = CARTESIAN_POINT ( 'NONE',  ( -22.10359825035988024, -295.3543095286810853, -345.7754876624986196 ) ) ;
#34784 = CARTESIAN_POINT ( 'NONE',  ( 33.64726771441192454, -293.4936948443024676, -253.2910701396889408 ) ) ;
#34785 = ORIENTED_EDGE ( 'NONE', *, *, #32641, .F. ) ;
#34786 = CARTESIAN_POINT ( 'NONE',  ( 37.30119535383369112, -277.3216613804019062, -258.5410928806853690 ) ) ;
#34787 = ORIENTED_EDGE ( 'NONE', *, *, #30500, .F. ) ;
#34788 = EDGE_CURVE ( 'NONE', #70318, #48610, #17320, .T. ) ;
#34789 = CARTESIAN_POINT ( 'NONE',  ( 12.95667890233088926, -280.2405265742137885, -212.1408468566241936 ) ) ;
#34790 = CARTESIAN_POINT ( 'NONE',  ( -2.813278050477213910, -275.4617399140823295, -205.7763170040344676 ) ) ;
#34791 = CARTESIAN_POINT ( 'NONE',  ( 37.72302324545031382, -277.1616743738731543, -258.4764993362041423 ) ) ;
#34792 = CARTESIAN_POINT ( 'NONE',  ( -42.71460500694947626, -275.1397471290803196, -345.5245312669811710 ) ) ;
#34793 = CARTESIAN_POINT ( 'NONE',  ( -57.94143701328127349, -298.4303232501237062, -200.2216604128813913 ) ) ;
#34794 = CARTESIAN_POINT ( 'NONE',  ( -110.6881158728572956, -295.0408554218947756, -276.9343593594032882 ) ) ;
#34795 = CARTESIAN_POINT ( 'NONE',  ( 175.2296996224750103, 133.0000000000000000, 23.00000000000000711 ) ) ;
#34796 = CARTESIAN_POINT ( 'NONE',  ( -112.6585964759462541, -279.2419554157448260, -254.5847601917703287 ) ) ;
#34797 = CARTESIAN_POINT ( 'NONE',  ( 5.398504748897619443, -276.6224295686203618, -329.6035624467439220 ) ) ;
#34798 = CARTESIAN_POINT ( 'NONE',  ( 25.15202228337788526, -285.6489470938124668, -226.2042640086056906 ) ) ;
#34799 = CARTESIAN_POINT ( 'NONE',  ( 6.623143572226626752, -300.6014512949777782, -195.1794950382704030 ) ) ;
#34800 = DIRECTION ( 'NONE',  ( -1.110223024625155531E-13, 0.000000000000000000, 1.000000000000000000 ) ) ;
#34801 = CARTESIAN_POINT ( 'NONE',  ( 16.12199045057448288, -287.4667401769644357, -320.3775553551095072 ) ) ;
#34802 = ADVANCED_FACE ( 'NONE', ( #29693 ), #15621, .T. ) ;
#34803 = CARTESIAN_POINT ( 'NONE',  ( -57.36613410449184869, -278.0300052831409516, -199.1080755551348886 ) ) ;
#34805 = CARTESIAN_POINT ( 'NONE',  ( -29.31317892787824420, -281.0296350217703889, -344.4184079500287794 ) ) ;
#34804 = CARTESIAN_POINT ( 'NONE',  ( -109.1780148339836387, -277.3364987196846414, -254.3373215321235818 ) ) ;
#34807 = CARTESIAN_POINT ( 'NONE',  ( -73.18439904005735741, -287.5771708395021165, -204.4658021102520422 ) ) ;
#34806 = AXIS2_PLACEMENT_3D ( 'NONE', #90356, #67688, #83265 ) ;
#34808 = CARTESIAN_POINT ( 'NONE',  ( -35.09016331039060788, -278.2283300456271604, -343.7236498893889802 ) ) ;
#34809 = CARTESIAN_POINT ( 'NONE',  ( 219.8344101925596021, 35.72494958537217968, -7.000000000000000000 ) ) ;
#34810 = CARTESIAN_POINT ( 'NONE',  ( -97.61296734770746752, -293.1617239487760571, -225.7035667479326548 ) ) ;
#34811 = CARTESIAN_POINT ( 'NONE',  ( -90.63453748185219183, -276.0343375893257871, -324.5998270100259901 ) ) ;
#34812 = CARTESIAN_POINT ( 'NONE',  ( -1.680142477784674737, -275.1894711722507054, -206.5334170151342619 ) ) ;
#34813 = CARTESIAN_POINT ( 'NONE',  ( 34.72836271182631407, -283.8288064465004936, -291.8930104289210590 ) ) ;
#34814 = DIRECTION ( 'NONE',  ( 0.000000000000000000, 1.000000000000000000, 0.000000000000000000 ) ) ;
#34815 = CARTESIAN_POINT ( 'NONE',  ( 24.68391636086507646, -290.0544256198056701, -313.6034794155489180 ) ) ;
#34816 = CARTESIAN_POINT ( 'NONE',  ( -105.4139788496644030, -294.1370311131459516, -301.9660448810851108 ) ) ;
#34817 = CARTESIAN_POINT ( 'NONE',  ( 208.4306832106271088, -142.7221692137691775, 0.000000000000000000 ) ) ;
#34818 = CARTESIAN_POINT ( 'NONE',  ( -35.36035753594892839, -272.7623271764321089, -196.8820886809818944 ) ) ;
#34819 = CARTESIAN_POINT ( 'NONE',  ( 36.52690191429072541, -291.5896792283005539, -262.4941703303803138 ) ) ;
#34820 = CARTESIAN_POINT ( 'NONE',  ( 207.9737475149031525, 296.4638663539913637, -68.98948423471202318 ) ) ;
#34821 = FACE_OUTER_BOUND ( 'NONE', #19761, .T. ) ;
#34822 = CARTESIAN_POINT ( 'NONE',  ( -97.78706769693164347, -289.6594086705076165, -223.7667576904704276 ) ) ;
#34823 = CARTESIAN_POINT ( 'NONE',  ( 37.03631310405469890, -285.5941160179363578, -254.7453713818323990 ) ) ;
#34824 = CARTESIAN_POINT ( 'NONE',  ( -106.1220527560646616, -286.3239754578983707, -244.1955297318808675 ) ) ;
#34825 = EDGE_CURVE ( 'NONE', #68312, #12543, #61268, .T. ) ;
#34826 = CARTESIAN_POINT ( 'NONE',  ( -104.7503082324676029, -285.7373738153922886, -241.7935368588081246 ) ) ;
#34827 = CARTESIAN_POINT ( 'NONE',  ( -112.4704175978014149, -292.4492774925226968, -276.8378661692688638 ) ) ;
#34828 = B_SPLINE_CURVE_WITH_KNOTS ( 'NONE', 3,
 ( #5577, #85560, #14548, #29206, #93129, #28284 ),
 .UNSPECIFIED., .F., .F.,
 ( 4, 2, 4 ),
 ( 0.000000000000000000, 0.0009570384287224865559, 0.001914076857444973112 ),
 .UNSPECIFIED. ) ;
#34829 = CARTESIAN_POINT ( 'NONE',  ( 35.83789687934412882, -273.8719728185081976, -289.1776209214245910 ) ) ;
#34830 = CARTESIAN_POINT ( 'NONE',  ( 27.63326298442649431, -276.4277087081979971, -311.7397266418570325 ) ) ;
#34831 = CARTESIAN_POINT ( 'NONE',  ( -94.55426840664475208, -289.3114171849274499, -220.9851317030108646 ) ) ;
#34832 = CARTESIAN_POINT ( 'NONE',  ( 1.047033484055708508, -276.5548809108971682, -337.1696683886106030 ) ) ;
#34833 = CARTESIAN_POINT ( 'NONE',  ( -96.05184441720986399, -297.8962955894935476, -316.4584689309289729 ) ) ;
#34834 = CARTESIAN_POINT ( 'NONE',  ( -43.53957993923267367, -248.2613007709077522, -477.2483004490479743 ) ) ;
#34835 = CARTESIAN_POINT ( 'NONE',  ( 202.9738562182569694, 293.9636489450776367, -44.00000000000000000 ) ) ;
#34836 = CARTESIAN_POINT ( 'NONE',  ( -100.8355526829287214, -282.7324501029693806, -307.3715781910439091 ) ) ;
#34837 = CARTESIAN_POINT ( 'NONE',  ( -25.68076379665600939, -278.2005651171000977, -196.2731755745033979 ) ) ;
#34838 = CARTESIAN_POINT ( 'NONE',  ( 208.4306832106270804, -199.2391364535880882, 0.000000000000000000 ) ) ;
#34839 = CARTESIAN_POINT ( 'NONE',  ( 38.68802916633765676, -274.1140019187301959, -276.8563481443550813 ) ) ;
#34840 = CARTESIAN_POINT ( 'NONE',  ( -96.97364705169449905, -277.3108886947960059, -312.6667065204230198 ) ) ;
#34841 = CARTESIAN_POINT ( 'NONE',  ( 32.20071665298686270, -295.3954400826411870, -294.8976309867817918 ) ) ;
#34842 = CARTESIAN_POINT ( 'NONE',  ( 38.87717864663719070, -280.3599579046581880, -261.3997930701264636 ) ) ;
#34843 = CARTESIAN_POINT ( 'NONE',  ( -47.81487395849057265, -296.1297233655395189, -342.8951192446049276 ) ) ;
#34844 = CARTESIAN_POINT ( 'NONE',  ( -34.85379651485801134, -296.3366775125805361, -346.8275067401354477 ) ) ;
#34845 = CARTESIAN_POINT ( 'NONE',  ( -110.3628441122352086, -272.2189246215068579, -270.3568844605550225 ) ) ;
#34846 = CARTESIAN_POINT ( 'NONE',  ( -47.28413701110132195, -293.9259653710377052, -196.0230483558537458 ) ) ;
#34847 = CARTESIAN_POINT ( 'NONE',  ( -109.9779594186021541, -285.0411874913648944, -244.8077651540625936 ) ) ;
#34848 = CARTESIAN_POINT ( 'NONE',  ( -31.33399846250000564, -272.2668211581582796, -194.8218091159841663 ) ) ;
#34849 = CARTESIAN_POINT ( 'NONE',  ( -32.30429976689524807, -285.9473153225691249, -193.5129037078436340 ) ) ;
#34850 = CARTESIAN_POINT ( 'NONE',  ( -105.9638482691047727, -280.9179354070602130, -240.9868505978010091 ) ) ;
#34851 = CARTESIAN_POINT ( 'NONE',  ( -39.97039889651348687, -285.0770602528756967, -197.1730151826463668 ) ) ;
#34852 = CARTESIAN_POINT ( 'NONE',  ( -43.05599790272027150, -287.1241451349372369, -345.1431174888140845 ) ) ;
#34853 = CARTESIAN_POINT ( 'NONE',  ( 202.9738562182569694, 291.4636489450776367, -54.00000000000002132 ) ) ;
#34854 = CARTESIAN_POINT ( 'NONE',  ( -38.61970067576419297, -285.5433849438857123, -197.2982652854080925 ) ) ;
#34855 = CARTESIAN_POINT ( 'NONE',  ( -63.81957747868795394, -284.3303814239517919, -342.4148633659583538 ) ) ;
#34856 = CARTESIAN_POINT ( 'NONE',  ( -68.22307855902910489, -290.7151550034422485, -200.0676336702732385 ) ) ;
#34857 = CARTESIAN_POINT ( 'NONE',  ( -112.0056208560555859, -279.9590775985041091, -285.6485065458944064 ) ) ;
#34858 = CARTESIAN_POINT ( 'NONE',  ( -105.8960037863007528, -279.4266203238732373, -304.4450316289065199 ) ) ;
#34859 = CARTESIAN_POINT ( 'NONE',  ( 30.02230883784898552, -281.0081782901216343, -242.2347904490163444 ) ) ;
#34860 = CARTESIAN_POINT ( 'NONE',  ( 28.37707973213417390, -277.0705438251273449, -234.1137325286281623 ) ) ;
#34861 = CARTESIAN_POINT ( 'NONE',  ( -36.27444894065352798, -295.0391552500411763, -347.3668250999490397 ) ) ;
#34862 = CARTESIAN_POINT ( 'NONE',  ( -90.98113109435963963, -289.3059168997201596, -218.4510202373755305 ) ) ;
#34863 = CARTESIAN_POINT ( 'NONE',  ( -106.9961918954946754, -295.7764794663020780, -247.3425047631344569 ) ) ;
#34864 = VERTEX_POINT ( 'NONE', #60327 ) ;
#34865 = ORIENTED_EDGE ( 'NONE', *, *, #91068, .F. ) ;
#34866 = CARTESIAN_POINT ( 'NONE',  ( 30.63930732748062269, -283.8742929518865026, -300.8175764710408089 ) ) ;
#34867 = CARTESIAN_POINT ( 'NONE',  ( -100.1868323992704291, -295.7069111884517270, -307.6437073652548406 ) ) ;
#34868 = CARTESIAN_POINT ( 'NONE',  ( 38.30367642553348873, -294.7912890927890999, -283.0609753807915467 ) ) ;
#34869 = CARTESIAN_POINT ( 'NONE',  ( -5.981698428774349985, -283.2801980118110805, -336.4085383071718525 ) ) ;
#34870 = CARTESIAN_POINT ( 'NONE',  ( 38.49703156754828370, -274.4607172271563513, -258.3890429680355965 ) ) ;
#34871 = CARTESIAN_POINT ( 'NONE',  ( -53.37617266193706200, -292.5032411105555639, -195.0989225402719001 ) ) ;
#34872 = CARTESIAN_POINT ( 'NONE',  ( -82.52003460816783331, -283.5824377822683005, -209.4744674429073541 ) ) ;
#34873 = CIRCLE ( 'NONE', #59070, 7.999911143031724237 ) ;
#34874 = CARTESIAN_POINT ( 'NONE',  ( -113.1519346539427744, -291.0525925022996603, -256.9987591825890263 ) ) ;
#34875 = CARTESIAN_POINT ( 'NONE',  ( -15.84137413978352704, -289.0996573495766029, -340.1980800740345217 ) ) ;
#34876 = DIRECTION ( 'NONE',  ( 1.124465274301078034E-16, 1.000000000000000000, 0.000000000000000000 ) ) ;
#34877 = CARTESIAN_POINT ( 'NONE',  ( 151.9709352735115147, -299.5541904835127980, -197.7582414438974183 ) ) ;
#34878 = CARTESIAN_POINT ( 'NONE',  ( -93.57506545626765160, -238.8899425540025732, -338.5510770644321497 ) ) ;
#34879 = AXIS2_PLACEMENT_3D ( 'NONE', #3502, #32394, #3034 ) ;
#34880 = CARTESIAN_POINT ( 'NONE',  ( -71.41164631641019866, -285.0140381376205596, -338.6395664266647145 ) ) ;
#34881 = CARTESIAN_POINT ( 'NONE',  ( -106.6379572354042296, -288.4809262143061801, -236.9535640164627353 ) ) ;
#34882 = VERTEX_POINT ( 'NONE', #89164 ) ;
#34883 = CARTESIAN_POINT ( 'NONE',  ( -76.97747113672873809, -278.4281391505144256, -208.6302636669330468 ) ) ;
#34884 = CARTESIAN_POINT ( 'NONE',  ( -22.94701782041445526, -276.5396826626063671, -346.0362993238227887 ) ) ;
#34885 = CARTESIAN_POINT ( 'NONE',  ( -86.28554348697379339, -279.7328562816900330, -327.0382947923185384 ) ) ;
#34886 = CARTESIAN_POINT ( 'NONE',  ( 204.3871895515903248, 292.5236489450776958, -53.99999999999455014 ) ) ;
#34887 = CARTESIAN_POINT ( 'NONE',  ( 36.76427342440241119, -279.8920491580465182, -251.7355715855615301 ) ) ;
#34888 = CARTESIAN_POINT ( 'NONE',  ( -98.69378116030685533, -283.1518735600507739, -227.8206685669494789 ) ) ;
#34889 = CARTESIAN_POINT ( 'NONE',  ( -112.1455606784105186, -298.4815393233037639, -257.0061016257323558 ) ) ;
#34890 = CARTESIAN_POINT ( 'NONE',  ( 21.37966315882518842, -294.6534933974772343, -313.8328321831493213 ) ) ;
#34891 = VERTEX_POINT ( 'NONE', #67431 ) ;
#34892 = CARTESIAN_POINT ( 'NONE',  ( -107.4274312687419979, -288.9437451264233800, -292.6481920682344935 ) ) ;
#34893 = CARTESIAN_POINT ( 'NONE',  ( -29.85706811716175579, -274.7959605023299332, -193.8281638375711395 ) ) ;
#34894 = CARTESIAN_POINT ( 'NONE',  ( -33.81424395968752350, -298.2642020799203237, -197.3610147765085685 ) ) ;
#34895 = ORIENTED_EDGE ( 'NONE', *, *, #9842, .T. ) ;
#34896 = FACE_OUTER_BOUND ( 'NONE', #36857, .T. ) ;
#34897 = LINE ( 'NONE', #85548, #21929 ) ;
#34898 = CARTESIAN_POINT ( 'NONE',  ( 201.2104617360081704, 15.00000000000000000, 9.000000000000001776 ) ) ;
#34899 = CARTESIAN_POINT ( 'NONE',  ( -2.268733174508112516, -283.6561238650434689, -334.7502549594791503 ) ) ;
#34900 = CARTESIAN_POINT ( 'NONE',  ( -72.06402642006176507, -281.3595705509151230, -202.7572053406856583 ) ) ;
#34901 = CARTESIAN_POINT ( 'NONE',  ( -110.5545463210118555, -283.5678223541961529, -273.6367442581140494 ) ) ;
#34902 = CARTESIAN_POINT ( 'NONE',  ( 36.58003424204504483, -283.3171595060405252, -263.0057923563188069 ) ) ;
#34903 = CARTESIAN_POINT ( 'NONE',  ( 35.31244880180084067, -273.8698938981283391, -257.9538829502668591 ) ) ;
#34904 = FACE_OUTER_BOUND ( 'NONE', #88431, .T. ) ;
#34905 = CARTESIAN_POINT ( 'NONE',  ( 158.6539576904058606, 293.9636489450775230, 11.60392986742922439 ) ) ;
#34906 = CARTESIAN_POINT ( 'NONE',  ( -86.98306216611699426, -278.5254089173731131, -329.0813367292180942 ) ) ;
#34907 = ORIENTED_EDGE ( 'NONE', *, *, #89600, .F. ) ;
#34908 = ORIENTED_EDGE ( 'NONE', *, *, #48014, .T. ) ;
#34909 = DIRECTION ( 'NONE',  ( -0.2456588035076310295, 0.9693563597868428694, 0.000000000000000000 ) ) ;
#34910 = CARTESIAN_POINT ( 'NONE',  ( -109.3616792153565882, -286.8185728203726512, -248.0148332090969348 ) ) ;
#34911 = CARTESIAN_POINT ( 'NONE',  ( 26.38021410812946854, -292.2571471555543781, -234.3115893274394921 ) ) ;
#34912 = CARTESIAN_POINT ( 'NONE',  ( -23.33865316137603330, -288.2263450277679908, -346.0275100325083031 ) ) ;
#34913 = CARTESIAN_POINT ( 'NONE',  ( -109.3461984836874592, -283.0155039983598044, -253.1798373346379947 ) ) ;
#34915 = CARTESIAN_POINT ( 'NONE',  ( 22.77181050501753745, -286.3873776472089503, -313.5391199532005544 ) ) ;
#34914 = CARTESIAN_POINT ( 'NONE',  ( -67.77493950686475443, -284.2194285512869669, -203.3596787471119001 ) ) ;
#34916 = CARTESIAN_POINT ( 'NONE',  ( 35.09791540649243302, -282.9122698011261150, -282.1777421405919313 ) ) ;
#34917 = CARTESIAN_POINT ( 'NONE',  ( -3.438236613605195835, -272.4995135901275489, -203.4472000419003734 ) ) ;
#34918 = CARTESIAN_POINT ( 'NONE',  ( -101.8304722108719176, -283.4891640215544157, -229.7700020852078922 ) ) ;
#34919 = CARTESIAN_POINT ( 'NONE',  ( -64.83325620725437943, -299.6934189815007130, -200.5258398211536530 ) ) ;
#34920 = CARTESIAN_POINT ( 'NONE',  ( -102.4396543298571913, -283.0536750585918071, -232.6772915953402503 ) ) ;
#34921 = CARTESIAN_POINT ( 'NONE',  ( 35.26444115834450344, -282.3625003152594672, -260.4055710915121722 ) ) ;
#34922 = CARTESIAN_POINT ( 'NONE',  ( 37.15481515015898850, -289.4240087408247177, -260.3462471551367798 ) ) ;
#34923 = CARTESIAN_POINT ( 'NONE',  ( 196.7028786247088306, 293.4605932342957431, -7.988019280608678940 ) ) ;
#34924 = CARTESIAN_POINT ( 'NONE',  ( 169.2744399300530347, 8.542400036368780647, 13.00000000000000178 ) ) ;
#34925 = CARTESIAN_POINT ( 'NONE',  ( 24.54947000265249812, -296.0566078392772624, -313.7288034762532334 ) ) ;
#34926 = CARTESIAN_POINT ( 'NONE',  ( -110.8423043290764838, -276.7444154510166072, -255.3748753844917587 ) ) ;
#34927 = CARTESIAN_POINT ( 'NONE',  ( -107.5879083662718045, -289.3496447778621814, -301.6308894866839978 ) ) ;
#34928 = CARTESIAN_POINT ( 'NONE',  ( -37.01222086387058852, -293.4477971240663123, -344.1729452613232070 ) ) ;
#34929 = CARTESIAN_POINT ( 'NONE',  ( -95.16856964639428895, -277.8724360898360146, -224.9834368949919110 ) ) ;
#34930 = CARTESIAN_POINT ( 'NONE',  ( -110.5412695400865033, -270.8106245447466449, -256.5530495532083819 ) ) ;
#34931 = CARTESIAN_POINT ( 'NONE',  ( -104.0106643317493536, -292.2819877342362815, -239.4339019974963492 ) ) ;
#34932 = CARTESIAN_POINT ( 'NONE',  ( -110.4542110544635705, -292.8376638359844719, -287.0812184334320705 ) ) ;
#34933 = CARTESIAN_POINT ( 'NONE',  ( -108.2371887829772277, -295.3949219677122073, -241.9962210214575293 ) ) ;
#34934 = CARTESIAN_POINT ( 'NONE',  ( -66.62795018090679378, -291.0422854302788096, -338.1560749579778076 ) ) ;
#34935 = CARTESIAN_POINT ( 'NONE',  ( 23.18188603638981959, -291.1714037175487988, -224.3954982932913538 ) ) ;
#34936 = CARTESIAN_POINT ( 'NONE',  ( -110.8352560569916818, -292.0382130484377967, -265.7163704602006646 ) ) ;
#34937 = ADVANCED_FACE ( 'NONE', ( #53192 ), #75910, .F. ) ;
#34938 = CARTESIAN_POINT ( 'NONE',  ( 151.7006524173675928, 129.9758505473876369, -12.49999999999999822 ) ) ;
#34939 = CARTESIAN_POINT ( 'NONE',  ( -79.63236048067405193, -292.2673751024350963, -210.5989172900428059 ) ) ;
#34940 = DIRECTION ( 'NONE',  ( 0.000000000000000000, 0.000000000000000000, 1.000000000000000000 ) ) ;
#34941 = CARTESIAN_POINT ( 'NONE',  ( -111.5336027501511893, -291.5167690566263445, -289.4810705395530590 ) ) ;
#34943 = CARTESIAN_POINT ( 'NONE',  ( 35.29532958035327539, -293.4497953869568505, -262.6019146164438780 ) ) ;
#34942 = CARTESIAN_POINT ( 'NONE',  ( 35.94274053605528962, -279.7971243591792359, -287.9602393055343441 ) ) ;
#34944 = CARTESIAN_POINT ( 'NONE',  ( -8.861111436926220719, -280.4146078811587586, -198.8219254528337103 ) ) ;
#34945 = AXIS2_PLACEMENT_3D ( 'NONE', #78309, #55124, #19136 ) ;
#34946 = CARTESIAN_POINT ( 'NONE',  ( 37.84395955264712796, -281.4262776350673221, -286.9404779621531816 ) ) ;
#34947 = CARTESIAN_POINT ( 'NONE',  ( -10.07936173475944486, -286.6953941858417920, -340.1073845675351208 ) ) ;
#34948 = CARTESIAN_POINT ( 'NONE',  ( 35.55156021711645309, -279.5085891333641825, -256.2427748035584614 ) ) ;
#34950 = AXIS2_PLACEMENT_3D ( 'NONE', #36961, #15647, #1903 ) ;
#34949 = CARTESIAN_POINT ( 'NONE',  ( -54.48213658813285321, -283.8317529041719922, -197.3460093845242511 ) ) ;
#34951 = CARTESIAN_POINT ( 'NONE',  ( 30.11800450644896898, -279.5660576432097741, -234.5847649902923706 ) ) ;
#34952 = CARTESIAN_POINT ( 'NONE',  ( 16.09370281646036105, -285.7092527622109515, -215.3506624183742701 ) ) ;
#34953 = CARTESIAN_POINT ( 'NONE',  ( 35.17922642174686132, -276.2278375210231047, -260.7010486603462596 ) ) ;
#34954 = CARTESIAN_POINT ( 'NONE',  ( 195.6296657338482419, 40.56040261944446002, 14.76007111301385777 ) ) ;
#34955 = CARTESIAN_POINT ( 'NONE',  ( 23.99493740568049560, -294.5884971453511412, -229.3214138984063197 ) ) ;
#34956 = CARTESIAN_POINT ( 'NONE',  ( 4.525022822553224522, -276.0300438007862454, -206.3782131517272660 ) ) ;
#34957 = CARTESIAN_POINT ( 'NONE',  ( -66.81508685788679713, -277.1160456262686012, -337.1698521534723341 ) ) ;
#34958 = CARTESIAN_POINT ( 'NONE',  ( -113.6664331571216877, -290.8509697137596959, -259.7954640900600225 ) ) ;
#34959 = CARTESIAN_POINT ( 'NONE',  ( -100.2343974470069554, -282.0692527251739534, -312.3337110748246914 ) ) ;
#34960 = CARTESIAN_POINT ( 'NONE',  ( -17.35691110858699560, -291.3750699415616623, -199.8525752498121051 ) ) ;
#34961 = CARTESIAN_POINT ( 'NONE',  ( -52.89989665120770468, -293.2512535387423895, -343.7827918696546590 ) ) ;
#34962 = ORIENTED_EDGE ( 'NONE', *, *, #66220, .F. ) ;
#34963 = CARTESIAN_POINT ( 'NONE',  ( 205.7381008070597943, 1.000000000000000000, -6.999999999999991118 ) ) ;
#34964 = CARTESIAN_POINT ( 'NONE',  ( 31.86134602843300456, -292.7468925525474219, -246.7744006299952559 ) ) ;
#34965 = CARTESIAN_POINT ( 'NONE',  ( 209.0108701966262004, 28.85123441772958230, 12.07129462079433324 ) ) ;
#34966 = CARTESIAN_POINT ( 'NONE',  ( -53.35057174420112602, -280.7666405000205145, -340.3538533559490702 ) ) ;
#34967 = CARTESIAN_POINT ( 'NONE',  ( -112.3777110944119357, -295.4076895070623436, -286.5604164944611512 ) ) ;
#34968 = CARTESIAN_POINT ( 'NONE',  ( -96.77861483662742614, -285.2168214329187208, -318.5538026829544833 ) ) ;
#34969 = CARTESIAN_POINT ( 'NONE',  ( 31.84127136285350801, -287.0759960627252099, -247.0648423105714073 ) ) ;
#34970 = CARTESIAN_POINT ( 'NONE',  ( 23.04500141755317344, -277.6568034566590768, -312.6880038354847215 ) ) ;
#34971 = CARTESIAN_POINT ( 'NONE',  ( -105.2036517932926785, -294.9837849558356311, -239.1465715141204669 ) ) ;
#34972 = CARTESIAN_POINT ( 'NONE',  ( -98.00120783608370800, -297.7290415774002668, -312.7686425383072333 ) ) ;
#34973 = CARTESIAN_POINT ( 'NONE',  ( 27.10811842817485839, -274.8251463079134282, -305.5864290773352536 ) ) ;
#34974 = ORIENTED_EDGE ( 'NONE', *, *, #93458, .F. ) ;
#34975 = FACE_BOUND ( 'NONE', #60847, .T. ) ;
#34976 = CARTESIAN_POINT ( 'NONE',  ( -101.5297151710278030, -296.7782490845821144, -227.8442588243519253 ) ) ;
#34977 = CARTESIAN_POINT ( 'NONE',  ( -26.23637979520668750, -290.8300022091412984, -344.0201461410976549 ) ) ;
#34978 = CARTESIAN_POINT ( 'NONE',  ( 202.7107630375198255, 295.9505694800565720, -54.00000000005820056 ) ) ;
#34979 = CARTESIAN_POINT ( 'NONE',  ( 22.83852374697876897, -288.7809803426674762, -311.8829848586217395 ) ) ;
#34980 = ORIENTED_EDGE ( 'NONE', *, *, #22274, .T. ) ;
#34981 = CARTESIAN_POINT ( 'NONE',  ( -5.032081409135720662, -279.5259625961167558, -200.7270117400689458 ) ) ;
#34982 = CARTESIAN_POINT ( 'NONE',  ( -99.84354733968551443, -297.7979727864587289, -225.5634407895096558 ) ) ;
#34983 = CARTESIAN_POINT ( 'NONE',  ( -108.3084050590193925, -289.0345037291086783, -243.6781269526779852 ) ) ;
#34984 = CARTESIAN_POINT ( 'NONE',  ( -113.9217547311807124, -296.7875359790674565, -278.1866868729893554 ) ) ;
#34985 = CARTESIAN_POINT ( 'NONE',  ( 29.87354671900513381, -293.5008940983319121, -241.6976179229490072 ) ) ;
#34986 = CARTESIAN_POINT ( 'NONE',  ( 175.2296996224750103, 250.5000000000000568, 0.000000000000000000 ) ) ;
#34987 =( LENGTH_UNIT ( ) NAMED_UNIT ( * ) SI_UNIT ( .MILLI., .METRE. ) );
#34988 = CARTESIAN_POINT ( 'NONE',  ( -12.43160647034326338, -290.2542039735134267, -342.5427356789984970 ) ) ;
#34989 = CARTESIAN_POINT ( 'NONE',  ( 40.64545035920995986, -283.8376638359844719, -252.5284128619064461 ) ) ;
#34990 = EDGE_CURVE ( 'NONE', #12630, #55975, #83589, .T. ) ;
#34991 = CARTESIAN_POINT ( 'NONE',  ( 39.31076506226148126, -280.8238365130334842, -264.2200784456269957 ) ) ;
#34992 = CARTESIAN_POINT ( 'NONE',  ( 15.23032876038422145, -284.3084113701843307, -323.6901844011642879 ) ) ;
#34993 = ADVANCED_FACE ( 'NONE', ( #46548 ), #75449, .T. ) ;
#34994 = CARTESIAN_POINT ( 'NONE',  ( 36.80945472854773470, -285.8943480812585562, -251.9162669860722303 ) ) ;
#34995 = CARTESIAN_POINT ( 'NONE',  ( -81.27673970728709207, -287.7340103903598560, -330.5170934129919829 ) ) ;
#34996 = CARTESIAN_POINT ( 'NONE',  ( 38.31928946176864770, -277.3507204399658121, -265.4951130508255801 ) ) ;
#34997 = VERTEX_POINT ( 'NONE', #32827 ) ;
#34999 = CARTESIAN_POINT ( 'NONE',  ( 33.86155837230335663, -280.6826821099535891, -253.8085155434326907 ) ) ;
#34998 = CARTESIAN_POINT ( 'NONE',  ( -102.1558831289512312, -279.0102546039531717, -236.6635809296179502 ) ) ;
#35000 = CARTESIAN_POINT ( 'NONE',  ( 28.83617688386293665, -277.1382940207387264, -309.1165189390781620 ) ) ;
#35001 = CARTESIAN_POINT ( 'NONE',  ( -69.78019392368931051, -278.4294387159051780, -200.9511783809121255 ) ) ;
#35002 = CARTESIAN_POINT ( 'NONE',  ( -84.79127711417702074, -218.1117258539772763, -350.1014080083962767 ) ) ;
#35003 = CARTESIAN_POINT ( 'NONE',  ( -114.1064060109667508, -273.4932526720010628, -270.3730758795568363 ) ) ;
#35004 = CARTESIAN_POINT ( 'NONE',  ( -36.56645602178579679, -299.4869440493469028, -193.9501587921773762 ) ) ;
#35005 = CARTESIAN_POINT ( 'NONE',  ( -69.85430415644619018, -291.9805209788416391, -337.9475929042657754 ) ) ;
#35006 = LINE ( 'NONE', #77637, #22699 ) ;
#35007 = AXIS2_PLACEMENT_3D ( 'NONE', #70971, #5641, #6578 ) ;
#35008 = CARTESIAN_POINT ( 'NONE',  ( 23.77476431663124146, -289.1914790262187012, -310.8686655463697548 ) ) ;
#35009 = CARTESIAN_POINT ( 'NONE',  ( -2.705076435574930827, -288.2638079838026215, -202.7131500892564588 ) ) ;
#35010 = CARTESIAN_POINT ( 'NONE',  ( 32.77008559830159840, -286.6267683397261976, -249.6232196799394956 ) ) ;
#35011 = CARTESIAN_POINT ( 'NONE',  ( -63.89666356167938943, -282.8970134293133469, -342.5716492105353836 ) ) ;
#35012 = CARTESIAN_POINT ( 'NONE',  ( -71.29175051220498460, -277.9960376746051338, -204.8195209370862528 ) ) ;
#35013 = CARTESIAN_POINT ( 'NONE',  ( 27.43379844523405353, -288.9235344496933635, -233.9930692874836211 ) ) ;
#35014 = CARTESIAN_POINT ( 'NONE',  ( 0.7749871145252934523, -279.0499621532649144, -207.2320315072333017 ) ) ;
#35015 = CARTESIAN_POINT ( 'NONE',  ( -95.65415360224463370, -279.2421997414294879, -315.0925526705166249 ) ) ;
#35016 = CARTESIAN_POINT ( 'NONE',  ( 21.52704858610170646, -275.4387243879731386, -227.0892002225640454 ) ) ;
#35017 = CARTESIAN_POINT ( 'NONE',  ( 35.56510900238991724, -286.6442381895781750, -293.8686891211037846 ) ) ;
#35018 = AXIS2_PLACEMENT_3D ( 'NONE', #12712, #6537, #65245 ) ;
#35019 = CARTESIAN_POINT ( 'NONE',  ( 9.119308708470402536, -283.2351032242546580, -331.5618816860834954 ) ) ;
#35020 = CARTESIAN_POINT ( 'NONE',  ( -88.27609999514243100, -284.2352236190148460, -328.0969160817451211 ) ) ;
#35021 = CARTESIAN_POINT ( 'NONE',  ( -21.38614744700854331, -283.0086018331040805, -341.6480968521278783 ) ) ;
#35022 = VERTEX_POINT ( 'NONE', #10567 ) ;
#35023 = ORIENTED_EDGE ( 'NONE', *, *, #33104, .T. ) ;
#35024 = DIRECTION ( 'NONE',  ( -0.000000000000000000, 1.000000000000000000, -0.000000000000000000 ) ) ;
#35025 = CARTESIAN_POINT ( 'NONE',  ( -15.28876965590376180, -290.6301743983809729, -342.9002802508434229 ) ) ;
#35026 = CARTESIAN_POINT ( 'NONE',  ( -66.80992407303810410, -290.3588327283977151, -199.7571375642989153 ) ) ;
#35027 = CARTESIAN_POINT ( 'NONE',  ( -47.28459635517239690, -297.1198846279776262, -197.8271035934619135 ) ) ;
#35028 = CARTESIAN_POINT ( 'NONE',  ( 39.34004276821458035, -292.8285587788984685, -264.5971703139227884 ) ) ;
#35029 = CARTESIAN_POINT ( 'NONE',  ( -29.11475894678043730, -287.4258740215034322, -343.5937964168320491 ) ) ;
#35030 = CARTESIAN_POINT ( 'NONE',  ( -11.89098930267787146, -290.6277527739537732, -200.8065911664070597 ) ) ;
#35031 = CARTESIAN_POINT ( 'NONE',  ( 32.69712346968345429, -289.0485376442100005, -292.4779092497420265 ) ) ;
#35032 = CARTESIAN_POINT ( 'NONE',  ( 10.59707575819634329, -289.1948066931273615, -210.1954327657594490 ) ) ;
#35033 = CARTESIAN_POINT ( 'NONE',  ( -110.6895420685528819, -292.7540674466096675, -254.6449255276718588 ) ) ;
#35034 = CARTESIAN_POINT ( 'NONE',  ( -105.5850139170171929, -288.9663577048036132, -238.7272238775061055 ) ) ;
#35035 = CARTESIAN_POINT ( 'NONE',  ( -110.7372182995887897, -292.7511992959705367, -254.8698763474712621 ) ) ;
#35036 = CARTESIAN_POINT ( 'NONE',  ( -70.09839522211105134, -286.5509159312609313, -204.8459266482407202 ) ) ;
#35037 = CARTESIAN_POINT ( 'NONE',  ( -22.57938188942921087, -294.2407228061202886, -196.6052906834899829 ) ) ;
#35038 = CARTESIAN_POINT ( 'NONE',  ( -187.9122233887894140, -89.54582641780471874, -21.50000000000000000 ) ) ;
#35039 = SPHERICAL_SURFACE ( 'NONE', #4982, 1.000000000000000000 ) ;
#35040 = CARTESIAN_POINT ( 'NONE',  ( 22.31491323200852506, -276.9039361497368077, -224.3021467622433249 ) ) ;
#35041 = CARTESIAN_POINT ( 'NONE',  ( -102.1415986314595443, -282.0475739677020783, -308.1231862601117655 ) ) ;
#35042 = CARTESIAN_POINT ( 'NONE',  ( -112.4404954440458226, -295.9538031667455016, -254.0415229095897587 ) ) ;
#35043 = CARTESIAN_POINT ( 'NONE',  ( 23.12142240598065968, -273.2041087588997357, -227.6521132108448171 ) ) ;
#35044 = CARTESIAN_POINT ( 'NONE',  ( -103.4231509686823927, -277.0904095311445872, -235.9772063905259358 ) ) ;
#35045 = CARTESIAN_POINT ( 'NONE',  ( -29.96513750278331401, -275.3526743908157641, -197.3356646905856167 ) ) ;
#35046 = CARTESIAN_POINT ( 'NONE',  ( -66.26817020021830729, -296.8637195194720562, -338.0267240711888803 ) ) ;
#35047 = DIRECTION ( 'NONE',  ( -1.000000000000000000, 0.000000000000000000, 0.000000000000000000 ) ) ;
#35048 = CARTESIAN_POINT ( 'NONE',  ( -96.23637586860564852, -297.9622066296504954, -226.9346773168308857 ) ) ;
#35050 = CARTESIAN_POINT ( 'NONE',  ( -81.06930966476510037, -273.2729221968295406, -211.8434672281357223 ) ) ;
#35049 = CARTESIAN_POINT ( 'NONE',  ( -15.85773043032068941, -284.3486647624100669, -198.0791666224836547 ) ) ;
#35051 = CARTESIAN_POINT ( 'NONE',  ( 27.13775883476131767, -286.9992249885727347, -228.2731224035461821 ) ) ;
#35052 = CARTESIAN_POINT ( 'NONE',  ( -54.50103321318048444, -288.9333890928223809, -345.4578141987332174 ) ) ;
#35053 = CARTESIAN_POINT ( 'NONE',  ( -94.32091129092921733, -297.8512790533748102, -319.6741618999815273 ) ) ;
#35054 = CARTESIAN_POINT ( 'NONE',  ( -6.020196105746181026, -292.6393662886162019, -338.3242831247117692 ) ) ;
#35055 = CARTESIAN_POINT ( 'NONE',  ( -39.57230616453448846, -279.2220148780185696, -193.5419540422863065 ) ) ;
#35056 = CARTESIAN_POINT ( 'NONE',  ( -106.6662871844225293, -293.6237833571632336, -303.7098442033569654 ) ) ;
#35057 = CARTESIAN_POINT ( 'NONE',  ( 153.7700350902760533, 129.6490463903464274, 11.80126012119838208 ) ) ;
#35058 = CARTESIAN_POINT ( 'NONE',  ( -45.42131696010972064, -287.9517222505797918, -343.3121309732811142 ) ) ;
#35059 = DIRECTION ( 'NONE',  ( -0.000000000000000000, -1.000000000000000000, -0.000000000000000000 ) ) ;
#35060 = CARTESIAN_POINT ( 'NONE',  ( -26.20232545359602128, -286.9103189074242550, -344.5817177250585246 ) ) ;
#35061 = CARTESIAN_POINT ( 'NONE',  ( -102.6538186299615063, -274.5337074681983722, -236.1179301645551618 ) ) ;
#35062 = CARTESIAN_POINT ( 'NONE',  ( -61.87575396307633468, -281.1647866547999683, -197.9403574164294639 ) ) ;
#35064 = CARTESIAN_POINT ( 'NONE',  ( 26.85504930592198747, -282.0263341306159077, -305.1142093861718081 ) ) ;
#35063 = CARTESIAN_POINT ( 'NONE',  ( -105.6854468564162772, -294.1571668150403411, -302.1028741232273660 ) ) ;
#35065 = CARTESIAN_POINT ( 'NONE',  ( -98.27315770537690298, -296.0904225430992938, -317.4393240023110820 ) ) ;
#35066 = CARTESIAN_POINT ( 'NONE',  ( -104.9280105224108723, -274.3670090560657968, -241.1206460327117327 ) ) ;
#35067 = CARTESIAN_POINT ( 'NONE',  ( 9.552133459559023265, -282.6968129675674390, -211.7627926796758402 ) ) ;
#35068 = CARTESIAN_POINT ( 'NONE',  ( -97.38312987122002085, -295.0280845433547370, -312.2948175903156880 ) ) ;
#35069 = VECTOR ( 'NONE', #27820, 1000.000000000000000 ) ;
#35070 = ORIENTED_EDGE ( 'NONE', *, *, #12828, .T. ) ;
#35071 = DIRECTION ( 'NONE',  ( 0.000000000000000000, 1.000000000000000000, -0.000000000000000000 ) ) ;
#35073 = CARTESIAN_POINT ( 'NONE',  ( -72.15412193862135837, -285.4949136495443440, -336.3909755689485905 ) ) ;
#35072 = AXIS2_PLACEMENT_3D ( 'NONE', #52610, #73936, #23747 ) ;
#35074 = CARTESIAN_POINT ( 'NONE',  ( 2.197429475817664013, -229.5268262511776527, 25.50000000000000000 ) ) ;
#35075 = CARTESIAN_POINT ( 'NONE',  ( 21.27581636871891391, -291.6952119285919025, -317.1477375740089997 ) ) ;
#35076 = CARTESIAN_POINT ( 'NONE',  ( 25.92809382574244381, -275.3272183865963711, -314.0547070106519527 ) ) ;
#35077 = CARTESIAN_POINT ( 'NONE',  ( 26.23559892921718273, -292.8931972852217882, -234.3841342450033665 ) ) ;
#35078 = AXIS2_PLACEMENT_3D ( 'NONE', #27371, #20736, #56261 ) ;
#35079 = CARTESIAN_POINT ( 'NONE',  ( 29.95544662441509942, -283.4743252330021619, -300.5165012843273189 ) ) ;
#35080 = CARTESIAN_POINT ( 'NONE',  ( -3.482472231383599404, -278.1974927048348150, -335.9354506382227328 ) ) ;
#35081 = CARTESIAN_POINT ( 'NONE',  ( -41.51863522020822472, -284.5289162565445622, -346.7095682255419433 ) ) ;
#35082 = CARTESIAN_POINT ( 'NONE',  ( 1.297366187555715200, -281.3188258148346108, -332.8236077957297994 ) ) ;
#35083 = CARTESIAN_POINT ( 'NONE',  ( -82.51219249051763427, -281.4358380443744068, -210.4241328578222578 ) ) ;
#35084 = CARTESIAN_POINT ( 'NONE',  ( -33.33448420970651682, -298.1010253735603328, -193.3611178742239929 ) ) ;
#35085 = CARTESIAN_POINT ( 'NONE',  ( -3.996769887463077708, -276.4578096550213786, -339.7810603579957274 ) ) ;
#35086 = CARTESIAN_POINT ( 'NONE',  ( 35.62320029464395787, -295.2815483374096175, -255.6153556392803523 ) ) ;
#35087 = DIRECTION ( 'NONE',  ( 0.000000000000000000, 0.000000000000000000, -1.000000000000000000 ) ) ;
#35088 = LINE ( 'NONE', #78655, #31503 ) ;
#35089 = CARTESIAN_POINT ( 'NONE',  ( -65.17218556482481517, -293.5515436169272903, -340.8433304976075533 ) ) ;
#35090 = CARTESIAN_POINT ( 'NONE',  ( 13.76990258603644435, -275.8198561066093362, -322.6387783478787128 ) ) ;
#35091 = CARTESIAN_POINT ( 'NONE',  ( 17.08075998302576082, -295.8138976143769128, -323.9237076688007733 ) ) ;
#35092 = CARTESIAN_POINT ( 'NONE',  ( 10.95989748297938249, -295.6061837355654234, -329.8850521119557584 ) ) ;
#35093 = ADVANCED_FACE ( 'NONE', ( #39432 ), #55472, .T. ) ;
#35094 = CARTESIAN_POINT ( 'NONE',  ( 29.88565193514773100, -289.9866415613514619, -303.2322536174998504 ) ) ;
#35095 = CARTESIAN_POINT ( 'NONE',  ( -59.76808878727397456, -275.3431944365568711, -341.7549938832565886 ) ) ;
#35096 = CARTESIAN_POINT ( 'NONE',  ( -57.52671180489815583, -281.7097081190568133, -198.7100223950835414 ) ) ;
#35097 = CARTESIAN_POINT ( 'NONE',  ( -66.64201862571009372, -293.5188337672774423, -338.7921455630880700 ) ) ;
#35098 = CARTESIAN_POINT ( 'NONE',  ( 26.79292985761020418, -282.8746400808794306, -229.9260790366863603 ) ) ;
#35099 = CARTESIAN_POINT ( 'NONE',  ( -22.38338496074521444, -285.1683966839905793, -198.5422064699684199 ) ) ;
#35100 = CARTESIAN_POINT ( 'NONE',  ( -81.88695342447972791, -220.3879184236133995, -351.6809530069663765 ) ) ;
#35101 = EDGE_LOOP ( 'NONE', ( #31038, #63576, #8335, #18175 ) ) ;
#35102 = CARTESIAN_POINT ( 'NONE',  ( -110.0150175914611879, -284.3193273053618100, -262.7436277951209718 ) ) ;
#35103 = ORIENTED_EDGE ( 'NONE', *, *, #46621, .T. ) ;
#35104 = CARTESIAN_POINT ( 'NONE',  ( 24.86464926190132729, -283.2291745764003963, -315.2372064562601395 ) ) ;
#35105 = CARTESIAN_POINT ( 'NONE',  ( -78.29714740122767580, -284.3090852276297937, -205.6258103314299603 ) ) ;
#35106 = CARTESIAN_POINT ( 'NONE',  ( -73.66491904115208911, -280.5233534871238135, -202.7189689908636296 ) ) ;
#35107 = CARTESIAN_POINT ( 'NONE',  ( -59.44551037914906289, -278.8534163515661817, -343.3962418862936374 ) ) ;
#35108 = CARTESIAN_POINT ( 'NONE',  ( -92.05005921254146983, -298.4090924074129703, -314.0302885647153062 ) ) ;
#35109 = CARTESIAN_POINT ( 'NONE',  ( -77.03173369861616493, -209.0939622114285896, -357.2395138152388654 ) ) ;
#35110 = CARTESIAN_POINT ( 'NONE',  ( 1.543904745177172577, -276.5734098270466461, -206.4241321320548934 ) ) ;
#35111 = CARTESIAN_POINT ( 'NONE',  ( -78.32199257516948876, -208.3160289898351039, -357.0357957823813990 ) ) ;
#35112 = CARTESIAN_POINT ( 'NONE',  ( -92.49551339617238455, -277.2776776924193882, -220.0629700480870383 ) ) ;
#35113 = CARTESIAN_POINT ( 'NONE',  ( -64.05385495817891695, -293.4687306080232361, -199.1689434712971547 ) ) ;
#35114 = CARTESIAN_POINT ( 'NONE',  ( 16.22819808353040472, -293.6146896561054405, -320.1020334733168511 ) ) ;
#35115 = CARTESIAN_POINT ( 'NONE',  ( -70.61813494197815544, -288.9868327067813425, -339.7456567375499503 ) ) ;
#35116 = LINE ( 'NONE', #91928, #8251 ) ;
#35118 = CARTESIAN_POINT ( 'NONE',  ( -10.43956925982369022, -284.8089592220474628, -201.6254240591889868 ) ) ;
#35117 = CARTESIAN_POINT ( 'NONE',  ( -44.75665195231122340, -293.7188518064703544, -346.4642630769265566 ) ) ;
#35119 = CARTESIAN_POINT ( 'NONE',  ( -34.83897387912438859, -293.9443433434321946, -196.1681139736239743 ) ) ;
#35120 = CARTESIAN_POINT ( 'NONE',  ( -32.09388494005224146, -284.2997450642483841, -343.6666697104413402 ) ) ;
#35121 = ORIENTED_EDGE ( 'NONE', *, *, #44275, .F. ) ;
#35122 = CARTESIAN_POINT ( 'NONE',  ( -40.63436127924891395, -292.9529698175599606, -193.6539177215897212 ) ) ;
#35123 = CARTESIAN_POINT ( 'NONE',  ( -2.393716854173553177, -283.0688945432116839, -334.5363652291671315 ) ) ;
#35124 = CARTESIAN_POINT ( 'NONE',  ( 25.38066613028506779, -292.9318826505336801, -314.3602872926184659 ) ) ;
#35125 = CARTESIAN_POINT ( 'NONE',  ( 34.92410261474422839, -288.6871812556929626, -296.6275207227560031 ) ) ;
#35126 = CARTESIAN_POINT ( 'NONE',  ( -46.01260315750639762, -289.6515226236320473, -346.8625005907836112 ) ) ;
#35127 = CARTESIAN_POINT ( 'NONE',  ( 27.65717319731061252, -287.2660356853135113, -237.0209720823233113 ) ) ;
#35128 = EDGE_LOOP ( 'NONE', ( #52939, #84957, #51732, #30467, #80366 ) ) ;
#35129 = CARTESIAN_POINT ( 'NONE',  ( 196.0143093133015384, 24.42324672360810212, 11.99999999999998757 ) ) ;
#35130 = CARTESIAN_POINT ( 'NONE',  ( -112.8911560229499713, -298.4934431435319766, -263.9981615028202100 ) ) ;
#35131 = CARTESIAN_POINT ( 'NONE',  ( -46.05696478967565355, -296.6286373044244442, -194.3522866930171062 ) ) ;
#35132 = CARTESIAN_POINT ( 'NONE',  ( -93.79504581237952721, -276.9514881447387324, -317.0329754559917319 ) ) ;
#35133 = CARTESIAN_POINT ( 'NONE',  ( -34.09950839995164529, -273.5995606539274263, -193.4909996258856495 ) ) ;
#35134 = CARTESIAN_POINT ( 'NONE',  ( -31.56715743719263401, -293.4579460093494276, -343.8784509056085312 ) ) ;
#35135 = CARTESIAN_POINT ( 'NONE',  ( 34.48726678029306925, -277.0799869147350023, -252.5124897734706906 ) ) ;
#35136 = CARTESIAN_POINT ( 'NONE',  ( -44.64710468268618371, -296.1984390029592760, -196.6581185529536810 ) ) ;
#35137 = CARTESIAN_POINT ( 'NONE',  ( -36.97825240356964827, -296.2525467787077105, -343.7697843894578682 ) ) ;
#35138 = CARTESIAN_POINT ( 'NONE',  ( -9.099141060038419937, -295.7536331495725790, -338.0252367568480167 ) ) ;
#35139 = CARTESIAN_POINT ( 'NONE',  ( -47.80257052418233599, -229.5268262511776527, 25.50000000000000000 ) ) ;
#35140 = CARTESIAN_POINT ( 'NONE',  ( -100.9491180487112985, -297.5936488349601063, -312.4152583790274207 ) ) ;
#35141 = AXIS2_PLACEMENT_3D ( 'NONE', #46792, #75694, #3738 ) ;
#35142 = CARTESIAN_POINT ( 'NONE',  ( -111.4021019463929321, -294.3836093643077447, -283.5043596144729463 ) ) ;
#35143 = CARTESIAN_POINT ( 'NONE',  ( 19.28711480348925278, -299.3951234332541844, -193.4569588003669480 ) ) ;
#35144 = CARTESIAN_POINT ( 'NONE',  ( -85.08096386428900360, -288.3006753530420951, -326.4314056935131134 ) ) ;
#35145 = CARTESIAN_POINT ( 'NONE',  ( -99.51505065204536038, -275.1208352737113501, -228.3223241137231128 ) ) ;
#35146 = CARTESIAN_POINT ( 'NONE',  ( -90.12520477952683962, -273.8225208782365598, -214.3113218752585567 ) ) ;
#35148 = CARTESIAN_POINT ( 'NONE',  ( -110.0717798650315871, -296.9785320766644645, -263.3018313253784299 ) ) ;
#35147 = AXIS2_PLACEMENT_3D ( 'NONE', #15478, #44349, #73259 ) ;
#35149 = CIRCLE ( 'NONE', #6375, 7.999911143031724237 ) ;
#35150 = CARTESIAN_POINT ( 'NONE',  ( -12.08491086282274374, -282.3589573431759163, -199.3098510257975136 ) ) ;
#35151 = CARTESIAN_POINT ( 'NONE',  ( 37.93730943332821681, -280.4097316369652049, -284.0855016050799122 ) ) ;
#35152 = VERTEX_POINT ( 'NONE', #6289 ) ;
#35153 = CARTESIAN_POINT ( 'NONE',  ( -86.04422592025551353, -283.0557899326468601, -329.8705858656843475 ) ) ;
#35154 = CARTESIAN_POINT ( 'NONE',  ( 20.73780776296399253, -275.5829070763356867, -320.7802861776054328 ) ) ;
#35155 = CARTESIAN_POINT ( 'NONE',  ( 5.748816988850379950, -279.0254450419402019, -207.5148949581167130 ) ) ;
#35156 = CARTESIAN_POINT ( 'NONE',  ( -56.07453365475736717, -277.8114028518803025, -197.5124507396807303 ) ) ;
#35157 = CARTESIAN_POINT ( 'NONE',  ( -32.63536286361777883, -272.6873203851653216, -196.9099087985494805 ) ) ;
#35158 = CARTESIAN_POINT ( 'NONE',  ( -28.04941198657036239, -276.1701406127610881, -195.8876971949641472 ) ) ;
#35159 = DIRECTION ( 'NONE',  ( -0.000000000000000000, -0.000000000000000000, 1.000000000000000000 ) ) ;
#35160 = CARTESIAN_POINT ( 'NONE',  ( -102.9632401559879327, -295.2983825482343718, -231.9457594866861143 ) ) ;
#35161 = CARTESIAN_POINT ( 'NONE',  ( -36.37361661899084453, -290.0843460592308247, -194.9993779147926318 ) ) ;
#35162 = CARTESIAN_POINT ( 'NONE',  ( -50.56635501534110233, -291.8877222276124144, -194.5052777122625685 ) ) ;
#35163 = CARTESIAN_POINT ( 'NONE',  ( 11.53235252346953921, -278.3760872149321699, -327.4693958504727789 ) ) ;
#35164 = CARTESIAN_POINT ( 'NONE',  ( -18.75191855850065537, -272.2912262481341372, -197.6476279402562568 ) ) ;
#35165 = CARTESIAN_POINT ( 'NONE',  ( -83.63170945779077670, -373.0521521680024648, -417.1172536214571096 ) ) ;
#35166 = CARTESIAN_POINT ( 'NONE',  ( -63.39217505487197712, -285.3091256307062622, -341.2884537110950305 ) ) ;
#35167 = CYLINDRICAL_SURFACE ( 'NONE', #47135, 20.00000000000000000 ) ;
#35168 = CARTESIAN_POINT ( 'NONE',  ( -41.47493295815851155, -283.9999627594650633, -195.4624494402378616 ) ) ;
#35169 = DIRECTION ( 'NONE',  ( 0.000000000000000000, 0.000000000000000000, 1.000000000000000000 ) ) ;
#35170 = CARTESIAN_POINT ( 'NONE',  ( -4.170862989313587121, -293.3996702235468206, -335.8490490180525399 ) ) ;
#35171 = CARTESIAN_POINT ( 'NONE',  ( -1.570734421161609218, -284.6708018781619671, -205.2549634704404014 ) ) ;
#35172 = CARTESIAN_POINT ( 'NONE',  ( 175.2296996224750103, 21.00000000000000000, 15.00000000000000000 ) ) ;
#35173 = CARTESIAN_POINT ( 'NONE',  ( -59.00974585222409274, -293.3323655896919036, -342.1629037603699430 ) ) ;
#35174 = CARTESIAN_POINT ( 'NONE',  ( -112.4579771270189639, -282.8589345309415535, -284.0774599851088169 ) ) ;
#35175 = CARTESIAN_POINT ( 'NONE',  ( -19.35913294916303684, -281.8873589836982774, -198.7326508194230712 ) ) ;
#35176 = CARTESIAN_POINT ( 'NONE',  ( -54.88863481883083040, -287.0364732816289006, -195.7949473659950002 ) ) ;
#35177 = CARTESIAN_POINT ( 'NONE',  ( 20.81974377915599206, -280.4592680848270447, -319.2612249246336091 ) ) ;
#35178 = CARTESIAN_POINT ( 'NONE',  ( 33.71031196159538013, -287.3304598633699811, -253.5556297796739500 ) ) ;
#35179 = CARTESIAN_POINT ( 'NONE',  ( -89.49067187255319311, -279.2296081869910154, -322.3551283074796743 ) ) ;
#35180 = CARTESIAN_POINT ( 'NONE',  ( -107.7765413463411193, -279.6165134930624845, -250.5274217184221186 ) ) ;
#35181 = CARTESIAN_POINT ( 'NONE',  ( -98.03480622130315680, -287.1393108790977067, -225.6125606721149666 ) ) ;
#35182 = ORIENTED_EDGE ( 'NONE', *, *, #999, .F. ) ;
#35183 = CARTESIAN_POINT ( 'NONE',  ( -103.8487329771342900, -296.8915871200160836, -231.4512189537137772 ) ) ;
#35184 = CARTESIAN_POINT ( 'NONE',  ( 37.27532521466388715, -289.5765603476536398, -273.8112632980647163 ) ) ;
#35185 = FACE_OUTER_BOUND ( 'NONE', #4716, .T. ) ;
#35186 = CARTESIAN_POINT ( 'NONE',  ( -72.08107566293803359, -276.1233781216987495, -198.2974183793908196 ) ) ;
#35187 = ORIENTED_EDGE ( 'NONE', *, *, #7720, .T. ) ;
#35188 = CARTESIAN_POINT ( 'NONE',  ( 8.414981144280172742, -272.6768079114083321, -210.7259392502402022 ) ) ;
#35189 = CARTESIAN_POINT ( 'NONE',  ( 38.43919010718616391, -292.0590079796406826, -278.8264501444517123 ) ) ;
#35190 = CARTESIAN_POINT ( 'NONE',  ( -90.08595122003215749, -296.7894884770489057, -219.7315038131477820 ) ) ;
#35191 = CARTESIAN_POINT ( 'NONE',  ( 34.38066818839624261, -288.8503355149758249, -253.3770917654753418 ) ) ;
#35192 = CARTESIAN_POINT ( 'NONE',  ( 17.80305468640262845, -282.6156393282927866, -220.9948336274530902 ) ) ;
#35193 = CARTESIAN_POINT ( 'NONE',  ( -70.36783672594074801, -290.9041416471278012, -339.2803579258600735 ) ) ;
#35194 = CARTESIAN_POINT ( 'NONE',  ( -111.7789606448097146, -291.6441437160613077, -288.0917515122961845 ) ) ;
#35195 = CARTESIAN_POINT ( 'NONE',  ( -107.0640408638667509, -286.1908228931040981, -298.1392233310317010 ) ) ;
#35196 = CARTESIAN_POINT ( 'NONE',  ( -113.0652416208005633, -278.5433079883870278, -284.3958294107782194 ) ) ;
#35197 = ORIENTED_EDGE ( 'NONE', *, *, #584, .F. ) ;
#35198 = CARTESIAN_POINT ( 'NONE',  ( -0.1892511644907210466, -292.6418881540054144, -336.1712218482339267 ) ) ;
#35199 = CARTESIAN_POINT ( 'NONE',  ( 38.42518934517773488, -281.5580400392859133, -284.1594466030773560 ) ) ;
#35200 = CARTESIAN_POINT ( 'NONE',  ( -51.82526126042856163, -275.7254368878644755, -197.4998507447658653 ) ) ;
#35201 = ADVANCED_FACE ( 'NONE', ( #18618 ), #12946, .F. ) ;
#35202 = CARTESIAN_POINT ( 'NONE',  ( -6.998514795304313196, -282.9805209788415823, -207.2794874003663779 ) ) ;
#35203 = CARTESIAN_POINT ( 'NONE',  ( -4.453982600200022013, -274.8646064966455924, -338.8763144015833859 ) ) ;
#35205 = AXIS2_PLACEMENT_3D ( 'NONE', #60773, #15825, #80669 ) ;
#35204 = CARTESIAN_POINT ( 'NONE',  ( 204.6539576904058606, 293.9636489450775230, 0.000000000000000000 ) ) ;
#35206 = CARTESIAN_POINT ( 'NONE',  ( 26.90618844118116826, -281.5340661876780928, -305.1490074827225385 ) ) ;
#35207 = CIRCLE ( 'NONE', #24582, 2.842139515347646750 ) ;
#35208 = CARTESIAN_POINT ( 'NONE',  ( -88.93330921929572241, -278.9633320578240614, -326.9854465793111444 ) ) ;
#35209 = CARTESIAN_POINT ( 'NONE',  ( -91.49718789812359887, -274.5757289615240211, -220.6592207342119423 ) ) ;
#35210 = CARTESIAN_POINT ( 'NONE',  ( -52.11622030124287619, -284.9263514514747158, -194.9773944654879756 ) ) ;
#35211 = CARTESIAN_POINT ( 'NONE',  ( -94.87807847671112427, -291.6627561658496575, -316.9179561813990631 ) ) ;
#35212 = CARTESIAN_POINT ( 'NONE',  ( -110.2774149309257723, -274.4342014711707520, -248.1165464941674088 ) ) ;
#35213 = AXIS2_PLACEMENT_3D ( 'NONE', #68717, #33185, #10460 ) ;
#35214 = CARTESIAN_POINT ( 'NONE',  ( -15.93152513608725052, -275.6384655142044835, -196.8561362936036687 ) ) ;
#35215 = DIRECTION ( 'NONE',  ( -0.000000000000000000, -0.000000000000000000, 1.000000000000000000 ) ) ;
#35216 = CARTESIAN_POINT ( 'NONE',  ( -100.2612980934016917, -298.0042605506891960, -310.9671402915281533 ) ) ;
#35217 = CARTESIAN_POINT ( 'NONE',  ( -107.9109168409701596, -282.2269498383935797, -295.4156600920512119 ) ) ;
#35218 = AXIS2_PLACEMENT_3D ( 'NONE', #40261, #83356, #63038 ) ;
#35219 = CARTESIAN_POINT ( 'NONE',  ( -113.7930766539588348, -290.1008250370772430, -279.7974675758250100 ) ) ;
#35220 = CARTESIAN_POINT ( 'NONE',  ( 35.73669741397215205, -273.3752093012220712, -255.0869582807416407 ) ) ;
#35221 = CARTESIAN_POINT ( 'NONE',  ( -2.605959168264249559, -288.1038210257819401, -202.5241882912712867 ) ) ;
#35222 = CARTESIAN_POINT ( 'NONE',  ( -105.4051403116671679, -289.1079206582259644, -297.7296520166478331 ) ) ;
#35223 = ORIENTED_EDGE ( 'NONE', *, *, #42272, .T. ) ;
#35224 = CARTESIAN_POINT ( 'NONE',  ( -94.26017601693298786, -289.8237752516374144, -219.3817751469406971 ) ) ;
#35225 = CARTESIAN_POINT ( 'NONE',  ( -99.72747028583918905, -290.7413698035805965, -232.4124267198380949 ) ) ;
#35226 = ORIENTED_EDGE ( 'NONE', *, *, #21048, .F. ) ;
#35227 = CARTESIAN_POINT ( 'NONE',  ( 39.33071437110933033, -288.6106856601679169, -268.6778581246182398 ) ) ;
#35228 = CARTESIAN_POINT ( 'NONE',  ( -87.10684196784009714, -278.1020191509133497, -323.7981664075922481 ) ) ;
#35229 = ADVANCED_FACE ( 'NONE', ( #4408 ), #70236, .T. ) ;
#35230 = CARTESIAN_POINT ( 'NONE',  ( 15.25665350483664540, -293.2502009538767425, -326.1724582659211364 ) ) ;
#35231 = CARTESIAN_POINT ( 'NONE',  ( -24.54236882900957539, -283.5444587441600675, -346.2405541171568188 ) ) ;
#35232 = CARTESIAN_POINT ( 'NONE',  ( -60.50760296608934397, -286.0931184365711033, -196.8951669331631251 ) ) ;
#35233 = CARTESIAN_POINT ( 'NONE',  ( -29.43814751788083584, -283.2827070557685261, -343.0037939215443998 ) ) ;
#35234 = CARTESIAN_POINT ( 'NONE',  ( -78.06300626195221071, -208.5067154030725476, -357.1885865629087107 ) ) ;
#35235 = CARTESIAN_POINT ( 'NONE',  ( -40.80092957519016039, -139.0259249319638002, -363.6696181199743023 ) ) ;
#35236 = CARTESIAN_POINT ( 'NONE',  ( 159.7936134115024345, 218.3991897550104966, -202.4342046892747078 ) ) ;
#35237 = CARTESIAN_POINT ( 'NONE',  ( -110.5031764828875396, -271.7494487804054302, -270.3509199023655469 ) ) ;
#35238 = CARTESIAN_POINT ( 'NONE',  ( -35.36828291736804175, -272.9977917035798782, -197.0660128374298665 ) ) ;
#35239 = CARTESIAN_POINT ( 'NONE',  ( -34.86291060757183402, -294.5294485291665296, -347.2596388131365757 ) ) ;
#35240 = CARTESIAN_POINT ( 'NONE',  ( 161.7159580759288815, 217.5486918941278418, -202.6611147385943354 ) ) ;
#35241 = CARTESIAN_POINT ( 'NONE',  ( -27.04619406426520811, -272.8651210279446104, -194.4970748072591107 ) ) ;
#35242 = CARTESIAN_POINT ( 'NONE',  ( -110.0905285846461226, -298.2200096415716644, -285.2051726285597510 ) ) ;
#35243 = CARTESIAN_POINT ( 'NONE',  ( -37.56463551181180094, -293.1290060949550025, -197.0398476178612555 ) ) ;
#35244 = ORIENTED_EDGE ( 'NONE', *, *, #75328, .T. ) ;
#35245 = AXIS2_PLACEMENT_3D ( 'NONE', #71691, #31262, #9453 ) ;
#35246 = CARTESIAN_POINT ( 'NONE',  ( -100.5637074175163832, -298.0702343856254402, -226.7972501618737624 ) ) ;
#35247 = CARTESIAN_POINT ( 'NONE',  ( 22.01534606782081127, -288.6395021693905392, -312.9607601015925979 ) ) ;
#35248 = AXIS2_PLACEMENT_3D ( 'NONE', #15745, #1992, #37496 ) ;
#35249 = CARTESIAN_POINT ( 'NONE',  ( 39.44588811497572323, -294.3900413975638912, -273.1584581180337068 ) ) ;
#35250 = CARTESIAN_POINT ( 'NONE',  ( -39.10014349113041732, -295.5660103188100720, -347.2794823723841660 ) ) ;
#35251 = CARTESIAN_POINT ( 'NONE',  ( 34.90743487784244792, -293.5810685688406352, -259.9178189155641121 ) ) ;
#35252 = ORIENTED_EDGE ( 'NONE', *, *, #90641, .T. ) ;
#35253 = CARTESIAN_POINT ( 'NONE',  ( 35.88356750541262841, -277.2346337947118968, -251.7231357639323903 ) ) ;
#35254 = ORIENTED_EDGE ( 'NONE', *, *, #53031, .F. ) ;
#35255 = CARTESIAN_POINT ( 'NONE',  ( -113.7059633698434880, -277.9370919454821660, -280.1654332635939113 ) ) ;
#35256 = CARTESIAN_POINT ( 'NONE',  ( 35.87790370661325312, -276.4734764132098235, -268.8451820742031941 ) ) ;
#35257 = CARTESIAN_POINT ( 'NONE',  ( -36.96753129560219975, -275.8169428051940599, -194.3624893066706534 ) ) ;
#35258 = CARTESIAN_POINT ( 'NONE',  ( 36.56417227919467194, -273.7602237509616430, -285.0692391952514413 ) ) ;
#35259 = CARTESIAN_POINT ( 'NONE',  ( -110.3145313817427109, -297.2607761888939990, -266.0184728521508646 ) ) ;
#35260 = CARTESIAN_POINT ( 'NONE',  ( -109.0471243335262415, -295.3433759139555832, -253.8170236080210032 ) ) ;
#35261 = PLANE ( 'NONE',  #68392 ) ;
#35262 = CARTESIAN_POINT ( 'NONE',  ( -93.03354370565018883, -279.7715123087858160, -217.2006664199690249 ) ) ;
#35263 = CARTESIAN_POINT ( 'NONE',  ( -16.37883840391437573, -276.9403619103208598, -340.3395050251974112 ) ) ;
#35264 = CARTESIAN_POINT ( 'NONE',  ( 39.14738155672085185, -286.2162256951568793, -268.7122837099698813 ) ) ;
#35265 = CARTESIAN_POINT ( 'NONE',  ( -111.8779441903994751, -274.6592404277505466, -262.0335151623966681 ) ) ;
#35266 = CARTESIAN_POINT ( 'NONE',  ( 153.6539576904058038, 130.0000000000000568, 12.50000000000000000 ) ) ;
#35267 = AXIS2_PLACEMENT_3D ( 'NONE', #73818, #24544, #46312 ) ;
#35268 = CARTESIAN_POINT ( 'NONE',  ( 34.15598294770959598, -286.5451143551745190, -254.8471551645389752 ) ) ;
#35269 = CARTESIAN_POINT ( 'NONE',  ( -65.17671216468951911, -277.9231930766616756, -201.7813387523666790 ) ) ;
#35270 = CARTESIAN_POINT ( 'NONE',  ( -101.3151644604992896, -277.6210199222451251, -233.9912021565911289 ) ) ;
#35271 = CARTESIAN_POINT ( 'NONE',  ( -98.74513084906185156, -287.1372543737727483, -227.2736937462622393 ) ) ;
#35272 = CARTESIAN_POINT ( 'NONE',  ( -51.34167688163601895, -278.4402474850571139, -342.4106228704139312 ) ) ;
#35273 = DIRECTION ( 'NONE',  ( 0.000000000000000000, -0.9681751575201842375, -0.2502735790305606889 ) ) ;
#35274 = AXIS2_PLACEMENT_3D ( 'NONE', #39431, #11034, #31893 ) ;
#35275 = CARTESIAN_POINT ( 'NONE',  ( -62.09732662507806822, -275.6094125554237735, -342.2577171105186267 ) ) ;
#35276 = CIRCLE ( 'NONE', #70097, 24.00000000000001421 ) ;
#35277 = CARTESIAN_POINT ( 'NONE',  ( -2.872912963869989955, -275.1719479777118522, -205.8956591705210144 ) ) ;
#35278 = CARTESIAN_POINT ( 'NONE',  ( 16.53053704046080696, -284.2891632778894859, -322.8550797438385302 ) ) ;
#35279 = CARTESIAN_POINT ( 'NONE',  ( 156.4851178187871312, 0.000000000000000000, -7.000000000000000888 ) ) ;
#35280 = CARTESIAN_POINT ( 'NONE',  ( 17.61458404037442804, -290.1939152879416497, -322.2178535949965976 ) ) ;
#35281 = AXIS2_PLACEMENT_3D ( 'NONE', #27156, #48927, #38643 ) ;
#35282 = CARTESIAN_POINT ( 'NONE',  ( -45.46885936090239966, -289.9491379481171407, -195.7516741655833812 ) ) ;
#35283 = CARTESIAN_POINT ( 'NONE',  ( 175.2296996224750103, 20.99999999999998934, 0.000000000000000000 ) ) ;
#35284 = CARTESIAN_POINT ( 'NONE',  ( -1.467369808913267848, -273.2232015027394141, -206.2040847470133542 ) ) ;
#35285 = CARTESIAN_POINT ( 'NONE',  ( 13.77048810584812877, -290.9175361705032969, -216.5242375703555240 ) ) ;
#35286 = CARTESIAN_POINT ( 'NONE',  ( 198.7213489544213303, 274.9184959104715631, -125.0903475807052416 ) ) ;
#35287 = CARTESIAN_POINT ( 'NONE',  ( 199.1087447750284980, 64.61450673763175701, -10.46317447812566570 ) ) ;
#35288 = CARTESIAN_POINT ( 'NONE',  ( -31.89576399111479432, -287.4646290104125796, -346.5252862749107976 ) ) ;
#35289 = CARTESIAN_POINT ( 'NONE',  ( -78.80950385535176395, -285.2215242630711032, -331.4091455325706193 ) ) ;
#35290 = CARTESIAN_POINT ( 'NONE',  ( 2.232645568271720560, -284.8144243973138714, -205.4932123914291537 ) ) ;
#35291 = VECTOR ( 'NONE', #24195, 1000.000000000000000 ) ;
#35292 = CARTESIAN_POINT ( 'NONE',  ( -85.23159774975364655, -285.1543755263406865, -326.2353752154668882 ) ) ;
#35293 = CARTESIAN_POINT ( 'NONE',  ( -40.23052178807429158, -283.8922255226194693, -343.4655394408608231 ) ) ;
#35294 = CARTESIAN_POINT ( 'NONE',  ( -111.7322060136481667, -292.3784462725532194, -282.3802459801327700 ) ) ;
#35295 = CARTESIAN_POINT ( 'NONE',  ( 7.368925629068237448, -274.5281663898666125, -331.3379027065130913 ) ) ;
#35296 = CARTESIAN_POINT ( 'NONE',  ( 25.30722190772271318, -275.2924921395457432, -225.6076313383064189 ) ) ;
#35297 = AXIS2_PLACEMENT_3D ( 'NONE', #5120, #47716, #33051 ) ;
#35298 = CARTESIAN_POINT ( 'NONE',  ( -101.0995803351279676, -288.0892729156792029, -311.0067632723485644 ) ) ;
#35299 = CARTESIAN_POINT ( 'NONE',  ( -25.76996866147937126, -276.9086265280614043, -346.4866395299678743 ) ) ;
#35300 = CARTESIAN_POINT ( 'NONE',  ( -23.18267267301051149, -296.8502258103880536, -343.7035100873140436 ) ) ;
#35301 = DIRECTION ( 'NONE',  ( 0.000000000000000000, 1.000000000000000000, 0.000000000000000000 ) ) ;
#35302 = CARTESIAN_POINT ( 'NONE',  ( 209.2540529155442073, 37.08890681920322407, 12.07129462079485904 ) ) ;
#35303 = CARTESIAN_POINT ( 'NONE',  ( -91.11362499387101366, -282.5214086041353880, -320.4592574139649059 ) ) ;
#35304 = CARTESIAN_POINT ( 'NONE',  ( -28.43652130149055779, -278.1648302356249474, -195.8394381513753046 ) ) ;
#35305 = DIRECTION ( 'NONE',  ( 0.000000000000000000, 0.000000000000000000, -1.000000000000000000 ) ) ;
#35306 = CARTESIAN_POINT ( 'NONE',  ( -103.6176530311758768, -271.5289067674997909, -232.4370613619283006 ) ) ;
#35307 = CARTESIAN_POINT ( 'NONE',  ( -106.3631949085399526, -277.5790271343043969, -294.5963379074660224 ) ) ;
#35308 = CARTESIAN_POINT ( 'NONE',  ( 16.68044971575040947, -295.7858743692547705, -320.4841174841319003 ) ) ;
#35309 = AXIS2_PLACEMENT_3D ( 'NONE', #86652, #72927, #22270 ) ;
#35310 = CARTESIAN_POINT ( 'NONE',  ( 17.01377030590352746, -279.7248184309614771, -216.1851107612656335 ) ) ;
#35311 = CARTESIAN_POINT ( 'NONE',  ( 31.76606354608881588, -294.8166633918522734, -294.7519593685512973 ) ) ;
#35312 = CARTESIAN_POINT ( 'NONE',  ( -95.19752181008296077, -297.1866683211546274, -320.4211037123490655 ) ) ;
#35313 = CARTESIAN_POINT ( 'NONE',  ( -57.90274796562979276, -297.6123617108498252, -200.3165370621973977 ) ) ;
#35314 = CARTESIAN_POINT ( 'NONE',  ( -51.09386068274324799, -291.2279474034933742, -344.1426212696375728 ) ) ;
#35315 = CARTESIAN_POINT ( 'NONE',  ( -26.62320554959377006, -286.3514578286117853, -194.0572822414794416 ) ) ;
#35316 = CARTESIAN_POINT ( 'NONE',  ( -41.10728688480014625, -272.1449585913027249, -194.6385265679608949 ) ) ;
#35317 = CARTESIAN_POINT ( 'NONE',  ( 38.02394462383258400, -287.1873193955063925, -254.5169133978125160 ) ) ;
#35318 = CARTESIAN_POINT ( 'NONE',  ( -37.02612016570056142, -282.0360135039760507, -195.7169807954790883 ) ) ;
#35319 = EDGE_CURVE ( 'NONE', #52696, #6956, #55551, .T. ) ;
#35320 = CARTESIAN_POINT ( 'NONE',  ( -95.13537540735848097, -284.2428779053269636, -225.3596569305279615 ) ) ;
#35321 = CARTESIAN_POINT ( 'NONE',  ( -56.79729785548920518, -287.3027138213166154, -342.8473892216402987 ) ) ;
#35322 = CARTESIAN_POINT ( 'NONE',  ( 61.48257290429442889, 47.14312216093964025, -312.8229988924202871 ) ) ;
#35323 = CARTESIAN_POINT ( 'NONE',  ( -27.82233136360427750, -285.6839534929694082, -197.9223848359166027 ) ) ;
#35324 = CARTESIAN_POINT ( 'NONE',  ( 30.87355905880138707, -282.9485999712395596, -305.5676319588594083 ) ) ;
#35325 = CARTESIAN_POINT ( 'NONE',  ( -111.3184403234689483, -289.3532816506603353, -290.8614136740770277 ) ) ;
#35326 = CARTESIAN_POINT ( 'NONE',  ( -68.36566886428350642, -281.2515098213852980, -200.7483611714270637 ) ) ;
#35327 = CARTESIAN_POINT ( 'NONE',  ( -99.04016210309333701, -280.4722264883238836, -225.0996595195135512 ) ) ;
#35328 = CARTESIAN_POINT ( 'NONE',  ( 21.00862402647616989, -282.0016731778902113, -314.2479301254109032 ) ) ;
#35329 = CARTESIAN_POINT ( 'NONE',  ( 30.89540736609959382, -277.1423916892329657, -239.1116677640277999 ) ) ;
#35330 = CARTESIAN_POINT ( 'NONE',  ( 24.02897609703129689, -294.1717096876017763, -316.8653124135184953 ) ) ;
#35331 = CARTESIAN_POINT ( 'NONE',  ( -7.585482484714454188, -286.6803959945262932, -338.8737553279843837 ) ) ;
#35332 = CARTESIAN_POINT ( 'NONE',  ( 38.80816098110800283, -295.1872088678599653, -273.1250041152688368 ) ) ;
#35333 = CARTESIAN_POINT ( 'NONE',  ( -107.9040592593216417, -295.2108041010885131, -290.2402414033725222 ) ) ;
#35334 = ORIENTED_EDGE ( 'NONE', *, *, #7047, .T. ) ;
#35335 = CARTESIAN_POINT ( 'NONE',  ( 35.64736362416090287, -283.6623426501461722, -285.0510579369343986 ) ) ;
#35336 = CARTESIAN_POINT ( 'NONE',  ( -109.0656378708356158, -296.4004569082486569, -256.5918340760067622 ) ) ;
#35337 = AXIS2_PLACEMENT_3D ( 'NONE', #27721, #34814, #42366 ) ;
#35338 = CARTESIAN_POINT ( 'NONE',  ( 21.96145215872486389, -293.9761660017497888, -221.7336705896772457 ) ) ;
#35339 = CARTESIAN_POINT ( 'NONE',  ( -26.71977809016659933, -283.5650285303413511, -342.7386086586990928 ) ) ;
#35340 = EDGE_CURVE ( 'NONE', #21738, #61290, #24668, .T. ) ;
#35341 = ADVANCED_FACE ( 'NONE', ( #92436, #76391, #11515 ), #41784, .F. ) ;
#35342 = CARTESIAN_POINT ( 'NONE',  ( -55.26701246912546139, -272.8857476170014138, -195.7186140738851918 ) ) ;
#35343 = CARTESIAN_POINT ( 'NONE',  ( -93.51265647848390472, -290.4857252523443663, -322.9558131065182351 ) ) ;
#35344 = CARTESIAN_POINT ( 'NONE',  ( -21.99963323167070328, -280.9971832273852215, -344.5563096135813339 ) ) ;
#35345 = CARTESIAN_POINT ( 'NONE',  ( -114.2299764661069759, -290.8387301814705665, -274.0943810606559623 ) ) ;
#35346 = CARTESIAN_POINT ( 'NONE',  ( 35.29499233449146089, -287.7867479008825171, -262.8779104595309946 ) ) ;
#35347 = CARTESIAN_POINT ( 'NONE',  ( 208.4306832106271088, -134.2391364535880882, 0.000000000000000000 ) ) ;
#35348 = CIRCLE ( 'NONE', #8093, 4.000000000000003553 ) ;
#35349 = CARTESIAN_POINT ( 'NONE',  ( 184.7149167944524493, 8.542400036368780647, 10.00000000000000178 ) ) ;
#35350 = CARTESIAN_POINT ( 'NONE',  ( 138.5936043815089249, 178.2952344932181461, -238.2260155999035192 ) ) ;
#35351 = CARTESIAN_POINT ( 'NONE',  ( -37.30987171927208834, -271.5523547857346784, -195.3611179825600175 ) ) ;
#35352 = CARTESIAN_POINT ( 'NONE',  ( -85.58300483283683491, -278.5614089002287983, -215.3576794820942553 ) ) ;
#35353 = ORIENTED_EDGE ( 'NONE', *, *, #82664, .F. ) ;
#35354 = CARTESIAN_POINT ( 'NONE',  ( -62.40174770981307972, -278.6387869451376673, -201.4147233026683068 ) ) ;
#35355 = CARTESIAN_POINT ( 'NONE',  ( 39.35907415515357854, -275.3006515257243336, -276.8983586705458038 ) ) ;
#35356 = CARTESIAN_POINT ( 'NONE',  ( -109.1495399033135385, -270.4770199085714921, -295.6887214991818382 ) ) ;
#35357 = CARTESIAN_POINT ( 'NONE',  ( -113.7956355219171343, -277.1115102838527378, -271.5807374497644560 ) ) ;
#35359 = CARTESIAN_POINT ( 'NONE',  ( -62.10361138193461983, -281.3956773573856935, -340.8335602679312615 ) ) ;
#35358 = AXIS2_PLACEMENT_3D ( 'NONE', #78710, #58345, #57415 ) ;
#35360 = CARTESIAN_POINT ( 'NONE',  ( -89.99355683654316351, -297.5433521758166080, -325.2218215773887664 ) ) ;
#35361 = PRODUCT_DEFINITION_SHAPE ( 'NONE', 'NONE',  #93720 ) ;
#35362 = CARTESIAN_POINT ( 'NONE',  ( 32.81102065386793498, -294.3147946737682332, -290.8164930270691571 ) ) ;
#35363 = EDGE_LOOP ( 'NONE', ( #36389, #4379, #85043, #25890 ) ) ;
#35364 = CARTESIAN_POINT ( 'NONE',  ( -94.66510066510163313, -289.8828471751627944, -224.3490475274149674 ) ) ;
#35365 = CARTESIAN_POINT ( 'NONE',  ( -13.10249022103224270, -275.0104237766035453, -197.3832207158263259 ) ) ;
#35366 = CARTESIAN_POINT ( 'NONE',  ( -37.82464763943075070, -298.2126168200189227, -197.3627154915492383 ) ) ;
#35367 = ORIENTED_EDGE ( 'NONE', *, *, #88464, .F. ) ;
#35368 = DIRECTION ( 'NONE',  ( -0.000000000000000000, -0.000000000000000000, 1.000000000000000000 ) ) ;
#35369 = VECTOR ( 'NONE', #38763, 1000.000000000000000 ) ;
#35370 = AXIS2_PLACEMENT_3D ( 'NONE', #20204, #49083, #77981 ) ;
#35371 = EDGE_CURVE ( 'NONE', #37103, #78803, #73076, .T. ) ;
#35372 = CARTESIAN_POINT ( 'NONE',  ( 150.6539576904058606, 293.9636489450775230, 0.000000000000000000 ) ) ;
#35373 = AXIS2_PLACEMENT_3D ( 'NONE', #85106, #78945, #5591 ) ;
#35374 = CARTESIAN_POINT ( 'NONE',  ( -68.66780278378681146, -280.7100926693755127, -204.0821517331897326 ) ) ;
#35375 = CARTESIAN_POINT ( 'NONE',  ( -20.00943296855395204, -282.0319375529127797, -196.3235165764820920 ) ) ;
#35376 = CARTESIAN_POINT ( 'NONE',  ( -110.3312503004726608, -283.5320716230345397, -276.3556165693473758 ) ) ;
#35377 = CARTESIAN_POINT ( 'NONE',  ( 1.018271775213363650, -282.4299549386903436, -206.7455215406967852 ) ) ;
#35378 = CARTESIAN_POINT ( 'NONE',  ( 18.82440290605323341, -274.7040443977327300, -318.0693628042634487 ) ) ;
#35379 = CARTESIAN_POINT ( 'NONE',  ( 209.9972545312790544, 27.55378999303206200, 10.50000000000000000 ) ) ;
#35380 = DIRECTION ( 'NONE',  ( 0.000000000000000000, 1.000000000000000000, 0.000000000000000000 ) ) ;
#35381 = CARTESIAN_POINT ( 'NONE',  ( -77.72132687017663955, -278.3821887997426074, -335.7960623972807639 ) ) ;
#35382 = AXIS2_PLACEMENT_3D ( 'NONE', #58618, #79915, #67115 ) ;
#35383 = DIRECTION ( 'NONE',  ( 0.000000000000000000, 0.000000000000000000, -1.000000000000000000 ) ) ;
#35384 = ORIENTED_EDGE ( 'NONE', *, *, #86333, .T. ) ;
#35385 = FACE_OUTER_BOUND ( 'NONE', #71152, .T. ) ;
#35386 = CARTESIAN_POINT ( 'NONE',  ( -70.98135671140305192, -285.4737339476653801, -337.7909356585846012 ) ) ;
#35387 = CARTESIAN_POINT ( 'NONE',  ( 34.37680400917464141, -292.5590021248916059, -255.9022835984209792 ) ) ;
#35388 = CARTESIAN_POINT ( 'NONE',  ( -34.67866899794705660, -288.3681006042632475, -347.2130603918622569 ) ) ;
#35389 = CARTESIAN_POINT ( 'NONE',  ( -52.27174511611867302, -284.0982131031319682, -197.8692717680117710 ) ) ;
#35391 = CARTESIAN_POINT ( 'NONE',  ( -87.43143793499899630, -288.0018076344250062, -324.9191241967814676 ) ) ;
#35390 = CARTESIAN_POINT ( 'NONE',  ( -104.0116636951921265, -283.5456209448807954, -239.0876811960825705 ) ) ;
#35392 = CARTESIAN_POINT ( 'NONE',  ( -10.81803359171806456, -283.9036357956117627, -338.8520147168692347 ) ) ;
#35393 = CARTESIAN_POINT ( 'NONE',  ( -36.92459258890065144, -272.0572502219812350, -195.3495599354373837 ) ) ;
#35394 = CARTESIAN_POINT ( 'NONE',  ( -107.4986434170018015, -282.5679858648593381, -300.2357864277485078 ) ) ;
#35395 = CARTESIAN_POINT ( 'NONE',  ( -71.14909938523703659, -297.4985909073644166, -337.3093099517820974 ) ) ;
#35396 = CARTESIAN_POINT ( 'NONE',  ( -49.03381529791319338, -283.9034929611922848, -196.0569101383812267 ) ) ;
#35397 = CARTESIAN_POINT ( 'NONE',  ( -102.0592721434700252, -279.0279633579047527, -304.6400374502080126 ) ) ;
#35398 = CARTESIAN_POINT ( 'NONE',  ( 25.91604973283455493, -290.0990160655243812, -311.0586840981738987 ) ) ;
#35399 = CARTESIAN_POINT ( 'NONE',  ( 200.3186454232214828, 275.5000000000000568, -3.421094783296264374 ) ) ;
#35400 = CARTESIAN_POINT ( 'NONE',  ( 220.4471435719830197, 34.91984470236808136, -7.000000000000000888 ) ) ;
#35401 = CARTESIAN_POINT ( 'NONE',  ( 38.16873689043865880, -295.5071830387250316, -273.0975566514466664 ) ) ;
#35402 = CARTESIAN_POINT ( 'NONE',  ( -109.0358133292690752, -276.2660599902676495, -292.5569101221272490 ) ) ;
#35403 = CARTESIAN_POINT ( 'NONE',  ( -111.7681878592238292, -289.5091854243160014, -289.5150058189582296 ) ) ;
#35404 = CARTESIAN_POINT ( 'NONE',  ( -85.01020390609726007, -294.1222714751994545, -326.7678634916808278 ) ) ;
#35405 = CARTESIAN_POINT ( 'NONE',  ( -39.70039309408342376, -278.7067698291309057, -196.8932206199147572 ) ) ;
#35406 = CARTESIAN_POINT ( 'NONE',  ( -81.91406062905878116, -271.5197303448059074, -210.6758288227294997 ) ) ;
#35407 = CARTESIAN_POINT ( 'NONE',  ( -5.845371623542153117, -293.7903173055038337, -203.9452511240053525 ) ) ;
#35408 = CARTESIAN_POINT ( 'NONE',  ( -69.85430415644619018, -279.9805209788416391, -337.9475929042657754 ) ) ;
#35409 = CARTESIAN_POINT ( 'NONE',  ( -4.815798806994362025, -293.1114493030560766, -339.4027942529838811 ) ) ;
#35410 = CARTESIAN_POINT ( 'NONE',  ( -73.92400415662122271, -291.1467725700177311, -334.4707355352870763 ) ) ;
#35411 = CARTESIAN_POINT ( 'NONE',  ( 12.62915964942925484, -290.9776741098256139, -213.1170162376579640 ) ) ;
#35412 = ADVANCED_FACE ( 'NONE', ( #26183 ), #19549, .F. ) ;
#35413 = CARTESIAN_POINT ( 'NONE',  ( 10.51209116820994538, -289.8016599912456286, -326.3336933605255012 ) ) ;
#35414 = DIRECTION ( 'NONE',  ( 0.000000000000000000, -1.000000000000000000, -0.000000000000000000 ) ) ;
#35415 = CARTESIAN_POINT ( 'NONE',  ( -70.03544029195215614, -290.2970748734683184, -335.8251484747642053 ) ) ;
#35416 = CYLINDRICAL_SURFACE ( 'NONE', #79310, 7.999999999999992895 ) ;
#35417 = CARTESIAN_POINT ( 'NONE',  ( -101.9580256934992946, -291.2139989372096238, -311.6016137616600759 ) ) ;
#35419 = CARTESIAN_POINT ( 'NONE',  ( -65.32695985371928771, -291.6759040720776284, -202.9248685316386798 ) ) ;
#35418 = CARTESIAN_POINT ( 'NONE',  ( 36.64467246944092693, -279.3895479394639665, -256.0634442057819342 ) ) ;
#35420 = AXIS2_PLACEMENT_3D ( 'NONE', #4504, #90198, #32922 ) ;
#35421 = CARTESIAN_POINT ( 'NONE',  ( -50.93962971697916231, -279.8829872176186200, -194.5713013124071438 ) ) ;
#35422 = CARTESIAN_POINT ( 'NONE',  ( 21.59108881676021596, -281.8858973652204440, -319.8855632474826507 ) ) ;
#35423 = CARTESIAN_POINT ( 'NONE',  ( -6.162439755335780589, -284.4616492636437215, -202.1351779158216004 ) ) ;
#35424 = CARTESIAN_POINT ( 'NONE',  ( 12.73271565463508992, -280.4842665362771186, -325.1645700833301476 ) ) ;
#35425 = CARTESIAN_POINT ( 'NONE',  ( -94.28103874402968643, -283.2289695988396261, -221.4681694013947890 ) ) ;
#35426 = CARTESIAN_POINT ( 'NONE',  ( -17.15659691235342876, -278.7880140560332052, -196.7726042104499413 ) ) ;
#35427 = AXIS2_PLACEMENT_3D ( 'NONE', #26544, #61600, #70585 ) ;
#35428 = CARTESIAN_POINT ( 'NONE',  ( 32.43651670737484949, -286.0626436911474002, -238.4135341959922130 ) ) ;
#35429 = CARTESIAN_POINT ( 'NONE',  ( 33.98891344527550018, -276.1402358258592926, -254.0402931635526897 ) ) ;
#35430 = CARTESIAN_POINT ( 'NONE',  ( 196.1222352346529192, 41.73615019500982726, 13.73113889404878485 ) ) ;
#35431 = CARTESIAN_POINT ( 'NONE',  ( -38.93505923740826802, -293.6319629735266403, -196.5783176565981307 ) ) ;
#35432 = CARTESIAN_POINT ( 'NONE',  ( 38.33806485315447077, -276.8445348388815432, -259.8169506347200013 ) ) ;
#35433 = CARTESIAN_POINT ( 'NONE',  ( -106.2855763294272151, -277.8971079005302158, -294.5733663795613779 ) ) ;
#35434 = CARTESIAN_POINT ( 'NONE',  ( -77.17108033825789448, -291.7008577034122254, -204.4010627264145228 ) ) ;
#35435 = VECTOR ( 'NONE', #64907, 1000.000000000000000 ) ;
#35436 = CARTESIAN_POINT ( 'NONE',  ( -5.527616766370074153, -278.5472189395063651, -201.8251544180090775 ) ) ;
#35437 = AXIS2_PLACEMENT_3D ( 'NONE', #10525, #54549, #82507 ) ;
#35438 = CARTESIAN_POINT ( 'NONE',  ( -69.62122395575467237, -291.4722118480507334, -200.4394641163905249 ) ) ;
#35439 = CARTESIAN_POINT ( 'NONE',  ( -107.2225524608957130, -289.9008563869512614, -248.4082829704373125 ) ) ;
#35440 = CARTESIAN_POINT ( 'NONE',  ( -63.59070751608000904, -293.3941268107629980, -340.6177209436892781 ) ) ;
#35441 = ORIENTED_EDGE ( 'NONE', *, *, #9521, .F. ) ;
#35442 = CARTESIAN_POINT ( 'NONE',  ( 153.1901962297558839, 19.73438857711721894, 11.80184082123541423 ) ) ;
#35443 = CIRCLE ( 'NONE', #88333, 3.842139515347647638 ) ;
#35444 = CARTESIAN_POINT ( 'NONE',  ( -66.58295218394705728, -291.1661396866224436, -203.4063749092488820 ) ) ;
#35445 = CYLINDRICAL_SURFACE ( 'NONE', #45899, 1.000000000000000888 ) ;
#35446 = CARTESIAN_POINT ( 'NONE',  ( 17.36665895637873192, -273.6952119285918457, -314.0302885647153062 ) ) ;
#35447 = CARTESIAN_POINT ( 'NONE',  ( -111.7435737959687145, -295.3730917661030162, -289.3134617385844081 ) ) ;
#35448 = CARTESIAN_POINT ( 'NONE',  ( -93.06082709831257205, -285.1469095971032743, -322.8081474383906198 ) ) ;
#35449 = CARTESIAN_POINT ( 'NONE',  ( -38.62277864818258166, -285.8689994018389484, -197.3598779483117767 ) ) ;
#35450 = CARTESIAN_POINT ( 'NONE',  ( 29.70892005420766679, -276.6624304283904507, -239.6612491835425374 ) ) ;
#35451 = CARTESIAN_POINT ( 'NONE',  ( -37.01307056537550011, -293.0680948198364604, -345.0179024847935239 ) ) ;
#35452 = CARTESIAN_POINT ( 'NONE',  ( -109.5760164090117570, -298.1024255590058942, -286.4911386907660358 ) ) ;
#35453 = AXIS2_PLACEMENT_3D ( 'NONE', #50704, #79592, #36028 ) ;
#35454 = CARTESIAN_POINT ( 'NONE',  ( 7.812662599335469693, -275.2149017442992545, -328.2896233777790940 ) ) ;
#35455 = ORIENTED_EDGE ( 'NONE', *, *, #63047, .F. ) ;
#35456 = CARTESIAN_POINT ( 'NONE',  ( 195.7178114849801318, 40.54307234874452348, 13.60494157104296953 ) ) ;
#35457 = CARTESIAN_POINT ( 'NONE',  ( -79.46894210689021065, -295.2712311838648702, -334.7896813277532146 ) ) ;
#35458 = CARTESIAN_POINT ( 'NONE',  ( -15.40439500297898689, -290.6862747222315306, -341.5491525112072395 ) ) ;
#35459 = DIRECTION ( 'NONE',  ( 0.000000000000000000, 0.000000000000000000, 1.000000000000000000 ) ) ;
#35460 = CARTESIAN_POINT ( 'NONE',  ( 25.78825877897586594, -288.7099537500333213, -307.3190575948840433 ) ) ;
#35461 = ORIENTED_EDGE ( 'NONE', *, *, #65933, .F. ) ;
#35462 = CARTESIAN_POINT ( 'NONE',  ( -6.314446994652713308, -279.5086174983890714, -200.1320052817969213 ) ) ;
#35463 = CARTESIAN_POINT ( 'NONE',  ( -16.52648650585935641, -295.4415855182214727, -344.4435695842685163 ) ) ;
#35464 = CARTESIAN_POINT ( 'NONE',  ( -71.37322890248786678, -287.6363422902873594, -338.0527757644180156 ) ) ;
#35465 = CARTESIAN_POINT ( 'NONE',  ( -113.7543057210643695, -297.0020208053404644, -261.0413541453291373 ) ) ;
#35466 = CARTESIAN_POINT ( 'NONE',  ( 31.81969329244595812, -293.5723878375407025, -246.7774943301253927 ) ) ;
#35467 = CARTESIAN_POINT ( 'NONE',  ( 197.4476397837911463, 67.35440902555335185, -10.31415233767359929 ) ) ;
#35468 = DIRECTION ( 'NONE',  ( -0.000000000000000000, -1.000000000000000000, -0.000000000000000000 ) ) ;
#35469 = CARTESIAN_POINT ( 'NONE',  ( 189.4188515237862589, 293.9636489450775798, -9.103929867429222611 ) ) ;
#35470 = CARTESIAN_POINT ( 'NONE',  ( 18.15398598407957564, -289.7939477327786904, -322.7341699796975263 ) ) ;
#35471 = CARTESIAN_POINT ( 'NONE',  ( -119.3990491898856732, -294.0523547857346784, -270.3284710469131937 ) ) ;
#35472 = VERTEX_POINT ( 'NONE', #48415 ) ;
#35473 = CARTESIAN_POINT ( 'NONE',  ( -82.17269701044327235, -278.8067737953701908, -207.8831658327532068 ) ) ;
#35474 = CARTESIAN_POINT ( 'NONE',  ( -18.24377381170336676, -284.8057763897393784, -342.7702001993695831 ) ) ;
#35475 = CARTESIAN_POINT ( 'NONE',  ( -37.95933222389735562, -284.6192906643012179, -193.9528407740463933 ) ) ;
#35476 = CARTESIAN_POINT ( 'NONE',  ( 36.38320225558939569, -285.7663519917486497, -280.7470542302582430 ) ) ;
#35477 = CARTESIAN_POINT ( 'NONE',  ( 25.06318338630315878, -277.9900370645592602, -313.4163189315645468 ) ) ;
#35479 = ORIENTED_EDGE ( 'NONE', *, *, #48515, .T. ) ;
#35478 = ADVANCED_FACE ( 'NONE', ( #62672 ), #42248, .F. ) ;
#35481 = CARTESIAN_POINT ( 'NONE',  ( -51.83947225011938542, -279.2104355055322458, -198.6594224968718834 ) ) ;
#35480 = CARTESIAN_POINT ( 'NONE',  ( -110.3919325758372594, -278.5484989262219528, -270.6380536738776641 ) ) ;
#35482 = CARTESIAN_POINT ( 'NONE',  ( -3.973080912198417636, -275.5616219418762398, -201.2957622270114655 ) ) ;
#35483 = CARTESIAN_POINT ( 'NONE',  ( -110.9514180564329990, -277.6143165612652410, -249.1569168530786271 ) ) ;
#35484 = CARTESIAN_POINT ( 'NONE',  ( 200.9738417244596178, 294.2968953162039156, -68.37162730693829360 ) ) ;
#35485 = CARTESIAN_POINT ( 'NONE',  ( -92.00993445479919330, -274.2358724459490986, -216.4704474699857712 ) ) ;
#35486 = ADVANCED_FACE ( 'NONE', ( #91973, #33761 ), #49373, .T. ) ;
#35487 = CONTEXT_DEPENDENT_SHAPE_REPRESENTATION ( #49304, #92007 ) ;
#35488 = CARTESIAN_POINT ( 'NONE',  ( -9.396827642807163983, -299.8208190870045655, -193.9437202937408813 ) ) ;
#35489 = CARTESIAN_POINT ( 'NONE',  ( -95.99890600148557951, -281.6948066931273615, -223.6242672951989618 ) ) ;
#35490 = DIRECTION ( 'NONE',  ( 0.000000000000000000, 0.000000000000000000, 1.000000000000000000 ) ) ;
#35491 = CARTESIAN_POINT ( 'NONE',  ( -49.48621853281270688, -286.9734890362925626, -198.0132261012766719 ) ) ;
#35492 = CARTESIAN_POINT ( 'NONE',  ( -46.40713285024969537, -287.6987542755727532, -194.9171524050337041 ) ) ;
#35493 = CARTESIAN_POINT ( 'NONE',  ( 33.79837243370585043, -287.1223522448397034, -287.1832089486352970 ) ) ;
#35494 = CARTESIAN_POINT ( 'NONE',  ( -108.1729423791250753, -283.6755887557876008, -300.5384428048024574 ) ) ;
#35495 = CARTESIAN_POINT ( 'NONE',  ( -36.98422120466628371, -278.4565726065222862, -196.5619809515205816 ) ) ;
#35496 = CARTESIAN_POINT ( 'NONE',  ( -69.32826939448453629, -287.4871641778752291, -203.3566091398639912 ) ) ;
#35497 = CARTESIAN_POINT ( 'NONE',  ( 21.07731089913698952, -279.4055687813314535, -225.4192596737672716 ) ) ;
#35498 = CARTESIAN_POINT ( 'NONE',  ( 12.09171111390374520, -277.6629190006742647, -324.8138380611150637 ) ) ;
#35499 = CARTESIAN_POINT ( 'NONE',  ( 29.21290243875100856, -276.4503908358885838, -300.5020091212221018 ) ) ;
#35500 = CARTESIAN_POINT ( 'NONE',  ( -41.75310905305579467, -287.9014657229816407, -346.8500732827675392 ) ) ;
#35501 = CARTESIAN_POINT ( 'NONE',  ( -90.31938848510732498, -284.5814777130545394, -326.0894620818544922 ) ) ;
#35502 = CARTESIAN_POINT ( 'NONE',  ( -108.9734851424181841, -285.4023364658055470, -242.1374834191706498 ) ) ;
#35503 = CARTESIAN_POINT ( 'NONE',  ( 9.274907507419671404, -280.8798851831136290, -214.1178997202809171 ) ) ;
#35504 = EDGE_LOOP ( 'NONE', ( #11454, #47572, #23204, #34662 ) ) ;
#35505 = ORIENTED_EDGE ( 'NONE', *, *, #25991, .T. ) ;
#35506 = DIRECTION ( 'NONE',  ( -0.000000000000000000, 1.000000000000000000, -0.000000000000000000 ) ) ;
#35507 = CARTESIAN_POINT ( 'NONE',  ( 21.46171059445233098, -290.0641252113188671, -318.1566883230302665 ) ) ;
#35508 = CARTESIAN_POINT ( 'NONE',  ( -111.1525730702722967, -289.4913092760557447, -250.1805432059843213 ) ) ;
#35509 = AXIS2_PLACEMENT_3D ( 'NONE', #72913, #14248, #29834 ) ;
#35510 = CARTESIAN_POINT ( 'NONE',  ( -110.5769942451401704, -271.6110516449974739, -270.3491615739666258 ) ) ;
#35511 = CARTESIAN_POINT ( 'NONE',  ( 33.31962016774464530, -293.2891678264079474, -300.8318522878861359 ) ) ;
#35512 = CARTESIAN_POINT ( 'NONE',  ( -73.90563459685535008, -288.0270258734280446, -334.3583724591348414 ) ) ;
#35513 = CARTESIAN_POINT ( 'NONE',  ( 35.05414176113733049, -291.9930243229286475, -285.8106542917220168 ) ) ;
#35514 = B_SPLINE_CURVE_WITH_KNOTS ( 'NONE', 3,
 ( #28092, #20516, #65021, #85366 ),
 .UNSPECIFIED., .F., .F.,
 ( 4, 4 ),
 ( 0.000000000000000000, 0.0006940106885258007230 ),
 .UNSPECIFIED. ) ;
#35515 = CARTESIAN_POINT ( 'NONE',  ( 23.84896899855845120, -289.3168631296668423, -310.9159516872866789 ) ) ;
#35516 = CARTESIAN_POINT ( 'NONE',  ( 35.77081079830085031, -295.8376638359844719, -253.6410175316879361 ) ) ;
#35517 = CARTESIAN_POINT ( 'NONE',  ( 11.14281742901739314, -290.3808272825906442, -327.5821997882495680 ) ) ;
#35518 = CARTESIAN_POINT ( 'NONE',  ( -104.3577542164685923, -289.0023027518378171, -236.2041471817235276 ) ) ;
#35519 = CARTESIAN_POINT ( 'NONE',  ( -107.7133135273980997, -292.8906291647765556, -244.2741010033949181 ) ) ;
#35520 = CARTESIAN_POINT ( 'NONE',  ( -69.10039032661624958, -284.4216962772506463, -336.3658274265531531 ) ) ;
#35521 = CARTESIAN_POINT ( 'NONE',  ( 12.05408248477928979, -294.7373705022885702, -213.7035052212461039 ) ) ;
#35522 = CARTESIAN_POINT ( 'NONE',  ( 189.9243309297870610, 250.5000000000000568, 20.22542485937349355 ) ) ;
#35523 = DIRECTION ( 'NONE',  ( 0.9951408606192332362, 0.000000000000000000, -0.09846150276129254919 ) ) ;
#35524 = CARTESIAN_POINT ( 'NONE',  ( -84.79248009415235288, -275.3815228900309080, -211.8219833771299534 ) ) ;
#35525 = AXIS2_PLACEMENT_3D ( 'NONE', #26859, #41511, #56702 ) ;
#35526 = CARTESIAN_POINT ( 'NONE',  ( -16.09535092101017995, -281.9674356062802758, -340.3696486909981900 ) ) ;
#35527 = CARTESIAN_POINT ( 'NONE',  ( -103.5484032776459600, -282.0833372688729810, -305.7091024207979899 ) ) ;
#35528 = CARTESIAN_POINT ( 'NONE',  ( -102.9829610885807654, -295.2266793465228147, -310.3033722968134498 ) ) ;
#35529 = CARTESIAN_POINT ( 'NONE',  ( 24.65437826159549672, -273.2394950067836703, -229.9326592251921682 ) ) ;
#35530 = CARTESIAN_POINT ( 'NONE',  ( -105.6014272423204829, -276.2389187174886729, -300.1875825290283615 ) ) ;
#35531 = CARTESIAN_POINT ( 'NONE',  ( -100.3280264514214792, -298.3860290119940828, -232.3943684674912049 ) ) ;
#35532 = CARTESIAN_POINT ( 'NONE',  ( -94.38788784590086323, -297.3244233046321483, -316.8686293091461721 ) ) ;
#35533 = FACE_OUTER_BOUND ( 'NONE', #86014, .T. ) ;
#35534 = CARTESIAN_POINT ( 'NONE',  ( -109.2990945701885437, -297.1800825185141548, -283.6492068335287513 ) ) ;
#35535 = CARTESIAN_POINT ( 'NONE',  ( 17.06571399127465583, -89.54582641780471874, -21.50000000000000000 ) ) ;
#35537 = CARTESIAN_POINT ( 'NONE',  ( -83.18893748377028885, -273.2369908975525163, -213.5541568656866787 ) ) ;
#35536 = CARTESIAN_POINT ( 'NONE',  ( 34.37448242459086600, -285.8695467260812393, -293.4954207105848241 ) ) ;
#35538 = CARTESIAN_POINT ( 'NONE',  ( 36.67207139781474012, -286.9514167653484265, -249.0127451384059043 ) ) ;
#35539 = CARTESIAN_POINT ( 'NONE',  ( -3.934788865591847262, -296.5937064219432386, -337.9208416878618095 ) ) ;
#35540 = CARTESIAN_POINT ( 'NONE',  ( 24.10757764472594999, -290.9710883043557601, -227.6300444767181830 ) ) ;
#35541 = EDGE_CURVE ( 'NONE', #41591, #61220, #42854, .T. ) ;
#35542 = CARTESIAN_POINT ( 'NONE',  ( -69.88466448665414532, -278.8316166907081879, -200.7399043162345151 ) ) ;
#35543 = EDGE_CURVE ( 'NONE', #12291, #72750, #59494, .T. ) ;
#35544 = CARTESIAN_POINT ( 'NONE',  ( -54.42813229853332757, -295.3380690714490129, -195.3538533559490702 ) ) ;
#35545 = CARTESIAN_POINT ( 'NONE',  ( 201.2104617360081704, 250.0000000000000568, 15.00000000000000000 ) ) ;
#35546 = CARTESIAN_POINT ( 'NONE',  ( -11.86987106776820511, -285.1862079733425048, -201.5256879404417418 ) ) ;
#35547 = CARTESIAN_POINT ( 'NONE',  ( 197.3691676728705033, 70.32516635541138328, -11.79160090895328139 ) ) ;
#35548 = CARTESIAN_POINT ( 'NONE',  ( 7.007303246093505855, -286.4486423079699762, -330.9086037081987115 ) ) ;
#35549 = CARTESIAN_POINT ( 'NONE',  ( 9.546310512083316269, -300.2487942568411086, -196.5480832843507812 ) ) ;
#35550 = CARTESIAN_POINT ( 'NONE',  ( -79.60014461081689774, -280.9189174290218034, -206.6357955574420089 ) ) ;
#35552 = CARTESIAN_POINT ( 'NONE',  ( -6.032943655893342694, -282.6288903448995029, -336.3200104194942810 ) ) ;
#35551 = CARTESIAN_POINT ( 'NONE',  ( -112.4786176582602053, -294.6537535082063641, -263.9840069950697057 ) ) ;
#35553 = CARTESIAN_POINT ( 'NONE',  ( -114.3098143371742168, -296.7641514905550935, -266.7373965977121202 ) ) ;
#35554 = CARTESIAN_POINT ( 'NONE',  ( -102.5610064780436517, -274.4388730627857171, -236.1652610441418574 ) ) ;
#35555 = CARTESIAN_POINT ( 'NONE',  ( -10.48252730804613897, -284.4795664665907111, -199.6803121136453001 ) ) ;
#35556 = CARTESIAN_POINT ( 'NONE',  ( -20.23774003576258806, -282.2719182022274254, -197.2841128585155275 ) ) ;
#35557 = CARTESIAN_POINT ( 'NONE',  ( -100.0922376137794458, -296.1299664686275719, -232.5030424647576979 ) ) ;
#35558 = ORIENTED_EDGE ( 'NONE', *, *, #24079, .T. ) ;
#35559 = CARTESIAN_POINT ( 'NONE',  ( 183.0442525570908288, 264.6571197653884155, 7.500000000000000000 ) ) ;
#35560 = CARTESIAN_POINT ( 'NONE',  ( -81.58112478838474146, -285.6370029104722335, -330.5479537597688022 ) ) ;
#35561 = DIRECTION ( 'NONE',  ( 0.000000000000000000, 1.000000000000000000, 0.000000000000000000 ) ) ;
#35562 = CARTESIAN_POINT ( 'NONE',  ( -4.829096099716524648, -286.1237833571632905, -337.9475929042657754 ) ) ;
#35563 = CARTESIAN_POINT ( 'NONE',  ( 38.57459002123052727, -274.9022556706869977, -282.5638851485002760 ) ) ;
#35564 = CARTESIAN_POINT ( 'NONE',  ( -25.40700136800590059, -292.0416943095534066, -198.2918429051778162 ) ) ;
#35565 = CARTESIAN_POINT ( 'NONE',  ( 5.308823781287471455, -282.1612441236668474, -210.2641915961094981 ) ) ;
#35566 = CARTESIAN_POINT ( 'NONE',  ( 27.47906547556778278, -277.6298989291624935, -305.7484320484457498 ) ) ;
#35567 = CARTESIAN_POINT ( 'NONE',  ( 1.701914455523916514, -284.1392592524099996, -335.7983900479193267 ) ) ;
#35568 = CARTESIAN_POINT ( 'NONE',  ( 14.19261064637782432, -281.1036916034582873, -322.6949364592601910 ) ) ;
#35569 = CARTESIAN_POINT ( 'NONE',  ( -90.91969204759215017, -281.2923472870057822, -217.8051170066295867 ) ) ;
#35570 = CARTESIAN_POINT ( 'NONE',  ( -46.12987281963491171, -297.9435993370572078, -193.8642682386428362 ) ) ;
#35571 = CARTESIAN_POINT ( 'NONE',  ( 35.20025596961704650, -275.7131136775552136, -296.3381156866676633 ) ) ;
#35572 = CARTESIAN_POINT ( 'NONE',  ( 32.16438303110388830, -295.1232582507774964, -243.7111911560612327 ) ) ;
#35573 = FACE_OUTER_BOUND ( 'NONE', #25281, .T. ) ;
#35574 = CARTESIAN_POINT ( 'NONE',  ( -22.36525510383600590, -293.0019250753132383, -344.6309744000934074 ) ) ;
#35575 = CARTESIAN_POINT ( 'NONE',  ( -76.59200930779327621, -273.0188863958001093, -208.7380567888023961 ) ) ;
#35576 = CONICAL_SURFACE ( 'NONE', #41562, 4.999999999999990230, 1.029744258676656754 ) ;
#35577 = CARTESIAN_POINT ( 'NONE',  ( 36.43126210635471551, -295.3186095221691403, -289.8613179153579722 ) ) ;
#35578 = CARTESIAN_POINT ( 'NONE',  ( -2.136234668907611489, -295.8015957772047955, -338.3948149389269133 ) ) ;
#35579 = CARTESIAN_POINT ( 'NONE',  ( -37.24059935678067745, -291.0510410131372510, -345.1943873888910161 ) ) ;
#35580 = CARTESIAN_POINT ( 'NONE',  ( -107.2172423288878207, -276.9026434700369919, -243.4310942860465161 ) ) ;
#35581 = CARTESIAN_POINT ( 'NONE',  ( -4.407404038106616184, -278.5349154432033743, -337.1334024252158770 ) ) ;
#35582 = CARTESIAN_POINT ( 'NONE',  ( 35.90439305436713369, -291.4592984149966810, -257.0114057549722588 ) ) ;
#35583 = CARTESIAN_POINT ( 'NONE',  ( 20.11367479828315652, -282.7348283083477440, -220.9532887883599983 ) ) ;
#35584 = AXIS2_PLACEMENT_3D ( 'NONE', #35926, #27422, #21249 ) ;
#35585 = CARTESIAN_POINT ( 'NONE',  ( -68.89557852661957327, -284.5475529160565884, -204.1764409460664922 ) ) ;
#35586 = CARTESIAN_POINT ( 'NONE',  ( 47.08420963622742050, 10.99842292863093896, -330.8880468998681295 ) ) ;
#35587 = VERTEX_POINT ( 'NONE', #71161 ) ;
#35588 = CARTESIAN_POINT ( 'NONE',  ( -96.58949594620050050, -284.8158242663156443, -227.6574013950746576 ) ) ;
#35589 = CARTESIAN_POINT ( 'NONE',  ( -56.49280826896303864, -280.8907391186834275, -196.0451239601401596 ) ) ;
#35590 = CARTESIAN_POINT ( 'NONE',  ( -102.5879497504052580, -282.8197931624920329, -310.4975805594237386 ) ) ;
#35591 = CARTESIAN_POINT ( 'NONE',  ( -82.11138006969866865, -280.3991825900214394, -208.0033119734538900 ) ) ;
#35592 = CARTESIAN_POINT ( 'NONE',  ( -72.50381948162078061, -279.0290751780003120, -338.0981590714568483 ) ) ;
#35593 = CARTESIAN_POINT ( 'NONE',  ( -82.13390479932378696, -299.9090924074130271, -214.2458315076590907 ) ) ;
#35594 = VERTEX_POINT ( 'NONE', #5826 ) ;
#35595 = ORIENTED_EDGE ( 'NONE', *, *, #4770, .F. ) ;
#35596 = CARTESIAN_POINT ( 'NONE',  ( -78.63378679019862716, -299.4966662489894702, -207.6890795956263105 ) ) ;
#35597 = CARTESIAN_POINT ( 'NONE',  ( -100.8542679731100975, -277.1022976673459084, -231.0452144819477098 ) ) ;
#35598 = CARTESIAN_POINT ( 'NONE',  ( -113.3759036933542603, -292.3011591358191481, -271.2397103727222998 ) ) ;
#35599 = CARTESIAN_POINT ( 'NONE',  ( 19.76820487696091888, -293.5446538253959829, -316.0138586652342383 ) ) ;
#35600 = CARTESIAN_POINT ( 'NONE',  ( -41.76329274598327856, -288.6140791635320966, -347.1856335842026624 ) ) ;
#35601 = DIRECTION ( 'NONE',  ( -0.000000000000000000, -0.000000000000000000, 1.000000000000000000 ) ) ;
#35603 = CARTESIAN_POINT ( 'NONE',  ( -11.72540053608412869, -284.7912190347873889, -201.1495177252999440 ) ) ;
#35602 = CARTESIAN_POINT ( 'NONE',  ( -3.506153775527077521, -293.1890930628226215, -338.8866451305271426 ) ) ;
#35604 = CARTESIAN_POINT ( 'NONE',  ( -4.304300342531534262, -294.3526987455283574, -203.8684239043339517 ) ) ;
#35605 = CARTESIAN_POINT ( 'NONE',  ( -5.481530360466991603, -284.9588735154609367, -203.8969395708655554 ) ) ;
#35606 = CARTESIAN_POINT ( 'NONE',  ( -38.87871202335794152, -284.3869739256532512, -343.8507720152429101 ) ) ;
#35607 = CARTESIAN_POINT ( 'NONE',  ( -113.9537707808432856, -291.5540996660268434, -265.5226427393353106 ) ) ;
#35608 = CARTESIAN_POINT ( 'NONE',  ( 21.37469264596427720, -281.4351506659519373, -226.8616363258992124 ) ) ;
#35609 = CARTESIAN_POINT ( 'NONE',  ( 24.55632620255637022, -292.9494285973721048, -315.5123895803252481 ) ) ;
#35610 = CARTESIAN_POINT ( 'NONE',  ( 25.72504150123767985, -288.9372845093539013, -314.3471929137066354 ) ) ;
#35611 = ADVANCED_FACE ( 'NONE', ( #78266 ), #84487, .T. ) ;
#35612 = CARTESIAN_POINT ( 'NONE',  ( -95.40773584403584096, -290.3616619358701882, -320.8374728391015651 ) ) ;
#35613 = CARTESIAN_POINT ( 'NONE',  ( 25.69712109552919088, -288.2252986347052683, -307.2728344847255357 ) ) ;
#35614 = ORIENTED_EDGE ( 'NONE', *, *, #4911, .T. ) ;
#35615 = CARTESIAN_POINT ( 'NONE',  ( 194.3388778885402814, 26.65530528383262521, 14.52131005158982369 ) ) ;
#35616 = CARTESIAN_POINT ( 'NONE',  ( -22.31891828115328025, -296.7221580835962413, -344.6216155800368028 ) ) ;
#35617 = CARTESIAN_POINT ( 'NONE',  ( -35.82337579786811688, -296.7556195291638801, -193.8545962127014946 ) ) ;
#35618 = CARTESIAN_POINT ( 'NONE',  ( -110.5861044000194511, -277.6434088707502497, -267.8883994169286780 ) ) ;
#35619 = CARTESIAN_POINT ( 'NONE',  ( -92.12084595472303761, -272.8025043903053302, -216.3354566199294595 ) ) ;
#35620 = CARTESIAN_POINT ( 'NONE',  ( -5.256977876383158055, -293.1019368152330458, -336.7171886361172710 ) ) ;
#35621 = CARTESIAN_POINT ( 'NONE',  ( 35.10873661480165708, -277.1146375905308332, -255.1696209777039144 ) ) ;
#35622 = CARTESIAN_POINT ( 'NONE',  ( -98.85362310101784544, -271.2608817246718331, -228.7104735480878617 ) ) ;
#35623 = CARTESIAN_POINT ( 'NONE',  ( 13.16534093424485619, -293.9825340517983818, -217.1054205664788412 ) ) ;
#35624 = CARTESIAN_POINT ( 'NONE',  ( -69.84882497563455672, -296.5703777250566304, -336.0689022153982819 ) ) ;
#35625 = CARTESIAN_POINT ( 'NONE',  ( -43.50955339366421981, -251.5889492418373266, -450.1178138017020274 ) ) ;
#35626 = CARTESIAN_POINT ( 'NONE',  ( -89.45970809972031645, -293.7836561774128086, -324.5968288064988201 ) ) ;
#35627 = CARTESIAN_POINT ( 'NONE',  ( -51.78960768913849932, -298.5235050161888921, -194.7782406503994821 ) ) ;
#35628 = CARTESIAN_POINT ( 'NONE',  ( 28.74905534621937164, -286.5617600331370909, -302.7244762176450763 ) ) ;
#35629 = CARTESIAN_POINT ( 'NONE',  ( -105.0205097476559644, -274.9777367158422408, -238.0411647941178614 ) ) ;
#35630 = CARTESIAN_POINT ( 'NONE',  ( -112.3846526553913776, -273.2569368302204680, -253.3881341676984675 ) ) ;
#35631 = CARTESIAN_POINT ( 'NONE',  ( -98.74878486601731709, -296.3376499812720226, -309.9664894402433788 ) ) ;
#35632 = EDGE_CURVE ( 'NONE', #28339, #43507, #57427, .T. ) ;
#35633 = CARTESIAN_POINT ( 'NONE',  ( -112.0889811220736050, -280.6592057729443468, -260.4106016565929735 ) ) ;
#35634 = CARTESIAN_POINT ( 'NONE',  ( 38.78562209701920693, -280.3392097480020198, -278.4829295093748556 ) ) ;
#35635 = CARTESIAN_POINT ( 'NONE',  ( -21.75476477491436711, -282.2059913733568806, -345.6629123341503487 ) ) ;
#35636 = CARTESIAN_POINT ( 'NONE',  ( 34.08648801887899538, -275.2642023349746978, -298.9884388004801963 ) ) ;
#35637 = CARTESIAN_POINT ( 'NONE',  ( -11.75854859957883924, -278.7795138264719981, -198.5286759895561204 ) ) ;
#35638 = CARTESIAN_POINT ( 'NONE',  ( -64.06611331430070777, -277.7043532313207947, -200.0507439231699607 ) ) ;
#35639 = AXIS2_PLACEMENT_3D ( 'NONE', #45789, #51501, #30674 ) ;
#35640 = CARTESIAN_POINT ( 'NONE',  ( -99.77082865465118289, -271.6603413238086091, -231.3998702102258278 ) ) ;
#35641 = CARTESIAN_POINT ( 'NONE',  ( 23.83169745274588180, -276.9623185015346394, -226.9477369890688294 ) ) ;
#35642 = CARTESIAN_POINT ( 'NONE',  ( 160.5350683151633291, 250.5000000000000568, 24.72542485937379197 ) ) ;
#35643 = CARTESIAN_POINT ( 'NONE',  ( 36.45635138963580602, -291.3766982735485271, -255.0578793968104492 ) ) ;
#35644 = CARTESIAN_POINT ( 'NONE',  ( -101.6839608269671089, -291.1092619407325515, -227.9679967971410122 ) ) ;
#35645 = CARTESIAN_POINT ( 'NONE',  ( 17.58144542816662792, -278.2692377988443013, -321.6785273975654604 ) ) ;
#35646 = CARTESIAN_POINT ( 'NONE',  ( -69.10709424787449962, -271.6342739609892192, -202.4061871036267064 ) ) ;
#35647 = EDGE_CURVE ( 'NONE', #59134, #24951, #82175, .T. ) ;
#35648 = LINE ( 'NONE', #85813, #69544 ) ;
#35649 = FACE_OUTER_BOUND ( 'NONE', #79480, .T. ) ;
#35650 = CARTESIAN_POINT ( 'NONE',  ( -22.24705103918196514, -284.2451764123570683, -196.8433691840046720 ) ) ;
#35651 = AXIS2_PLACEMENT_3D ( 'NONE', #92172, #20695, #27329 ) ;
#35652 = DIRECTION ( 'NONE',  ( 0.000000000000000000, 0.000000000000000000, 1.000000000000000000 ) ) ;
#35653 = CARTESIAN_POINT ( 'NONE',  ( 32.18207957688112941, -292.0342789044797769, -246.6746413627150787 ) ) ;
#35654 = CARTESIAN_POINT ( 'NONE',  ( 34.59125077131827197, -285.4530311993144096, -251.9653702247021556 ) ) ;
#35655 = CARTESIAN_POINT ( 'NONE',  ( 165.2424497756046549, 275.0000000000000568, 22.91843887563435445 ) ) ;
#35656 = CARTESIAN_POINT ( 'NONE',  ( 157.4221907153413724, 15.99782226686453868, -9.062927103449267108 ) ) ;
#35657 = CARTESIAN_POINT ( 'NONE',  ( -37.01164480955512204, -293.0478298014481879, -345.3731601704226364 ) ) ;
#35658 = CARTESIAN_POINT ( 'NONE',  ( -76.41961876713757817, -282.0442731461977246, -335.9633993510827281 ) ) ;
#35659 = CARTESIAN_POINT ( 'NONE',  ( -98.66964972169510872, -280.7173433427058171, -229.2176549231458011 ) ) ;
#35660 = CARTESIAN_POINT ( 'NONE',  ( -105.0881373935143870, -286.2225377310180647, -234.4923749928344705 ) ) ;
#35661 = CARTESIAN_POINT ( 'NONE',  ( -7.908527205002114258, -278.6723627708439608, -200.2922913497037314 ) ) ;
#35662 = CARTESIAN_POINT ( 'NONE',  ( 35.55264398448798602, -287.4891697034146887, -265.5867029780700932 ) ) ;
#35663 = CARTESIAN_POINT ( 'NONE',  ( -81.15576975124106696, -279.0861569633106569, -329.4855817737606003 ) ) ;
#35664 = CARTESIAN_POINT ( 'NONE',  ( -103.5202686159419443, -279.7769454022767377, -239.0490774802385090 ) ) ;
#35665 = CARTESIAN_POINT ( 'NONE',  ( -105.2089308069749478, -286.9613679259056767, -237.6128997148364022 ) ) ;
#35666 = ORIENTED_EDGE ( 'NONE', *, *, #10935, .F. ) ;
#35667 = CARTESIAN_POINT ( 'NONE',  ( -36.18225594080007568, -297.8996140624144005, -193.3611496608207858 ) ) ;
#35668 = CARTESIAN_POINT ( 'NONE',  ( -12.72212176263686523, -290.7104039402578337, -340.8290054400819145 ) ) ;
#35669 = CARTESIAN_POINT ( 'NONE',  ( 197.7335303680046650, 24.96166607582781083, 12.00000000000000178 ) ) ;
#35670 = CARTESIAN_POINT ( 'NONE',  ( -88.52914483777347243, -281.9090924074130839, -206.2264541496106460 ) ) ;
#35671 = ORIENTED_EDGE ( 'NONE', *, *, #38515, .T. ) ;
#35672 = CARTESIAN_POINT ( 'NONE',  ( 23.02314523118107203, -272.9419774259030191, -225.5714554022020195 ) ) ;
#35673 = CARTESIAN_POINT ( 'NONE',  ( 27.41519983118940118, -292.4839354754254828, -310.6221847946114281 ) ) ;
#35674 = CARTESIAN_POINT ( 'NONE',  ( -47.80804525473786981, -294.6963550318693592, -342.7204223099776073 ) ) ;
#35675 = CARTESIAN_POINT ( 'NONE',  ( 36.24371113329314653, -289.0090469521384762, -265.5220676799170292 ) ) ;
#35676 = CARTESIAN_POINT ( 'NONE',  ( 18.71758528305098679, -282.6332287571396478, -222.0164127441720723 ) ) ;
#35677 = CARTESIAN_POINT ( 'NONE',  ( -43.11949770513703584, -290.5490251124095948, -346.5531342840275215 ) ) ;
#35678 = CARTESIAN_POINT ( 'NONE',  ( 22.90951944397731310, -289.5017811974460074, -317.5318607374728685 ) ) ;
#35679 = CARTESIAN_POINT ( 'NONE',  ( -109.9716663538028314, -286.7926487088613499, -251.6558070265734273 ) ) ;
#35680 = CARTESIAN_POINT ( 'NONE',  ( -103.6047097010405054, -278.2067200241035607, -309.6857391723037267 ) ) ;
#35681 = ORIENTED_EDGE ( 'NONE', *, *, #25637, .T. ) ;
#35682 = CARTESIAN_POINT ( 'NONE',  ( 36.05528065059214526, -291.8614408748849200, -288.3650417386569416 ) ) ;
#35683 = CARTESIAN_POINT ( 'NONE',  ( 38.25509172380060363, -281.2024669385270386, -255.7281050929548485 ) ) ;
#35684 = CARTESIAN_POINT ( 'NONE',  ( -70.05628937930782740, -275.4768869026192419, -203.7231323141346024 ) ) ;
#35685 = CARTESIAN_POINT ( 'NONE',  ( -69.91165696735023971, -288.1233781216987495, -202.8022627189028810 ) ) ;
#35686 = CARTESIAN_POINT ( 'NONE',  ( 22.84414049294219140, -273.1645078783168969, -223.9541726910825616 ) ) ;
#35687 = CARTESIAN_POINT ( 'NONE',  ( 197.8563597697584839, 24.47698789593438917, 12.00000000000000178 ) ) ;
#35688 = CARTESIAN_POINT ( 'NONE',  ( -81.31992600304128871, -278.9437314535050518, -211.9546083853312268 ) ) ;
#35689 = CARTESIAN_POINT ( 'NONE',  ( 18.62365015148619207, -277.4742813533255799, -322.6668374275178053 ) ) ;
#35690 = CARTESIAN_POINT ( 'NONE',  ( -105.3133474471421067, -298.3525514961377212, -242.1612939324398610 ) ) ;
#35691 = CARTESIAN_POINT ( 'NONE',  ( -27.41444184473359513, -281.9878390649325297, -346.5344163940760041 ) ) ;
#35692 = CARTESIAN_POINT ( 'NONE',  ( -83.15620781575645992, -291.4496448347164232, -328.4903266148244256 ) ) ;
#35693 = CARTESIAN_POINT ( 'NONE',  ( -113.0699119117287950, -274.2592728085912768, -261.8948109620706077 ) ) ;
#35694 = CARTESIAN_POINT ( 'NONE',  ( -71.19972443311384325, -274.9296880755725851, -201.7540304111158775 ) ) ;
#35695 = CARTESIAN_POINT ( 'NONE',  ( 19.37825820711082869, -296.2306114685429748, -319.1953626746648638 ) ) ;
#35696 = CARTESIAN_POINT ( 'NONE',  ( -67.31674705229335132, -281.4459563578201937, -338.9426996510161985 ) ) ;
#35697 = CARTESIAN_POINT ( 'NONE',  ( -112.2957123586946722, -290.4382974932345292, -252.8214389033918792 ) ) ;
#35698 = CARTESIAN_POINT ( 'NONE',  ( 35.49274659202517768, -273.7838106213210949, -286.7589880351060287 ) ) ;
#35699 = CARTESIAN_POINT ( 'NONE',  ( -26.75264705767810725, -287.7846753087542879, -194.8475083008703166 ) ) ;
#35700 = CARTESIAN_POINT ( 'NONE',  ( -108.7253268187797204, -289.6924569084037557, -253.6149846006159976 ) ) ;
#35701 = VERTEX_POINT ( 'NONE', #85808 ) ;
#35702 = CARTESIAN_POINT ( 'NONE',  ( -100.2062359093196875, -288.5488646877317365, -313.7967765379049183 ) ) ;
#35703 = CARTESIAN_POINT ( 'NONE',  ( -106.9735466448185690, -289.9254795745940214, -292.5168735078441387 ) ) ;
#35704 = ORIENTED_EDGE ( 'NONE', *, *, #71157, .T. ) ;
#35705 = CARTESIAN_POINT ( 'NONE',  ( 37.41521308436237803, -288.4162592285081246, -253.1886648918073490 ) ) ;
#35706 = CARTESIAN_POINT ( 'NONE',  ( -39.15403469166486872, -277.4088019899522237, -343.3597681775084993 ) ) ;
#35707 = CARTESIAN_POINT ( 'NONE',  ( -34.87839844508079068, -293.9422192775799090, -347.0124366629040082 ) ) ;
#35708 = CARTESIAN_POINT ( 'NONE',  ( -35.89278673019682486, -283.6858706970404000, -347.2586335577438490 ) ) ;
#35709 = CARTESIAN_POINT ( 'NONE',  ( -109.9587174054438634, -285.2077617760877501, -244.8167821481874000 ) ) ;
#35710 = CARTESIAN_POINT ( 'NONE',  ( 33.47504669929764987, -281.6498968822420466, -252.5037049940493432 ) ) ;
#35711 = CARTESIAN_POINT ( 'NONE',  ( 189.6301554638078244, 271.4469872958309793, -139.6143609917278638 ) ) ;
#35712 = CARTESIAN_POINT ( 'NONE',  ( 101.9353623535783981, 116.6993224611678386, -282.1991941425848154 ) ) ;
#35713 = CARTESIAN_POINT ( 'NONE',  ( 24.45853180448317588, -23.43590537780826466, -341.6733390498814629 ) ) ;
#35714 = CARTESIAN_POINT ( 'NONE',  ( -87.43643810223066737, -272.5290967060798266, -216.9708593713176867 ) ) ;
#35715 = CARTESIAN_POINT ( 'NONE',  ( 15.67982577811148026, -273.7446385433290175, -219.6620939320645789 ) ) ;
#35716 = CARTESIAN_POINT ( 'NONE',  ( -47.62955460570826460, -294.6872688541436673, -346.6086553418827521 ) ) ;
#35717 = CARTESIAN_POINT ( 'NONE',  ( 46.20262913025351992, 10.70065294047900295, -328.7549391094264593 ) ) ;
#35718 = CARTESIAN_POINT ( 'NONE',  ( 9.223534236405900089, -273.3616841466711094, -209.6571047707684841 ) ) ;
#35719 = CARTESIAN_POINT ( 'NONE',  ( -111.4739401608841121, -298.3618730044814242, -274.2696299215406839 ) ) ;
#35720 = CARTESIAN_POINT ( 'NONE',  ( -48.11685016983486918, -290.5071472515609230, -343.1114493814743014 ) ) ;
#35721 = CARTESIAN_POINT ( 'NONE',  ( -107.3007046392191199, -291.9214536950478305, -248.4107289403539482 ) ) ;
#35722 = ORIENTED_EDGE ( 'NONE', *, *, #43350, .F. ) ;
#35723 = CARTESIAN_POINT ( 'NONE',  ( -78.08775392017629713, -298.4597666689002153, -205.3028416987097842 ) ) ;
#35724 = VECTOR ( 'NONE', #16930, 1000.000000000000000 ) ;
#35725 = CARTESIAN_POINT ( 'NONE',  ( -14.55275688468293360, -286.8478771943365473, -200.8915419411851531 ) ) ;
#35726 = CARTESIAN_POINT ( 'NONE',  ( 38.20038889795292647, -294.5320232029475847, -284.4875671691122534 ) ) ;
#35727 = CARTESIAN_POINT ( 'NONE',  ( -88.55978787883272219, -296.2399624968351191, -327.8453971409397809 ) ) ;
#35728 = CARTESIAN_POINT ( 'NONE',  ( -2.441302814725339942, -292.6941719932141268, -206.2301367280074658 ) ) ;
#35729 = ORIENTED_EDGE ( 'NONE', *, *, #31528, .F. ) ;
#35730 = CARTESIAN_POINT ( 'NONE',  ( -3.229932089025133291, -276.4191939330307264, -202.9248745331114776 ) ) ;
#35731 = ORIENTED_EDGE ( 'NONE', *, *, #8208, .T. ) ;
#35732 = CARTESIAN_POINT ( 'NONE',  ( -101.8362077740213891, -278.6123068678450068, -228.3125459905606363 ) ) ;
#35733 = CARTESIAN_POINT ( 'NONE',  ( -16.39428891565522761, -272.7271574728490577, -199.5431013742716004 ) ) ;
#35734 = CARTESIAN_POINT ( 'NONE',  ( 9.229930784917645070, -299.8529804473018885, -196.9542415464881344 ) ) ;
#35735 = CARTESIAN_POINT ( 'NONE',  ( 25.58384586021559670, -277.0068504540777212, -307.8282250205483592 ) ) ;
#35736 = CARTESIAN_POINT ( 'NONE',  ( 4.288999983718310816, -276.3648587867934907, -206.7309499166615865 ) ) ;
#35737 = CARTESIAN_POINT ( 'NONE',  ( 34.90909198118203705, -273.8472112388758433, -291.8128951153929620 ) ) ;
#35738 = CARTESIAN_POINT ( 'NONE',  ( -109.4621264632441040, -297.0462940991317851, -282.2999945447016898 ) ) ;
#35739 = CARTESIAN_POINT ( 'NONE',  ( -28.84582845064091927, -293.5172005873548073, -343.5097043233968179 ) ) ;
#35740 = DIRECTION ( 'NONE',  ( -0.000000000000000000, -0.000000000000000000, -1.000000000000000000 ) ) ;
#35741 = CARTESIAN_POINT ( 'NONE',  ( -104.9185423907243830, -278.5681303172277126, -307.1428701550810842 ) ) ;
#35742 = CARTESIAN_POINT ( 'NONE',  ( -59.19297676218162962, -277.5096859653685897, -340.0139837811059351 ) ) ;
#35743 = CARTESIAN_POINT ( 'NONE',  ( 22.61592798916430525, -285.5967661822577384, -222.8178033497227943 ) ) ;
#35744 = CARTESIAN_POINT ( 'NONE',  ( -94.20140499135716539, -299.2332506711222209, -221.1203838538394564 ) ) ;
#35745 = CARTESIAN_POINT ( 'NONE',  ( 82.62000873716831961, -301.8234436266066041, -196.4228867002380809 ) ) ;
#35746 = CARTESIAN_POINT ( 'NONE',  ( 22.12880004312654236, -286.1540203084305176, -227.6627659026793822 ) ) ;
#35747 = EDGE_CURVE ( 'NONE', #30213, #34891, #73146, .T. ) ;
#35748 = CARTESIAN_POINT ( 'NONE',  ( -94.71198856607145444, -277.4448965557360793, -223.5997661955304352 ) ) ;
#35749 = CARTESIAN_POINT ( 'NONE',  ( -85.85915613411758329, -277.9390693801459520, -215.0309148531598851 ) ) ;
#35750 = CARTESIAN_POINT ( 'NONE',  ( -105.2776397533293817, -286.1332247496409309, -302.2579535769954191 ) ) ;
#35751 = CARTESIAN_POINT ( 'NONE',  ( -39.15225920570156859, -278.2804555294076749, -343.7358573806489517 ) ) ;
#35752 = DIRECTION ( 'NONE',  ( 0.000000000000000000, -1.000000000000000000, 0.000000000000000000 ) ) ;
#35753 = CARTESIAN_POINT ( 'NONE',  ( 38.83168960953429405, -273.9265756188825662, -268.3473877790993924 ) ) ;
#35754 = CARTESIAN_POINT ( 'NONE',  ( -4.065683449955379558, -275.1544247831729422, -205.2579013259077385 ) ) ;
#35755 = CARTESIAN_POINT ( 'NONE',  ( 21.42563208398200914, -282.9092808682374880, -223.4745883359465211 ) ) ;
#35756 = LINE ( 'NONE', #84984, #36817 ) ;
#35757 = CARTESIAN_POINT ( 'NONE',  ( 37.35819362320376769, -289.3263221075469573, -258.9067730182167679 ) ) ;
#35758 = CARTESIAN_POINT ( 'NONE',  ( 0.1016626691354874934, -292.5539616869652946, -335.4045937221521285 ) ) ;
#35759 = CARTESIAN_POINT ( 'NONE',  ( 140.6539576904058606, 275.0000000000000568, 11.50000000000000000 ) ) ;
#35760 = CARTESIAN_POINT ( 'NONE',  ( -16.48477909591456836, -273.0120659692967706, -199.8365492795474552 ) ) ;
#35761 = CARTESIAN_POINT ( 'NONE',  ( -27.92659694341521970, -290.3123838423521192, -196.6737761133524316 ) ) ;
#35762 = CARTESIAN_POINT ( 'NONE',  ( 198.4603912096053193, 279.4542985770845576, -127.2015713121144529 ) ) ;
#35763 = CARTESIAN_POINT ( 'NONE',  ( 113.5000000000000568, -296.0521521680024080, -400.5374811273811702 ) ) ;
#35764 = CARTESIAN_POINT ( 'NONE',  ( -67.79511929089275668, -287.9245270392905240, -340.3275171708549465 ) ) ;
#35765 = CARTESIAN_POINT ( 'NONE',  ( 6.971419010202898114, -284.8856750332267893, -208.5684967984578009 ) ) ;
#35766 = EDGE_CURVE ( 'NONE', #37280, #16726, #30578, .T. ) ;
#35767 = CARTESIAN_POINT ( 'NONE',  ( -2.130893058473325219, -284.0016689284511813, -334.9942056471790579 ) ) ;
#35768 = CARTESIAN_POINT ( 'NONE',  ( -103.1534602389561996, -284.9218810746347117, -302.4370002272187321 ) ) ;
#35769 = CARTESIAN_POINT ( 'NONE',  ( -104.5488301102956399, -292.9817149725633953, -236.1636130415934929 ) ) ;
#35770 = CARTESIAN_POINT ( 'NONE',  ( -95.07343119308772827, -273.5750843044803560, -219.4416568718659164 ) ) ;
#35771 = CARTESIAN_POINT ( 'NONE',  ( -97.89017324259570785, -288.0189680198514566, -315.5842550233263637 ) ) ;
#35772 = CARTESIAN_POINT ( 'NONE',  ( -35.71150949447974909, -277.0322640413725708, -347.3569829833591598 ) ) ;
#35773 = CARTESIAN_POINT ( 'NONE',  ( 36.33339277657601940, -295.3762979524936441, -258.2885446450802078 ) ) ;
#35774 = LINE ( 'NONE', #64687, #81691 ) ;
#35775 = CARTESIAN_POINT ( 'NONE',  ( -106.6662871844225293, -299.4805209788416391, -237.0123917617630980 ) ) ;
#35776 = CARTESIAN_POINT ( 'NONE',  ( -95.51701017061657240, -282.6087202723107339, -315.2913177761462293 ) ) ;
#35777 = CARTESIAN_POINT ( 'NONE',  ( -87.57258024323981260, -277.3507448689070998, -214.6667795891417825 ) ) ;
#35778 = CARTESIAN_POINT ( 'NONE',  ( -3.827864094035249298, -296.8649790477389274, -194.1700559458335817 ) ) ;
#35779 = CARTESIAN_POINT ( 'NONE',  ( 33.68359635123288598, -275.1293091870567764, -287.7141103081686424 ) ) ;
#35780 = CARTESIAN_POINT ( 'NONE',  ( 35.16186280490963867, -294.8990185131866610, -257.1023748630064460 ) ) ;
#35781 = CARTESIAN_POINT ( 'NONE',  ( 35.65993172397911337, -294.5702738797263578, -276.2066457257869843 ) ) ;
#35782 = CARTESIAN_POINT ( 'NONE',  ( -8.557931017036427335, -295.9985180532308959, -341.3030176357415826 ) ) ;
#35783 = CARTESIAN_POINT ( 'NONE',  ( -94.77475341973931222, -295.7500708638505102, -315.4215706449027721 ) ) ;
#35784 = CARTESIAN_POINT ( 'NONE',  ( -90.04898186073360478, -291.7971315190189330, -323.7178710680459517 ) ) ;
#35785 = CARTESIAN_POINT ( 'NONE',  ( -67.87940098858975091, -283.6087447183925292, -341.0466810819299326 ) ) ;
#35786 = CARTESIAN_POINT ( 'NONE',  ( -5.609662958338034855, -272.6046521313609787, -201.5615300403260903 ) ) ;
#35787 = CARTESIAN_POINT ( 'NONE',  ( 38.78589388530826199, -287.2398248088587707, -258.7152248779223100 ) ) ;
#35788 = CARTESIAN_POINT ( 'NONE',  ( -77.21355966776269497, -279.5689968616500209, -333.5256334986544857 ) ) ;
#35789 = CARTESIAN_POINT ( 'NONE',  ( -57.44751234073129353, -284.8450669311596926, -199.8870005509313330 ) ) ;
#35790 = CARTESIAN_POINT ( 'NONE',  ( -94.87370288003533858, -287.8870459161533972, -318.4962138518991424 ) ) ;
#35791 = CARTESIAN_POINT ( 'NONE',  ( 197.9737475143014365, 296.4634315385704895, -68.42128063630356394 ) ) ;
#35792 = CARTESIAN_POINT ( 'NONE',  ( -17.14885707722984520, -285.8274733178143947, -200.0925741636767157 ) ) ;
#35793 = CARTESIAN_POINT ( 'NONE',  ( 36.81131506836469924, -282.9990012263287440, -289.5793139696389744 ) ) ;
#35794 = CARTESIAN_POINT ( 'NONE',  ( -96.21833019228341755, -288.9457831250846880, -319.6396334000407364 ) ) ;
#35795 = CARTESIAN_POINT ( 'NONE',  ( -112.4514144652794840, -280.3145960139933095, -257.5170053841952722 ) ) ;
#35796 = CARTESIAN_POINT ( 'NONE',  ( -111.3461277529025750, -279.6222378719067478, -289.8198421680204433 ) ) ;
#35797 = CARTESIAN_POINT ( 'NONE',  ( -74.50396051839560130, -279.3766049704270245, -207.4701722827693118 ) ) ;
#35798 = CARTESIAN_POINT ( 'NONE',  ( -70.23804776299030550, -275.5963438220910007, -203.3560650445036799 ) ) ;
#35799 = CARTESIAN_POINT ( 'NONE',  ( 33.41656906309316355, -293.9404761935502393, -300.8646278004086412 ) ) ;
#35800 = CARTESIAN_POINT ( 'NONE',  ( -69.48867689414198878, -287.4974818992690189, -337.7289047352825264 ) ) ;
#35801 = CARTESIAN_POINT ( 'NONE',  ( -19.59309812983185140, -293.8766987957554875, -196.2027023095965887 ) ) ;
#35802 = CARTESIAN_POINT ( 'NONE',  ( -109.3466978557941758, -295.6541873522023138, -256.5281938818084768 ) ) ;
#35803 = CARTESIAN_POINT ( 'NONE',  ( 18.70485979573221869, -284.1577355837754340, -319.3519061008559561 ) ) ;
#35804 = CARTESIAN_POINT ( 'NONE',  ( -108.6134334162905191, -296.0093421270138379, -286.2490857875458232 ) ) ;
#35805 = CARTESIAN_POINT ( 'NONE',  ( 19.17851645802307559, -293.9237280147394245, -218.5252459732615478 ) ) ;
#35806 = CARTESIAN_POINT ( 'NONE',  ( -9.215783632738521192, -281.0812841903089634, -202.8864894940599584 ) ) ;
#35807 = CARTESIAN_POINT ( 'NONE',  ( 37.71786178296748204, -274.4082826995642108, -254.2091094770837572 ) ) ;
#35808 = CARTESIAN_POINT ( 'NONE',  ( -3.098661364161939602, -289.2631499489598355, -339.2286659032781699 ) ) ;
#35809 = CARTESIAN_POINT ( 'NONE',  ( -109.9314630807485571, -282.4144313842024303, -292.1094843333185054 ) ) ;
#35810 = CARTESIAN_POINT ( 'NONE',  ( -112.8464250445575772, -290.6970402503378637, -285.4206052511104303 ) ) ;
#35811 = CARTESIAN_POINT ( 'NONE',  ( 31.42073759807091093, -288.2125167344005376, -294.9337581478991979 ) ) ;
#35812 = LINE ( 'NONE', #6470, #64130 ) ;
#35813 = CARTESIAN_POINT ( 'NONE',  ( -72.17143339019004600, -195.1523444700580967, -358.2329797547330372 ) ) ;
#35814 = CARTESIAN_POINT ( 'NONE',  ( -12.49039970532447086, -92.45239924107487184, -356.2151309002171615 ) ) ;
#35815 = CARTESIAN_POINT ( 'NONE',  ( -85.33152481854864391, -275.1952119285918457, -330.4860931364850671 ) ) ;
#35816 = CARTESIAN_POINT ( 'NONE',  ( -98.12206922384847019, -278.3147700226716665, -229.5483537839099029 ) ) ;
#35817 = ORIENTED_EDGE ( 'NONE', *, *, #59917, .T. ) ;
#35818 = CARTESIAN_POINT ( 'NONE',  ( -2.992133447830128468, -279.4375672508744515, -205.5832059854104727 ) ) ;
#35819 = CARTESIAN_POINT ( 'NONE',  ( 34.70345811978169337, -274.8757322465228867, -243.2458185281324177 ) ) ;
#35820 = CARTESIAN_POINT ( 'NONE',  ( 204.1738562182569865, 292.3636489450777276, -53.99999999999267430 ) ) ;
#35821 = CARTESIAN_POINT ( 'NONE',  ( -74.70385637036221738, -278.1396314869719504, -203.7077191627982984 ) ) ;
#35822 = CARTESIAN_POINT ( 'NONE',  ( -97.25671647852421131, -281.9615904925966561, -314.8811990818225013 ) ) ;
#35823 = CARTESIAN_POINT ( 'NONE',  ( -104.3704482384691090, -298.7822565502026464, -234.4566871739443457 ) ) ;
#35824 = CARTESIAN_POINT ( 'NONE',  ( -85.97466090867335708, -291.8491154946696611, -215.7694116278451588 ) ) ;
#35825 = ORIENTED_EDGE ( 'NONE', *, *, #70691, .T. ) ;
#35826 = CARTESIAN_POINT ( 'NONE',  ( -100.7377745373110969, -288.7287360421577205, -307.6390872808646009 ) ) ;
#35827 = CARTESIAN_POINT ( 'NONE',  ( -46.87659259968729231, -274.5854986846861721, -194.0564745330433425 ) ) ;
#35828 = CARTESIAN_POINT ( 'NONE',  ( -109.1297112356303813, -272.7304682825526925, -256.8437820316009947 ) ) ;
#35829 = ORIENTED_EDGE ( 'NONE', *, *, #5207, .T. ) ;
#35830 = CARTESIAN_POINT ( 'NONE',  ( 154.4601611254703641, 20.78894139178057543, -13.92477262272432448 ) ) ;
#35831 = CARTESIAN_POINT ( 'NONE',  ( -47.94142310011969954, -281.8386345904721679, -195.4954448632993547 ) ) ;
#35832 = CARTESIAN_POINT ( 'NONE',  ( 139.6925840978351516, 15.36528803885690664, 22.50000000000000000 ) ) ;
#35833 = CARTESIAN_POINT ( 'NONE',  ( 33.02746530422345472, -282.3610835660103930, -249.8085845527403421 ) ) ;
#35834 = CARTESIAN_POINT ( 'NONE',  ( -50.78269387533965329, -281.6428450905522709, -195.5726583206794089 ) ) ;
#35835 = CARTESIAN_POINT ( 'NONE',  ( -108.5916475128085779, -283.8342606845941418, -253.3703990194199775 ) ) ;
#35836 = CARTESIAN_POINT ( 'NONE',  ( -109.1737112997808623, -280.6563994718788990, -251.5753916457361186 ) ) ;
#35837 = CARTESIAN_POINT ( 'NONE',  ( 35.53014415759140121, -273.8875264506598342, -259.3032789301449839 ) ) ;
#35838 = CARTESIAN_POINT ( 'NONE',  ( 145.2857639756989272, -299.5541904835127980, -189.7068768330456123 ) ) ;
#35839 = FACE_BOUND ( 'NONE', #59264, .T. ) ;
#35840 = CARTESIAN_POINT ( 'NONE',  ( -112.9049625825611542, -279.1793577268580862, -284.3743818936777075 ) ) ;
#35841 = EDGE_LOOP ( 'NONE', ( #35070, #13567, #18117, #24878 ) ) ;
#35842 = CARTESIAN_POINT ( 'NONE',  ( -84.51696442439769896, -276.2617199649768054, -330.5374356780156404 ) ) ;
#35843 = ORIENTED_EDGE ( 'NONE', *, *, #52765, .F. ) ;
#35844 = CARTESIAN_POINT ( 'NONE',  ( 180.6899167944524436, 8.542400036368780647, 13.00000000000000178 ) ) ;
#35845 = CARTESIAN_POINT ( 'NONE',  ( -110.2764947031228786, -286.2891552171987541, -289.3574583836836496 ) ) ;
#35846 = CARTESIAN_POINT ( 'NONE',  ( 28.88903878787332147, -292.3289665526837098, -239.1595139744169956 ) ) ;
#35847 = CARTESIAN_POINT ( 'NONE',  ( 23.20206595798455140, -287.5355122723147474, -317.7929195592660108 ) ) ;
#35848 = EDGE_CURVE ( 'NONE', #46065, #79497, #39841, .T. ) ;
#35849 = CARTESIAN_POINT ( 'NONE',  ( -30.41442431525060286, -284.3806684431287408, -196.6211690512395762 ) ) ;
#35851 = CARTESIAN_POINT ( 'NONE',  ( -94.90636749792419380, -288.1430436631787302, -316.8829739982963929 ) ) ;
#35850 = CARTESIAN_POINT ( 'NONE',  ( -109.3000335489130777, -282.9244779913994421, -285.8279545215975759 ) ) ;
#35852 = CARTESIAN_POINT ( 'NONE',  ( 35.53594366060141851, -282.8770397174846494, -279.4924914117164008 ) ) ;
#35853 = CARTESIAN_POINT ( 'NONE',  ( -52.12579010839287008, -271.8628675853944969, -196.7796558272020491 ) ) ;
#35854 = CARTESIAN_POINT ( 'NONE',  ( -105.0824008955871847, -282.4962667108395067, -305.3709732489545559 ) ) ;
#35855 = CARTESIAN_POINT ( 'NONE',  ( -109.6566811225870879, -298.2965337832521868, -290.2494103855281082 ) ) ;
#35856 = CARTESIAN_POINT ( 'NONE',  ( -109.1664589734814825, -282.8391623287386665, -248.0223609661307762 ) ) ;
#35857 = CARTESIAN_POINT ( 'NONE',  ( -99.36801492669393099, -278.9562932844493162, -309.3935241990178611 ) ) ;
#35858 = CARTESIAN_POINT ( 'NONE',  ( 36.74542958286263428, -289.3887213943446000, -257.5920177674213392 ) ) ;
#35859 = CARTESIAN_POINT ( 'NONE',  ( 193.4805262621761699, 275.8411434044543284, 16.89623125813409033 ) ) ;
#35860 = CARTESIAN_POINT ( 'NONE',  ( 175.2296996224750103, 250.0000000000000568, 0.000000000000000000 ) ) ;
#35861 = CARTESIAN_POINT ( 'NONE',  ( 12.46534283833557666, -296.2852212115566317, -327.2510415009658686 ) ) ;
#35862 = CARTESIAN_POINT ( 'NONE',  ( -110.1188386758993261, -276.3185844338349284, -288.5383938779753521 ) ) ;
#35863 = CARTESIAN_POINT ( 'NONE',  ( -106.3729476996660566, -289.3137027838367317, -304.2288814774816501 ) ) ;
#35864 = CARTESIAN_POINT ( 'NONE',  ( 14.86799095559641870, -292.7014616147563402, -322.5922116243596633 ) ) ;
#35865 = CARTESIAN_POINT ( 'NONE',  ( 0.6692559086183191841, -279.2548770556284126, -207.4021954739244507 ) ) ;
#35866 = CARTESIAN_POINT ( 'NONE',  ( -88.30162822418512292, -271.4119551560722812, -216.0282409862622046 ) ) ;
#35867 = CARTESIAN_POINT ( 'NONE',  ( -30.77950644801808977, -293.4520169201267095, -197.1615203598858841 ) ) ;
#35868 = CARTESIAN_POINT ( 'NONE',  ( -54.42813229853332757, -279.7662352645559736, -345.3683826091709648 ) ) ;
#35869 = CARTESIAN_POINT ( 'NONE',  ( 1.400589923602379328, -293.0241885309461622, -336.1010808217097292 ) ) ;
#35870 = CARTESIAN_POINT ( 'NONE',  ( -100.9836276131071600, -291.6435689623929193, -307.8267549743551399 ) ) ;
#35871 = CARTESIAN_POINT ( 'NONE',  ( 25.66538900130607459, -291.2238618999442679, -227.7940489043524224 ) ) ;
#35872 = EDGE_CURVE ( 'NONE', #88143, #5640, #587, .T. ) ;
#35873 = CARTESIAN_POINT ( 'NONE',  ( -71.42970933976185677, -290.9368117308164869, -335.5933148208285957 ) ) ;
#35874 = CARTESIAN_POINT ( 'NONE',  ( 160.5350683151633291, 215.0000000000000568, 20.22542485937379908 ) ) ;
#35875 = CARTESIAN_POINT ( 'NONE',  ( -73.61616102243436899, -290.3496054595977967, -333.9111032647531943 ) ) ;
#35876 = DIRECTION ( 'NONE',  ( 0.000000000000000000, 0.000000000000000000, -1.000000000000000000 ) ) ;
#35877 = CARTESIAN_POINT ( 'NONE',  ( -81.71293537649171412, -292.6676974693359625, -207.9175258363220564 ) ) ;
#35879 = CARTESIAN_POINT ( 'NONE',  ( -81.72904545615023153, -291.4286961341201732, -212.3423116172144489 ) ) ;
#35878 = CARTESIAN_POINT ( 'NONE',  ( 21.60479574164332561, -278.9298727412668768, -223.3968255557733755 ) ) ;
#35880 = CARTESIAN_POINT ( 'NONE',  ( -95.89248886396806881, -279.5598684884321301, -220.3653823007524863 ) ) ;
#35881 = CARTESIAN_POINT ( 'NONE',  ( 33.15528250359770368, -280.8244693569112087, -239.4431663804909647 ) ) ;
#35882 = CARTESIAN_POINT ( 'NONE',  ( 21.93665262005682237, -284.9221397388207038, -224.4146540452813667 ) ) ;
#35883 = CARTESIAN_POINT ( 'NONE',  ( 197.0195873853737965, 40.95756171125039202, 12.27312447568957232 ) ) ;
#35884 = CARTESIAN_POINT ( 'NONE',  ( 19.42382688510289768, -280.3602386447441290, -318.2195343636670941 ) ) ;
#35885 = CARTESIAN_POINT ( 'NONE',  ( -37.94024538081043119, -284.0444955579608290, -195.3635020417542307 ) ) ;
#35886 = CARTESIAN_POINT ( 'NONE',  ( 207.5150402071092799, 1.051285333831500024, 7.457902384259533335 ) ) ;
#35887 = CARTESIAN_POINT ( 'NONE',  ( -96.52899969924932577, -276.3797080960275707, -318.5435135066287557 ) ) ;
#35888 = CARTESIAN_POINT ( 'NONE',  ( -99.42289277995428165, -273.8880870927927731, -231.6503023657550386 ) ) ;
#35889 = CARTESIAN_POINT ( 'NONE',  ( 200.6103193995254230, 250.5000000000000568, -2.464576988612312114 ) ) ;
#35890 = CARTESIAN_POINT ( 'NONE',  ( -101.8325759346736419, -292.6387921538587875, -234.3762031830789851 ) ) ;
#35891 = CARTESIAN_POINT ( 'NONE',  ( -24.27833677943826274, -275.6409346657578681, -195.0215473671578366 ) ) ;
#35892 = CARTESIAN_POINT ( 'NONE',  ( -7.502893733694051548, -276.3165191749701535, -337.0074466121967021 ) ) ;
#35893 = CARTESIAN_POINT ( 'NONE',  ( 0.2664088270362876543, -296.5518716179108765, -335.3097752432576613 ) ) ;
#35894 = CARTESIAN_POINT ( 'NONE',  ( -43.18017833146507201, -289.2906359675313297, -347.1394494099674830 ) ) ;
#35895 = CARTESIAN_POINT ( 'NONE',  ( 20.87712562472719569, -278.9722352924721918, -222.1959591063992434 ) ) ;
#35896 = CARTESIAN_POINT ( 'NONE',  ( -42.05184177742446394, -291.8276416329142080, -193.5053142319234780 ) ) ;
#35897 = CARTESIAN_POINT ( 'NONE',  ( -109.9316994606314637, -289.7433907783371865, -260.2849011877294743 ) ) ;
#35898 = CARTESIAN_POINT ( 'NONE',  ( -2.908968490600246870, -292.5968778742449672, -336.9898478507655000 ) ) ;
#35899 = ORIENTED_EDGE ( 'NONE', *, *, #28273, .F. ) ;
#35900 = FACE_OUTER_BOUND ( 'NONE', #38229, .T. ) ;
#35901 = CARTESIAN_POINT ( 'NONE',  ( 2.279133542742972640, -292.1059960429151943, -208.9156975273704404 ) ) ;
#35902 = DIRECTION ( 'NONE',  ( 1.000000000000000000, 0.000000000000000000, 0.000000000000000000 ) ) ;
#35903 = CARTESIAN_POINT ( 'NONE',  ( -67.68488546085839630, -271.1237833571632905, -207.2794874003663779 ) ) ;
#35904 = CARTESIAN_POINT ( 'NONE',  ( -92.53618087868541409, -294.8778100336870693, -323.7126831653220052 ) ) ;
#35905 = CARTESIAN_POINT ( 'NONE',  ( -98.95710847973568036, -286.4747001422683752, -224.9215309864172241 ) ) ;
#35906 = CARTESIAN_POINT ( 'NONE',  ( 34.56777083021366792, -287.2158780779911353, -257.5050147388474784 ) ) ;
#35907 = CARTESIAN_POINT ( 'NONE',  ( 35.79665274808300524, -277.1955717858698449, -279.7960810334030270 ) ) ;
#35908 = CARTESIAN_POINT ( 'NONE',  ( 9.235256765963400838, -292.4293254916535147, -328.7579145080817966 ) ) ;
#35909 = CARTESIAN_POINT ( 'NONE',  ( 35.06351440005865072, -295.5127370837394096, -285.7666654754575006 ) ) ;
#35910 = CARTESIAN_POINT ( 'NONE',  ( -37.82770890019034482, -275.8532590699784919, -343.7691034773999377 ) ) ;
#35911 = ORIENTED_EDGE ( 'NONE', *, *, #45009, .F. ) ;
#35912 = CARTESIAN_POINT ( 'NONE',  ( 113.5000000000000568, -296.0521521680024080, -400.5374811273811702 ) ) ;
#35913 = CARTESIAN_POINT ( 'NONE',  ( -113.3679943625155175, -296.3709421736039076, -258.2050748188232774 ) ) ;
#35914 = CARTESIAN_POINT ( 'NONE',  ( -39.98504682171709845, -291.0056509608852480, -344.8047284580619589 ) ) ;
#35915 = CARTESIAN_POINT ( 'NONE',  ( 165.2494399300530290, -11.64849832608277325, -3.999999999999998224 ) ) ;
#35916 = CARTESIAN_POINT ( 'NONE',  ( -37.26774325382954345, -299.1327251845659134, -193.6694534736314779 ) ) ;
#35917 = CARTESIAN_POINT ( 'NONE',  ( 23.61448049025223028, -287.6433958573451832, -229.9180713994797145 ) ) ;
#35918 = EDGE_LOOP ( 'NONE', ( #71927, #49914, #83083, #5909 ) ) ;
#35919 = CARTESIAN_POINT ( 'NONE',  ( 15.00966031843823245, -279.8275142907165218, -214.1443839329539003 ) ) ;
#35920 = CARTESIAN_POINT ( 'NONE',  ( -74.54975851904841022, -296.1848026193763985, -337.7176519130306360 ) ) ;
#35921 = CARTESIAN_POINT ( 'NONE',  ( -36.13073356646869172, -287.1767450163325179, -346.1291438599660069 ) ) ;
#35922 = CARTESIAN_POINT ( 'NONE',  ( -69.51521488416017291, -295.7973987926621930, -340.3084376610596564 ) ) ;
#35923 = CARTESIAN_POINT ( 'NONE',  ( 22.60286574353643729, -293.3041532455619631, -228.6409289324111285 ) ) ;
#35924 = CARTESIAN_POINT ( 'NONE',  ( 199.0345205062965590, 66.35750757917867304, -8.036855303410847640 ) ) ;
#35925 = FILL_AREA_STYLE_COLOUR ( '', #49228 ) ;
#35926 = CARTESIAN_POINT ( 'NONE',  ( 0.000000000000000000, 0.000000000000000000, 22.50000000000000000 ) ) ;
#35927 = CARTESIAN_POINT ( 'NONE',  ( 36.83505127818909131, -289.2988652670415490, -288.3193737197967152 ) ) ;
#35928 = CARTESIAN_POINT ( 'NONE',  ( -88.52914483777347243, -287.1952119285918457, -334.4957818155094174 ) ) ;
#35929 = CARTESIAN_POINT ( 'NONE',  ( -77.43228425001780124, -278.8782056059986871, -204.6789177783452089 ) ) ;
#35930 = CARTESIAN_POINT ( 'NONE',  ( -5.223540613919172237, -284.6287268044742405, -337.9655420994542965 ) ) ;
#35931 = CARTESIAN_POINT ( 'NONE',  ( -113.5626383055736426, -283.2035593823263753, -264.2769435574415979 ) ) ;
#35932 = CARTESIAN_POINT ( 'NONE',  ( 32.74716778369376158, -285.9594446539716159, -295.4382946877983045 ) ) ;
#35933 = CARTESIAN_POINT ( 'NONE',  ( 38.38990711771787545, -277.4583277372731231, -273.9612593269754370 ) ) ;
#35934 = CARTESIAN_POINT ( 'NONE',  ( -29.99195762371079610, -274.4810204064551158, -197.7107995257357516 ) ) ;
#35935 = ORIENTED_EDGE ( 'NONE', *, *, #46451, .T. ) ;
#35936 = CARTESIAN_POINT ( 'NONE',  ( -41.08095014715326698, -293.7849822740155901, -343.7717365995626437 ) ) ;
#35938 = CARTESIAN_POINT ( 'NONE',  ( -110.2706850432613237, -277.8254170273582986, -276.0786069709569119 ) ) ;
#35937 = CARTESIAN_POINT ( 'NONE',  ( -107.8202617599682611, -278.3009134815028460, -289.3814321308679496 ) ) ;
#35939 = CARTESIAN_POINT ( 'NONE',  ( 37.33076981444173725, -276.4116857576322559, -252.8250571644439901 ) ) ;
#35940 = CARTESIAN_POINT ( 'NONE',  ( -112.8425207458116830, -277.5098449731387404, -257.4137319488613116 ) ) ;
#35941 = CARTESIAN_POINT ( 'NONE',  ( -57.32492746522063243, -168.5919582920984965, -361.8708629427547407 ) ) ;
#35942 = EDGE_CURVE ( 'NONE', #5341, #90630, #8114, .T. ) ;
#35943 = CARTESIAN_POINT ( 'NONE',  ( -109.3021001887156416, -298.3042791699436407, -244.6646762997305018 ) ) ;
#35944 = CARTESIAN_POINT ( 'NONE',  ( -20.19161114001083490, -279.3376638359844719, -345.3538533559490702 ) ) ;
#35945 = VERTEX_POINT ( 'NONE', #44578 ) ;
#35946 = CARTESIAN_POINT ( 'NONE',  ( 82.64534425881677748, -299.8335964094648034, -192.8708706794661509 ) ) ;
#35947 = CARTESIAN_POINT ( 'NONE',  ( -91.75987617780724293, -286.3330092501024637, -221.1653526072449552 ) ) ;
#35948 = CARTESIAN_POINT ( 'NONE',  ( -18.45584352790105243, -288.0522069390998467, -196.7044456223308089 ) ) ;
#35949 = CARTESIAN_POINT ( 'NONE',  ( 35.55285048385430002, -286.9815796920115645, -276.4981385649771823 ) ) ;
#35950 = CARTESIAN_POINT ( 'NONE',  ( -97.52833812884441045, -284.7020046198523460, -222.4330937194190483 ) ) ;
#35951 = CARTESIAN_POINT ( 'NONE',  ( 27.16790575827264931, -279.4672489902299048, -234.5149025364347040 ) ) ;
#35952 = CARTESIAN_POINT ( 'NONE',  ( 17.79237646302278364, -288.7123910101200863, -220.6319972394503850 ) ) ;
#35953 = CARTESIAN_POINT ( 'NONE',  ( -7.702995656680331926, -278.9276765446437025, -202.8769132350293205 ) ) ;
#35954 = CARTESIAN_POINT ( 'NONE',  ( -66.98632753178294763, -278.7642342872966310, -337.6102038145389201 ) ) ;
#35955 = CARTESIAN_POINT ( 'NONE',  ( 34.18029930946099881, -275.8470486854521369, -255.3805479684553745 ) ) ;
#35956 = CARTESIAN_POINT ( 'NONE',  ( 20.26411540205024764, -287.0339640099466010, -320.8742275618199074 ) ) ;
#35957 = CARTESIAN_POINT ( 'NONE',  ( -50.05669831860699759, -284.0131449892352293, -346.1940824747232455 ) ) ;
#35958 = CARTESIAN_POINT ( 'NONE',  ( 26.67416482063226724, -282.6067064476460473, -313.0401050614949554 ) ) ;
#35959 = ORIENTED_EDGE ( 'NONE', *, *, #87554, .F. ) ;
#35960 = VERTEX_POINT ( 'NONE', #93383 ) ;
#35961 = CARTESIAN_POINT ( 'NONE',  ( 207.7755975652984830, 28.53818587417392294, 12.00000000000000000 ) ) ;
#35962 = CARTESIAN_POINT ( 'NONE',  ( -37.47524285369376429, -290.9141804616032232, -346.1386665567623595 ) ) ;
#35963 = CARTESIAN_POINT ( 'NONE',  ( -113.3258391799145954, -289.1190904959850059, -279.7271718684771145 ) ) ;
#35964 = CARTESIAN_POINT ( 'NONE',  ( -96.46424865163734808, -272.2151832899973556, -227.0572939716278995 ) ) ;
#35965 = CARTESIAN_POINT ( 'NONE',  ( 34.37077811291285911, -292.5469449500603787, -242.4536423903509501 ) ) ;
#35966 = CARTESIAN_POINT ( 'NONE',  ( -110.4799782128428092, -288.9140540002245530, -279.3888547370207220 ) ) ;
#35967 = CARTESIAN_POINT ( 'NONE',  ( 31.78268359051463676, -291.4435557515766391, -243.9075059910906305 ) ) ;
#35968 = CARTESIAN_POINT ( 'NONE',  ( 23.08548225642544338, -289.3345534916576298, -312.0448444051788783 ) ) ;
#35969 = CARTESIAN_POINT ( 'NONE',  ( -4.771743288812468897, -297.1233781216987495, -337.9199732462171255 ) ) ;
#35970 = CARTESIAN_POINT ( 'NONE',  ( 15.30079172572841983, -290.3092396135111812, -323.8540385873101854 ) ) ;
#35971 = CARTESIAN_POINT ( 'NONE',  ( -50.22644223858247869, -289.8878837468391225, -196.3070036835548819 ) ) ;
#35972 = CARTESIAN_POINT ( 'NONE',  ( 2.113205009760168451, -294.5801435537571251, -206.5176132412560719 ) ) ;
#35973 = CARTESIAN_POINT ( 'NONE',  ( -107.2067417246463066, -285.2032612896694559, -292.3220927090198415 ) ) ;
#35974 = CARTESIAN_POINT ( 'NONE',  ( -17.14431014670264375, -294.3124661091924281, -197.9588123442455867 ) ) ;
#35975 = CARTESIAN_POINT ( 'NONE',  ( 197.1844320129423807, 70.43964897667966341, -15.08154681515735085 ) ) ;
#35976 = CARTESIAN_POINT ( 'NONE',  ( 180.7287904564219332, 250.0000000000000568, -24.90000000000002345 ) ) ;
#35977 = CARTESIAN_POINT ( 'NONE',  ( -112.2309057073502743, -274.6389754008060891, -261.9936996624375638 ) ) ;
#35978 = CARTESIAN_POINT ( 'NONE',  ( 35.86426593198129353, -280.7620156665488480, -271.3260681264384857 ) ) ;
#35979 = CARTESIAN_POINT ( 'NONE',  ( -100.7347939852731145, -282.0118106665311757, -310.5372700994254842 ) ) ;
#35980 = CARTESIAN_POINT ( 'NONE',  ( -69.46973829306152481, -294.6614688339735721, -340.1748627454306870 ) ) ;
#35981 = CARTESIAN_POINT ( 'NONE',  ( -16.33184127520627271, -272.5671703946092066, -199.3389479500310983 ) ) ;
#35982 = CARTESIAN_POINT ( 'NONE',  ( -86.06589630116212675, -275.8131726462228244, -326.7078955979637840 ) ) ;
#35983 = CARTESIAN_POINT ( 'NONE',  ( -107.9377117754009134, -298.1357512147263833, -249.9296075600573772 ) ) ;
#35984 = CARTESIAN_POINT ( 'NONE',  ( -5.268421674030641100, -296.0468539821069385, -336.6070564659072488 ) ) ;
#35985 = DIRECTION ( 'NONE',  ( 0.000000000000000000, 0.000000000000000000, 1.000000000000000000 ) ) ;
#35986 = CARTESIAN_POINT ( 'NONE',  ( 14.43777369014532930, -295.1040353204406870, -322.1187978897140738 ) ) ;
#35987 = CARTESIAN_POINT ( 'NONE',  ( 187.8995604928813918, 43.86402690510830382, 15.00000000000000000 ) ) ;
#35989 = CARTESIAN_POINT ( 'NONE',  ( -100.1664722097354172, -296.0401386917951072, -307.6365571505736511 ) ) ;
#35988 = CARTESIAN_POINT ( 'NONE',  ( -0.4979073383079692383, -284.5593644069957122, -204.6125189248627976 ) ) ;
#35990 = CARTESIAN_POINT ( 'NONE',  ( -93.43153693400074644, -283.8319477712225876, -323.1339330929971538 ) ) ;
#35991 = AXIS2_PLACEMENT_3D ( 'NONE', #16573, #59692, #74328 ) ;
#35992 = CARTESIAN_POINT ( 'NONE',  ( 35.83026231740477385, -286.9160724351013414, -246.2822878044025003 ) ) ;
#35993 = CARTESIAN_POINT ( 'NONE',  ( -61.04964880909157898, -297.3381486891323675, -341.9442544535156685 ) ) ;
#35994 = CARTESIAN_POINT ( 'NONE',  ( 23.30507938420539915, -290.9534921414048085, -226.4987368238243448 ) ) ;
#35995 = CARTESIAN_POINT ( 'NONE',  ( -107.2679199732858990, -278.1587454728679631, -238.3821078083812495 ) ) ;
#35996 = CARTESIAN_POINT ( 'NONE',  ( 31.95455697924147387, -285.4809262143061801, -303.7686719486574134 ) ) ;
#35997 = DIRECTION ( 'NONE',  ( -1.000000000000000000, -0.000000000000000000, -0.000000000000000000 ) ) ;
#35998 = CARTESIAN_POINT ( 'NONE',  ( 0.3858672293007937570, -285.3614245582684248, -207.3434506458920623 ) ) ;
#35999 = EDGE_CURVE ( 'NONE', #1988, #52326, #63050, .T. ) ;
#36000 = CARTESIAN_POINT ( 'NONE',  ( 198.9494509394918396, 68.47434140769267685, -9.196269295805851840 ) ) ;
#36001 = FACE_OUTER_BOUND ( 'NONE', #18232, .T. ) ;
#36002 = CARTESIAN_POINT ( 'NONE',  ( -108.7384034567929518, -297.9077319520077936, -289.0912630905892797 ) ) ;
#36003 = CARTESIAN_POINT ( 'NONE',  ( -33.95965310423532202, -281.5191842455809592, -194.0252283119619392 ) ) ;
#36005 = CARTESIAN_POINT ( 'NONE',  ( -16.13250130004695748, -282.7701389099767653, -340.2121729858519075 ) ) ;
#36004 = CARTESIAN_POINT ( 'NONE',  ( -99.38186327574641155, -295.1495617136193914, -227.5666745904416928 ) ) ;
#36006 = CARTESIAN_POINT ( 'NONE',  ( -113.1394902320587619, -296.8883355883930335, -256.8077043951365113 ) ) ;
#36007 = CARTESIAN_POINT ( 'NONE',  ( -63.34203998585009998, -299.2274142097465983, -201.3528631349783211 ) ) ;
#36008 = CARTESIAN_POINT ( 'NONE',  ( 36.88036766833413083, -285.4515845579388724, -256.2048878173302455 ) ) ;
#36009 = ADVANCED_FACE ( 'NONE', ( #36094 ), #114, .F. ) ;
#36010 = CARTESIAN_POINT ( 'NONE',  ( -109.4223383124809317, -280.8190351025744462, -249.6395772778710977 ) ) ;
#36011 = CARTESIAN_POINT ( 'NONE',  ( -65.65264073796910793, -296.7313028557964572, -202.8192858317003981 ) ) ;
#36012 = EDGE_LOOP ( 'NONE', ( #86330, #63469, #6944 ) ) ;
#36013 = DIRECTION ( 'NONE',  ( -0.3024135303179394940, -0.9531768234072001134, 0.000000000000000000 ) ) ;
#36014 = CARTESIAN_POINT ( 'NONE',  ( -90.03799071820556321, -285.7805930399254635, -323.3009071382941784 ) ) ;
#36015 = CARTESIAN_POINT ( 'NONE',  ( 156.4851178187871312, 1.000000000000000000, 7.000000000000000000 ) ) ;
#36016 = CARTESIAN_POINT ( 'NONE',  ( -85.28047601435909542, -282.9094976428775681, -210.1954327657594206 ) ) ;
#36017 = CARTESIAN_POINT ( 'NONE',  ( 29.81139469213858817, -274.2629953692501203, -232.9070604222078202 ) ) ;
#36018 = CARTESIAN_POINT ( 'NONE',  ( 30.82914868770197714, -293.0367602763806190, -244.2510552437138927 ) ) ;
#36019 = CARTESIAN_POINT ( 'NONE',  ( 35.71755542012938633, -282.9412769274255197, -260.3360734027672265 ) ) ;
#36021 = CARTESIAN_POINT ( 'NONE',  ( 14.30559291453952220, -277.9119945697760841, -323.1485080595585941 ) ) ;
#36020 = PRODUCT_RELATED_PRODUCT_CATEGORY ( 'part', '', ( #44255 ) ) ;
#36022 = CARTESIAN_POINT ( 'NONE',  ( -49.94095544460658687, -284.8103124484644013, -345.5656071417282078 ) ) ;
#36023 = CARTESIAN_POINT ( 'NONE',  ( 25.89337390959351026, -280.8573242301625328, -307.7235039038418449 ) ) ;
#36024 = CARTESIAN_POINT ( 'NONE',  ( -103.9433420287878107, -281.0100932150013477, -235.7629195286055790 ) ) ;
#36025 = CARTESIAN_POINT ( 'NONE',  ( -76.43455178122212601, -273.7114879240963319, -203.9613669617654068 ) ) ;
#36026 = CARTESIAN_POINT ( 'NONE',  ( 37.28575135553037256, -275.1481372145277078, -251.3942128689417643 ) ) ;
#36027 = CARTESIAN_POINT ( 'NONE',  ( 34.00229101283765232, -295.1945003886354471, -248.9387161770248156 ) ) ;
#36028 = DIRECTION ( 'NONE',  ( 0.000000000000000000, -0.000000000000000000, -1.000000000000000000 ) ) ;
#36029 = DIRECTION ( 'NONE',  ( 1.000000000000000000, 0.000000000000000000, 0.000000000000000000 ) ) ;
#36030 = CARTESIAN_POINT ( 'NONE',  ( 24.68951602234481868, -292.2766482646951545, -313.8858616748576651 ) ) ;
#36031 = AXIS2_PLACEMENT_3D ( 'NONE', #44042, #28928, #15183 ) ;
#36032 = CARTESIAN_POINT ( 'NONE',  ( 11.59238728939789986, -274.2605113655901050, -216.0394790837535766 ) ) ;
#36033 = CARTESIAN_POINT ( 'NONE',  ( -25.15144851101744194, -293.7250088159098027, -195.0344592441111047 ) ) ;
#36035 = CARTESIAN_POINT ( 'NONE',  ( -11.30273312026978516, -293.5889631587131703, -198.2638520161769407 ) ) ;
#36034 = CARTESIAN_POINT ( 'NONE',  ( 21.31550574532285580, -284.6948066931273615, -317.0979686699210447 ) ) ;
#36036 = CARTESIAN_POINT ( 'NONE',  ( -76.81469423215196457, -291.5822160145771136, -333.9371446128778871 ) ) ;
#36037 = CARTESIAN_POINT ( 'NONE',  ( -108.9748653721970157, -276.8316147081663985, -248.7112204203098997 ) ) ;
#36038 = CARTESIAN_POINT ( 'NONE',  ( -93.80320085285353571, -279.7949379966387937, -318.8731075945761404 ) ) ;
#36039 = CARTESIAN_POINT ( 'NONE',  ( -28.75365586934023554, -293.0223985715033450, -344.3560854813433707 ) ) ;
#36040 = CARTESIAN_POINT ( 'NONE',  ( 38.47427313575620644, -283.4068803728491730, -269.9135330446234207 ) ) ;
#36041 = CARTESIAN_POINT ( 'NONE',  ( -13.44152678679741086, -281.6548426100673055, -339.7186813489938118 ) ) ;
#36042 = EDGE_LOOP ( 'NONE', ( #34779, #43065, #77126, #64284 ) ) ;
#36043 = CARTESIAN_POINT ( 'NONE',  ( 9.919151263593899870, -282.0469650887955595, -326.0917758862202618 ) ) ;
#36044 = CARTESIAN_POINT ( 'NONE',  ( -38.18037391631578714, -281.1215382646490752, -193.6748145284742009 ) ) ;
#36045 = CARTESIAN_POINT ( 'NONE',  ( -110.3120082757571794, -283.0520183596102015, -293.7141185224048172 ) ) ;
#36046 = CARTESIAN_POINT ( 'NONE',  ( -112.2521607238216035, -279.2830203613024764, -287.1314223183925378 ) ) ;
#36047 = CARTESIAN_POINT ( 'NONE',  ( -82.12360743858742751, -279.1708348516762612, -332.1453273622139477 ) ) ;
#36048 = CARTESIAN_POINT ( 'NONE',  ( -105.5795714935544112, -298.8376638359844719, -285.9686137636504668 ) ) ;
#36049 = VERTEX_POINT ( 'NONE', #57882 ) ;
#36050 = EDGE_LOOP ( 'NONE', ( #8235, #79842, #37979, #3189 ) ) ;
#36051 = CARTESIAN_POINT ( 'NONE',  ( -89.53538278272077378, -299.3172587367963615, -216.4293233262237663 ) ) ;
#36052 = CARTESIAN_POINT ( 'NONE',  ( -94.88986917784711750, -275.9130159801692344, -317.9211897202442287 ) ) ;
#36053 = CARTESIAN_POINT ( 'NONE',  ( -58.67593673882629446, -293.5400804007318811, -197.4308474503789057 ) ) ;
#36054 = CARTESIAN_POINT ( 'NONE',  ( 35.72347447959032962, -292.8701997590976589, -268.0431603906367855 ) ) ;
#36055 = CARTESIAN_POINT ( 'NONE',  ( -34.67523727084896734, -288.5271409076464693, -347.2533599789834398 ) ) ;
#36056 = CARTESIAN_POINT ( 'NONE',  ( 185.4166944662832179, 249.5000000000000568, 23.37680765314684095 ) ) ;
#36058 = CARTESIAN_POINT ( 'NONE',  ( 7.428238399418281901, -285.0737673624904573, -211.6271832805844610 ) ) ;
#36057 = CARTESIAN_POINT ( 'NONE',  ( 22.69733833132485756, -292.7640681905851352, -317.6464692267282430 ) ) ;
#36059 = CARTESIAN_POINT ( 'NONE',  ( -95.26940642525214287, -293.0579227246906839, -223.9162803048484989 ) ) ;
#36060 = CARTESIAN_POINT ( 'NONE',  ( -39.97953290717646979, -284.4982838564886833, -196.7150074804497990 ) ) ;
#36061 = CARTESIAN_POINT ( 'NONE',  ( 21.41418920589967456, -283.4832875887590831, -314.5292747608009449 ) ) ;
#36062 = CARTESIAN_POINT ( 'NONE',  ( -38.90333493461796621, -290.0125429811660638, -347.1099388892132538 ) ) ;
#36063 = CARTESIAN_POINT ( 'NONE',  ( -24.87204739732126058, -280.7078826319194604, -198.3715617798361563 ) ) ;
#36064 = CARTESIAN_POINT ( 'NONE',  ( 29.22199726182032364, -292.8431909825834509, -308.3797495876948460 ) ) ;
#36065 = CARTESIAN_POINT ( 'NONE',  ( -6.974314153894478174, -289.4665338820295233, -340.9584765960046866 ) ) ;
#36066 = CARTESIAN_POINT ( 'NONE',  ( -65.41871858278739182, -289.9017306944202232, -342.0498639999348143 ) ) ;
#36067 = CARTESIAN_POINT ( 'NONE',  ( -105.5656866611570024, -285.0655859301717214, -244.3902176126077563 ) ) ;
#36068 = ORIENTED_EDGE ( 'NONE', *, *, #54005, .F. ) ;
#36069 = CARTESIAN_POINT ( 'NONE',  ( 195.0378959947337592, 25.05079320569620904, 13.55224814914091525 ) ) ;
#36070 = CARTESIAN_POINT ( 'NONE',  ( -14.13745576728970477, -296.6147329282335932, -342.4850981996587507 ) ) ;
#36071 = CARTESIAN_POINT ( 'NONE',  ( -81.60015338384043559, -294.3251199883722506, -332.8316626668808453 ) ) ;
#36072 = CARTESIAN_POINT ( 'NONE',  ( -98.18241759816103809, -278.1763729420327422, -229.5057189560954782 ) ) ;
#36073 = CARTESIAN_POINT ( 'NONE',  ( -101.1539947238558455, -272.6276161224485008, -227.2835178636804585 ) ) ;
#36074 = CARTESIAN_POINT ( 'NONE',  ( -82.80259452368517259, -294.1662509362652713, -328.4263195235254784 ) ) ;
#36075 = CARTESIAN_POINT ( 'NONE',  ( 30.08654156860731632, -277.7179808264780263, -300.8800667299840370 ) ) ;
#36076 = CARTESIAN_POINT ( 'NONE',  ( -92.92759666765854831, -271.3830875816646540, -221.1567118011929267 ) ) ;
#36077 = CARTESIAN_POINT ( 'NONE',  ( 14.60811261049018306, -295.5062136478746879, -322.2818715579534796 ) ) ;
#36078 = CARTESIAN_POINT ( 'NONE',  ( -103.0390978787870750, -297.1913692566685654, -303.0039009459678141 ) ) ;
#36079 = CARTESIAN_POINT ( 'NONE',  ( -43.52509054635434183, -249.8758584012454946, -454.3901068140907000 ) ) ;
#36080 = CARTESIAN_POINT ( 'NONE',  ( -95.11896568555668807, -293.8893466703573836, -318.4624883155148609 ) ) ;
#36081 = CARTESIAN_POINT ( 'NONE',  ( -35.48331144383948299, -298.7262563450054813, -193.4628507519142033 ) ) ;
#36082 = CARTESIAN_POINT ( 'NONE',  ( -82.28943665980462185, -275.4394140254975127, -210.2567668775636776 ) ) ;
#36083 = CARTESIAN_POINT ( 'NONE',  ( -107.1728276478716424, -291.1998071498833838, -292.5973368350095143 ) ) ;
#36084 = CARTESIAN_POINT ( 'NONE',  ( -5.528460655804314783, -294.9550397425869619, -336.1016801320116656 ) ) ;
#36085 = CARTESIAN_POINT ( 'NONE',  ( -104.8601920155234097, -280.0912315486333455, -303.9397612074504877 ) ) ;
#36086 = CARTESIAN_POINT ( 'NONE',  ( -79.62419890423167601, -278.1789125132446543, -206.5363926290765164 ) ) ;
#36087 = CARTESIAN_POINT ( 'NONE',  ( -37.32261616562219331, -282.4004734249032822, -347.2722309324539083 ) ) ;
#36088 = CARTESIAN_POINT ( 'NONE',  ( 38.63372606223966699, -275.0536505971246015, -282.5714272009927299 ) ) ;
#36089 = CARTESIAN_POINT ( 'NONE',  ( -98.77073766801068189, -277.5573952300843530, -225.2512589974267314 ) ) ;
#36090 = CARTESIAN_POINT ( 'NONE',  ( -1.974970567337443805, -278.5192938369738727, -204.0344802787012100 ) ) ;
#36091 = CARTESIAN_POINT ( 'NONE',  ( -107.7550556810145110, -271.4098443262947171, -248.8013328842553449 ) ) ;
#36092 = CARTESIAN_POINT ( 'NONE',  ( 14.83968657196227170, -278.3174682628719552, -324.3036662464737105 ) ) ;
#36093 = CIRCLE ( 'NONE', #37563, 4.999999999999997335 ) ;
#36094 = FACE_OUTER_BOUND ( 'NONE', #32737, .T. ) ;
#36095 = CARTESIAN_POINT ( 'NONE',  ( 35.83096562836566790, -291.3421151222876233, -252.3564576761066007 ) ) ;
#36096 = CARTESIAN_POINT ( 'NONE',  ( -104.6099768869517987, -291.0379081191270529, -232.8914109928861649 ) ) ;
#36097 = CARTESIAN_POINT ( 'NONE',  ( 22.16545967015004592, -276.9242011598900035, -224.4171277122600543 ) ) ;
#36098 = CARTESIAN_POINT ( 'NONE',  ( -112.3407520386660252, -270.5882458039783387, -267.5372233972520917 ) ) ;
#36099 = CARTESIAN_POINT ( 'NONE',  ( -67.11703004482465929, -284.8687720866598738, -199.5261792228695867 ) ) ;
#36100 = PRESENTATION_STYLE_ASSIGNMENT (( #27134 ) ) ;
#36101 = CARTESIAN_POINT ( 'NONE',  ( -111.2706959294984443, -282.7151187825085685, -257.6564226164061324 ) ) ;
#36102 =( BOUNDED_SURFACE ( )  B_SPLINE_SURFACE ( 3, 2, ( 
 ( #2752, #83203, #3690 ),
 ( #89359, #25450, #11711 ),
 ( #53873, #10769, #4153 ),
 ( #46284, #75188, #90298 ),
 ( #33023, #24516, #40564 ),
 ( #18350, #32092, #53397 ) ),
 .UNSPECIFIED., .F., .F., .F. ) 
 B_SPLINE_SURFACE_WITH_KNOTS ( ( 4, 2, 4 ),
 ( 3, 3 ),
 ( 0.000000000000000000, 0.2633701841259441512, 0.5267403682518883024 ),
 ( 0.000000000000000000, 1.000000000000000000 ),
 .UNSPECIFIED. ) 
 GEOMETRIC_REPRESENTATION_ITEM ( )  RATIONAL_B_SPLINE_SURFACE ( (
 ( 1.000000000000000000, 0.9475641245298915827, 1.000000000000000000),
 ( 1.000000000000000000, 0.9475658968925606551, 1.000000000000000000),
 ( 1.000000000000000000, 0.9451322790880675173, 1.000000000000000000),
 ( 1.000000000000000000, 0.9354614375526318915, 1.000000000000000000),
 ( 1.000000000000000000, 0.9282241625909629645, 1.000000000000000000),
 ( 1.000000000000000000, 0.9186651033962672797, 1.000000000000000000) ) ) 
 REPRESENTATION_ITEM ( '' )  SURFACE ( )  );
#36103 = CARTESIAN_POINT ( 'NONE',  ( 175.2296996224750103, 150.9142415853029036, 0.000000000000000000 ) ) ;
#36104 = CARTESIAN_POINT ( 'NONE',  ( 33.01409034714732371, -292.0697750463023112, -249.2766881751722110 ) ) ;
#36105 = CARTESIAN_POINT ( 'NONE',  ( -72.94596188093042599, -283.7147452805493799, -205.2067978766801275 ) ) ;
#36106 = DIRECTION ( 'NONE',  ( -1.000000000000000000, 0.000000000000000000, 0.000000000000000000 ) ) ;
#36107 = CARTESIAN_POINT ( 'NONE',  ( 159.4851178187871312, 14.99999999999999467, -9.000000000000001776 ) ) ;
#36108 = CARTESIAN_POINT ( 'NONE',  ( 34.55341498742018302, -291.2748186305441891, -248.8256107140244069 ) ) ;
#36109 = CARTESIAN_POINT ( 'NONE',  ( -103.8225608363302968, -282.5403751060389936, -307.9248652838684848 ) ) ;
#36110 = CARTESIAN_POINT ( 'NONE',  ( -109.5432677627753861, -279.9529435662199148, -285.6377029558079812 ) ) ;
#36111 = CARTESIAN_POINT ( 'NONE',  ( -111.8294181819885580, -285.5317876106329891, -288.2936401661785908 ) ) ;
#36112 = CARTESIAN_POINT ( 'NONE',  ( 0.1686625972033692078, -286.5663059486057591, -207.6765310297049894 ) ) ;
#36113 =( BOUNDED_CURVE ( )  B_SPLINE_CURVE ( 3, ( #41160, #34571, #26530, #6162 ),
 .UNSPECIFIED., .F., .F. ) 
 B_SPLINE_CURVE_WITH_KNOTS ( ( 4, 4 ),
 ( 1.570796326794895004, 2.004620063563922638 ),
 .UNSPECIFIED. ) 
 CURVE ( )  GEOMETRIC_REPRESENTATION_ITEM ( )  RATIONAL_B_SPLINE_CURVE ( ( 1.000000000000000000, 0.9843778111405747655, 0.9843778111405747655, 1.000000000000000000 ) ) 
 REPRESENTATION_ITEM ( '' )  );
#36114 = CARTESIAN_POINT ( 'NONE',  ( -103.6541636890630684, -279.5477988865100087, -302.3855822783746703 ) ) ;
#36115 = CARTESIAN_POINT ( 'NONE',  ( -104.4153484784346375, -278.9614671629792042, -299.7066355650611627 ) ) ;
#36116 = CARTESIAN_POINT ( 'NONE',  ( -13.25386239782711151, -288.3433976551850719, -198.9595572518784934 ) ) ;
#36117 = EDGE_LOOP ( 'NONE', ( #61801, #48868, #37538, #71657 ) ) ;
#36118 = CARTESIAN_POINT ( 'NONE',  ( -43.28763838203731495, -297.8124832326483897, -193.5378236265038652 ) ) ;
#36119 = CARTESIAN_POINT ( 'NONE',  ( 9.020825600810162825, -290.3921225341840113, -328.8620838514359548 ) ) ;
#36120 = DIRECTION ( 'NONE',  ( -1.000000000000000000, -0.000000000000000000, -0.000000000000000000 ) ) ;
#36121 = CARTESIAN_POINT ( 'NONE',  ( -55.63300648810263738, -282.3376638359844151, -190.3683826091709363 ) ) ;
#36122 = ORIENTED_EDGE ( 'NONE', *, *, #12195, .T. ) ;
#36123 = CARTESIAN_POINT ( 'NONE',  ( 38.64485042180249508, -291.8799963969167948, -264.6615961247072732 ) ) ;
#36124 = CARTESIAN_POINT ( 'NONE',  ( -1.869488593554387679, -288.0507938011772353, -205.7095203647421329 ) ) ;
#36125 = CARTESIAN_POINT ( 'NONE',  ( -34.29372919938526820, -281.8511042219344063, -196.3978499006769312 ) ) ;
#36126 = CARTESIAN_POINT ( 'NONE',  ( 2.885484765620438985, -289.9491557817245848, -335.3876467558663990 ) ) ;
#36127 = CARTESIAN_POINT ( 'NONE',  ( -12.36877165450719041, -290.0492890485820112, -342.7329635065437401 ) ) ;
#36128 = CARTESIAN_POINT ( 'NONE',  ( -62.17351888655193193, -285.3750885767565819, -341.1857236781678466 ) ) ;
#36129 = CARTESIAN_POINT ( 'NONE',  ( -112.7179820969497825, -278.9163410485656414, -254.5680578233979645 ) ) ;
#36130 = EDGE_LOOP ( 'NONE', ( #28487, #92464, #83435, #3421, #67289, #77404 ) ) ;
#36131 = CARTESIAN_POINT ( 'NONE',  ( 22.02481473602728457, -292.2692665478901972, -317.1251156490727681 ) ) ;
#36132 = CARTESIAN_POINT ( 'NONE',  ( 37.33177405566786433, -281.1504378322624120, -251.5762235762069565 ) ) ;
#36133 = CARTESIAN_POINT ( 'NONE',  ( -21.69642338203885146, -276.1152528934460975, -197.7932821805744936 ) ) ;
#36134 = CARTESIAN_POINT ( 'NONE',  ( 202.1700622694972083, 300.2031883395015939, -5.006794249105121608 ) ) ;
#36135 = CARTESIAN_POINT ( 'NONE',  ( -85.33152481854864391, -287.9090924074130839, -210.2361428286349110 ) ) ;
#36136 = CARTESIAN_POINT ( 'NONE',  ( 8.911505652960718393, -272.9167885492464620, -210.0733500168014700 ) ) ;
#36137 = CYLINDRICAL_SURFACE ( 'NONE', #86365, 26.04691768583011680 ) ;
#36138 = CARTESIAN_POINT ( 'NONE',  ( -11.71569465512919628, -279.9025552876253187, -201.8876143152286318 ) ) ;
#36139 = CARTESIAN_POINT ( 'NONE',  ( 33.34120471936005714, -276.3781914395808599, -240.6956267869684893 ) ) ;
#36140 = CARTESIAN_POINT ( 'NONE',  ( -55.45612375885657741, -299.2398894230291262, -198.9834729463937322 ) ) ;
#36141 = CARTESIAN_POINT ( 'NONE',  ( -34.49971972426728684, -282.0759994322939406, -347.0731989144782688 ) ) ;
#36142 = CARTESIAN_POINT ( 'NONE',  ( -99.15806731602999946, -292.8701305757792852, -229.5652703128246515 ) ) ;
#36143 = CARTESIAN_POINT ( 'NONE',  ( -100.5564026171813765, -274.7197541196087514, -227.7190330620076111 ) ) ;
#36144 = CARTESIAN_POINT ( 'NONE',  ( -104.9106396670619574, -298.2272803921481454, -234.1591187536167809 ) ) ;
#36145 = CARTESIAN_POINT ( 'NONE',  ( -23.14671990896060549, -296.8704908393681308, -343.8887171170696320 ) ) ;
#36146 = CARTESIAN_POINT ( 'NONE',  ( -62.16633697422399507, -281.3754123317987705, -341.0114909284214377 ) ) ;
#36147 = CARTESIAN_POINT ( 'NONE',  ( -100.0113666966936421, -290.8111178333703606, -225.6592479574994172 ) ) ;
#36148 = CARTESIAN_POINT ( 'NONE',  ( -5.811794039078424845, -272.4888846436464860, -202.7023282460580447 ) ) ;
#36149 = CARTESIAN_POINT ( 'NONE',  ( 26.45670808654967843, -288.5990953131250194, -228.6933423732967299 ) ) ;
#36150 = CARTESIAN_POINT ( 'NONE',  ( -102.6788527408748024, -289.9234544646740801, -237.0029979799479065 ) ) ;
#36151 = ORIENTED_EDGE ( 'NONE', *, *, #81715, .F. ) ;
#36152 = CARTESIAN_POINT ( 'NONE',  ( -84.81292382985320444, -288.2664684170431428, -330.3042528901302148 ) ) ;
#36153 = CARTESIAN_POINT ( 'NONE',  ( -45.36898666447230255, -288.8233762748753293, -342.9396971751189653 ) ) ;
#36154 = ORIENTED_EDGE ( 'NONE', *, *, #17632, .F. ) ;
#36155 = CARTESIAN_POINT ( 'NONE',  ( -85.33023056062818057, -286.4861905406572760, -210.5397718275824275 ) ) ;
#36156 = CARTESIAN_POINT ( 'NONE',  ( -80.82857180994611213, -277.9943416018773519, -329.0209805634548843 ) ) ;
#36157 = CARTESIAN_POINT ( 'NONE',  ( 37.47930206118654439, -292.6845838309280907, -287.2521649463952826 ) ) ;
#36158 = CARTESIAN_POINT ( 'NONE',  ( -79.09740938484608819, -284.2510563865067752, -334.9349016014886047 ) ) ;
#36159 = CARTESIAN_POINT ( 'NONE',  ( -2.898492634936535861, -282.9427750701872810, -339.2191386595620202 ) ) ;
#36161 = CARTESIAN_POINT ( 'NONE',  ( 2.712037078011438229, -280.9387457910447097, -209.2448531990257266 ) ) ;
#36160 = VECTOR ( 'NONE', #53688, 1000.000000000000227 ) ;
#36162 = CARTESIAN_POINT ( 'NONE',  ( 203.9604463576624198, 295.7236918480278405, -68.68622640684732517 ) ) ;
#36163 = CARTESIAN_POINT ( 'NONE',  ( -114.3576317657223171, -272.4623070776191867, -284.0502682576448592 ) ) ;
#36164 = CARTESIAN_POINT ( 'NONE',  ( 120.1367009602576843, 148.5113953528500588, -260.6353423530172790 ) ) ;
#36165 = CARTESIAN_POINT ( 'NONE',  ( -99.41208178824524566, -272.2826807188951648, -231.6329699845104813 ) ) ;
#36166 = CARTESIAN_POINT ( 'NONE',  ( 7.530922440670147822, -273.6013850210127885, -212.3897990701607057 ) ) ;
#36167 = CARTESIAN_POINT ( 'NONE',  ( 1.732776325546617091, -294.0517974865024939, -336.6386571122970963 ) ) ;
#36168 = CARTESIAN_POINT ( 'NONE',  ( 199.8274843008227322, 285.7222973586868306, -96.42357284835115649 ) ) ;
#36169 = EDGE_CURVE ( 'NONE', #25231, #69141, #33804, .T. ) ;
#36170 = CARTESIAN_POINT ( 'NONE',  ( -94.70555265768811637, -271.9268954147405566, -219.7381321319227254 ) ) ;
#36171 = CARTESIAN_POINT ( 'NONE',  ( -58.27540603824840559, -299.6391313150692781, -199.1386114633301361 ) ) ;
#36172 = ADVANCED_FACE ( 'NONE', ( #15717 ), #44105, .F. ) ;
#36173 = CARTESIAN_POINT ( 'NONE',  ( 36.04398846671895029, -288.8041319961679392, -265.5377609561448367 ) ) ;
#36174 = VERTEX_POINT ( 'NONE', #73010 ) ;
#36175 = CARTESIAN_POINT ( 'NONE',  ( -86.23620346047437124, -296.6529416620409734, -329.5400648823112419 ) ) ;
#36176 = CARTESIAN_POINT ( 'NONE',  ( -71.21231322094249094, -286.0846060671940450, -205.6249610798599292 ) ) ;
#36177 = CARTESIAN_POINT ( 'NONE',  ( -110.7372606567545148, -271.7548341422327667, -247.9404482524247726 ) ) ;
#36178 = CARTESIAN_POINT ( 'NONE',  ( 25.58829341018716974, -294.9394667676555741, -314.4746136519703441 ) ) ;
#36179 = CARTESIAN_POINT ( 'NONE',  ( -94.60158123103721550, -296.3464978079836101, -321.7697798333427386 ) ) ;
#36180 = CARTESIAN_POINT ( 'NONE',  ( -110.3678558490410921, -290.7438610845713356, -268.4638771025769870 ) ) ;
#36181 = ORIENTED_EDGE ( 'NONE', *, *, #8683, .T. ) ;
#36182 = CARTESIAN_POINT ( 'NONE',  ( -93.09948816549784567, -275.1792242776418220, -219.3480538221003542 ) ) ;
#36183 = CARTESIAN_POINT ( 'NONE',  ( 31.49171079292095143, -274.7823020051932872, -304.0969182757463045 ) ) ;
#36184 = EDGE_LOOP ( 'NONE', ( #41872, #21049, #75414, #88913 ) ) ;
#36185 = CARTESIAN_POINT ( 'NONE',  ( -107.5225470536054218, -277.6553342928883126, -302.0213302858275028 ) ) ;
#36186 = CARTESIAN_POINT ( 'NONE',  ( 17.89776309050611758, -273.2596508508046895, -221.3462019362630713 ) ) ;
#36187 = CARTESIAN_POINT ( 'NONE',  ( -91.35957232452396681, -274.3402643619718333, -220.7815026719439118 ) ) ;
#36188 = CARTESIAN_POINT ( 'NONE',  ( 0.7245659950945282368, -275.5146720957750404, -207.7962090360141758 ) ) ;
#36189 = CARTESIAN_POINT ( 'NONE',  ( -5.558798911149763100, -276.2246234912205409, -201.3406774805418138 ) ) ;
#36190 = CARTESIAN_POINT ( 'NONE',  ( 33.64288830939032238, -273.9001936931389878, -295.8049895631006621 ) ) ;
#36191 = CARTESIAN_POINT ( 'NONE',  ( -101.5529013551746402, -296.7273134833705512, -305.3012711713106455 ) ) ;
#36192 = CARTESIAN_POINT ( 'NONE',  ( 35.41778759416050804, -292.2754084186418027, -281.7116495838174046 ) ) ;
#36193 = CARTESIAN_POINT ( 'NONE',  ( 156.4851178187871312, 0.000000000000000000, 7.000000000000000000 ) ) ;
#36194 = CARTESIAN_POINT ( 'NONE',  ( -114.3232277504436922, -279.0288211952927213, -271.6136572608987763 ) ) ;
#36195 = CARTESIAN_POINT ( 'NONE',  ( -56.59812814241952594, -277.4739243381552569, -340.8280314783614813 ) ) ;
#36196 = CARTESIAN_POINT ( 'NONE',  ( -21.07240359344990210, -284.9415278765324047, -195.6041232483434271 ) ) ;
#36197 = CARTESIAN_POINT ( 'NONE',  ( -107.1945446413967602, -298.9146376392331490, -242.4612867527767435 ) ) ;
#36198 = FACE_OUTER_BOUND ( 'NONE', #40803, .T. ) ;
#36199 = CARTESIAN_POINT ( 'NONE',  ( 33.54756173344362935, -286.5104435205909681, -252.2186946920048740 ) ) ;
#36200 = CARTESIAN_POINT ( 'NONE',  ( -67.23217062761143836, -275.6894162747487371, -338.0703033919854192 ) ) ;
#36201 = CARTESIAN_POINT ( 'NONE',  ( -71.94719444666444019, -276.0937830790541057, -335.3201917227514173 ) ) ;
#36202 = CARTESIAN_POINT ( 'NONE',  ( -85.08664083924865906, -285.7108983820560297, -328.2672327651857245 ) ) ;
#36203 = CARTESIAN_POINT ( 'NONE',  ( 20.34401482185246479, -277.3941091419751501, -315.7629543829226009 ) ) ;
#36204 = EDGE_CURVE ( 'NONE', #13726, #3915, #25777, .T. ) ;
#36205 = CARTESIAN_POINT ( 'NONE',  ( 155.7140808774799723, 21.00000000000000000, 15.62500000000000000 ) ) ;
#36206 = CARTESIAN_POINT ( 'NONE',  ( 37.94210523876643038, -274.1050885672996174, -282.4726022670672592 ) ) ;
#36207 = CARTESIAN_POINT ( 'NONE',  ( 19.93019163537890748, -275.5629893314053334, -224.9117720082027745 ) ) ;
#36208 = CARTESIAN_POINT ( 'NONE',  ( -85.64652553884448594, -281.3861835362627062, -212.7026992079060221 ) ) ;
#36209 = DIRECTION ( 'NONE',  ( 0.000000000000000000, 1.000000000000000000, 0.000000000000000000 ) ) ;
#36210 = CARTESIAN_POINT ( 'NONE',  ( 36.11047487907135434, -289.6988326202091457, -288.1384983865893332 ) ) ;
#36211 = CARTESIAN_POINT ( 'NONE',  ( 8.979508819043772405, -290.6871085107884483, -211.3098595550771961 ) ) ;
#36212 = DIRECTION ( 'NONE',  ( -0.000000000000000000, -0.000000000000000000, 1.000000000000000000 ) ) ;
#36213 = CARTESIAN_POINT ( 'NONE',  ( -40.51988780746840746, -296.8062553152834084, -197.0202687202381355 ) ) ;
#36214 = CARTESIAN_POINT ( 'NONE',  ( -107.7351817500601499, -288.9995936178340230, -246.7894565015827482 ) ) ;
#36215 = CARTESIAN_POINT ( 'NONE',  ( 126.6218730542261568, 145.9178657400643431, -262.1768218896158373 ) ) ;
#36216 = DIRECTION ( 'NONE',  ( -0.8660254037844404840, 0.000000000000000000, -0.4999999999999968359 ) ) ;
#36217 = CARTESIAN_POINT ( 'NONE',  ( -45.96680493742259443, -287.6393777948164256, -346.2314120663837684 ) ) ;
#36218 = CARTESIAN_POINT ( 'NONE',  ( -36.55313339357986990, -284.3017864267904997, -194.3656720424375521 ) ) ;
#36219 = CARTESIAN_POINT ( 'NONE',  ( -92.09138181866777018, -285.2790877378170649, -319.5516840566954215 ) ) ;
#36220 = CARTESIAN_POINT ( 'NONE',  ( -108.8248672537759916, -285.5608388698738054, -254.7218818756450958 ) ) ;
#36221 = CARTESIAN_POINT ( 'NONE',  ( -67.68998171193675262, -293.6358269726344474, -201.3732299545440299 ) ) ;
#36222 = CIRCLE ( 'NONE', #70980, 7.500000000000012434 ) ;
#36223 = CARTESIAN_POINT ( 'NONE',  ( -15.78734953429887788, -274.6567307449877831, -196.4061723616887036 ) ) ;
#36224 = CARTESIAN_POINT ( 'NONE',  ( -102.5679607563286453, -288.1249453047005886, -308.6071487640248847 ) ) ;
#36225 = CARTESIAN_POINT ( 'NONE',  ( -75.33619964256796209, -277.5442842848946157, -337.3343813541747522 ) ) ;
#36227 = CARTESIAN_POINT ( 'NONE',  ( 21.84241173838362471, -296.1582889395841676, -315.8692799580741735 ) ) ;
#36226 = VECTOR ( 'NONE', #78272, 1000.000000000000000 ) ;
#36228 = CARTESIAN_POINT ( 'NONE',  ( -74.94434090351494149, -277.8906705383787994, 25.50000000000000000 ) ) ;
#36229 = CARTESIAN_POINT ( 'NONE',  ( 31.95455697924148097, -295.6233781216988632, -236.9535640164627637 ) ) ;
#36230 = CARTESIAN_POINT ( 'NONE',  ( -102.2143595042586384, -282.7682134834214480, -305.0061453710436581 ) ) ;
#36231 = CARTESIAN_POINT ( 'NONE',  ( -58.70737429970168364, -277.7756543135695324, -198.4687775456655743 ) ) ;
#36232 = CARTESIAN_POINT ( 'NONE',  ( -111.1426760980806421, -271.2793402925843225, -250.7651741823665930 ) ) ;
#36233 = CARTESIAN_POINT ( 'NONE',  ( 29.24370265665852031, -275.3068144968546562, -300.5319118705396022 ) ) ;
#36234 = CARTESIAN_POINT ( 'NONE',  ( 4.885234301560047676, -294.1539758710568435, -209.9032628039611836 ) ) ;
#36235 = CARTESIAN_POINT ( 'NONE',  ( 34.71252335331385552, -294.3202420795350349, -257.1919305607589763 ) ) ;
#36236 = CARTESIAN_POINT ( 'NONE',  ( 39.12197166903187906, -294.9765553017186903, -270.2922338149988377 ) ) ;
#36237 = CARTESIAN_POINT ( 'NONE',  ( 29.15439281089968304, -295.3630349436596134, -308.3042450659706333 ) ) ;
#36238 = CARTESIAN_POINT ( 'NONE',  ( -73.30425303103517365, -295.3767318592470588, -333.8882365478965539 ) ) ;
#36239 = CARTESIAN_POINT ( 'NONE',  ( -109.6473059386526074, -292.2938767804967028, -290.4746084014727785 ) ) ;
#36240 = CARTESIAN_POINT ( 'NONE',  ( -110.2239978041050108, -284.4058160186900750, -295.2040383013028304 ) ) ;
#36241 = CARTESIAN_POINT ( 'NONE',  ( -67.02945677763784715, -271.8067254603124638, -200.6550021296810087 ) ) ;
#36242 = CARTESIAN_POINT ( 'NONE',  ( 34.85496684569687176, -287.0470206597084939, -243.5909614202414559 ) ) ;
#36243 = CARTESIAN_POINT ( 'NONE',  ( -109.4016682721986058, -280.2804856558169604, -289.8343764701360215 ) ) ;
#36244 = CARTESIAN_POINT ( 'NONE',  ( 9.189192824204345911, -285.7684638311361596, -213.8077409972586338 ) ) ;
#36245 = CARTESIAN_POINT ( 'NONE',  ( -62.12737906677441657, -287.3741381016166656, -341.2021366259628508 ) ) ;
#36246 = CARTESIAN_POINT ( 'NONE',  ( -111.5035148913391652, -276.8895736657335078, -254.7960457309725371 ) ) ;
#36247 = CARTESIAN_POINT ( 'NONE',  ( 64.33209501061345748, 48.33985520751024723, -319.1928417150128325 ) ) ;
#36248 = CARTESIAN_POINT ( 'NONE',  ( -105.2734661674978582, -283.6987165151049908, -297.3924250609644560 ) ) ;
#36249 = CARTESIAN_POINT ( 'NONE',  ( 1.161046873152622005, -281.7589742732415630, -204.0772676821704295 ) ) ;
#36250 = CARTESIAN_POINT ( 'NONE',  ( -59.96938899550903557, -288.3971639252766295, -343.7151083917140681 ) ) ;
#36251 = CARTESIAN_POINT ( 'NONE',  ( -108.8624574460518062, -280.4897720851660665, -243.9175747877524145 ) ) ;
#36252 = CARTESIAN_POINT ( 'NONE',  ( -112.5775939159673413, -279.6916163650565181, -284.3203642132336313 ) ) ;
#36253 = CARTESIAN_POINT ( 'NONE',  ( -69.73838228804767425, -279.4466036330701399, -204.9297293615757383 ) ) ;
#36254 = CARTESIAN_POINT ( 'NONE',  ( 6.114281093487582197, -276.6245297572546633, -209.6060260265964530 ) ) ;
#36255 = CARTESIAN_POINT ( 'NONE',  ( 37.08258354717888494, -293.3043273409497260, -250.5611721048423988 ) ) ;
#36256 = CARTESIAN_POINT ( 'NONE',  ( 35.29596897621665619, -285.7940883196065442, -287.5546002946338717 ) ) ;
#36257 = CARTESIAN_POINT ( 'NONE',  ( -92.24991617180027959, -292.8838006630689961, -217.4511133676278405 ) ) ;
#36258 = CARTESIAN_POINT ( 'NONE',  ( -106.2825595604194007, -295.1400436662619313, -295.4380356678344697 ) ) ;
#36259 = CARTESIAN_POINT ( 'NONE',  ( -0.5188315579235495134, -284.4788311169131134, -335.0557124160932290 ) ) ;
#36260 = CARTESIAN_POINT ( 'NONE',  ( 18.84664950873154865, -293.8801406550237516, -316.9975506500848610 ) ) ;
#36261 = CARTESIAN_POINT ( 'NONE',  ( -72.04473842588902244, -292.6838126011361396, -201.9565796498543193 ) ) ;
#36262 = CARTESIAN_POINT ( 'NONE',  ( 32.07077971309043107, -281.8976896403491423, -247.2712957346687688 ) ) ;
#36263 = EDGE_CURVE ( 'NONE', #51665, #85436, #67053, .T. ) ;
#36264 = CARTESIAN_POINT ( 'NONE',  ( -106.6256940145609349, -272.0359502076033777, -237.3073980192059764 ) ) ;
#36265 = CARTESIAN_POINT ( 'NONE',  ( -103.7062565986324074, -290.6960984426877417, -309.3130227035121607 ) ) ;
#36266 = CARTESIAN_POINT ( 'NONE',  ( -107.0992998114111430, -282.3077402035950172, -300.0620126838579154 ) ) ;
#36267 = CARTESIAN_POINT ( 'NONE',  ( -98.14029470744488037, -290.2547026373045469, -317.5763188062454674 ) ) ;
#36268 = CARTESIAN_POINT ( 'NONE',  ( -8.250422995209902410, -286.7772066954727848, -203.3851142079568319 ) ) ;
#36269 = CARTESIAN_POINT ( 'NONE',  ( 188.7149167944524493, -12.49482340714361506, -3.999999999999998224 ) ) ;
#36270 = CARTESIAN_POINT ( 'NONE',  ( 4.125645570873484047, -58.01712834443207356, -352.5247458089312431 ) ) ;
#36271 = CARTESIAN_POINT ( 'NONE',  ( -12.70371226548575372, -92.33704762566186730, -356.1934519075916796 ) ) ;
#36272 = CARTESIAN_POINT ( 'NONE',  ( -59.77344130751080797, -278.9512946298843303, -200.6699299088105306 ) ) ;
#36273 = CARTESIAN_POINT ( 'NONE',  ( -41.05314201354045878, -278.9246709703813281, -197.1460152149548435 ) ) ;
#36274 = CARTESIAN_POINT ( 'NONE',  ( 32.53565102784897078, -274.8041662142536552, -237.9402023170395921 ) ) ;
#36275 = CARTESIAN_POINT ( 'NONE',  ( -75.47108427777141060, -209.2092562841938559, -354.8108879202522985 ) ) ;
#36276 = EDGE_CURVE ( 'NONE', #64125, #2981, #61150, .T. ) ;
#36277 = CARTESIAN_POINT ( 'NONE',  ( -73.47089559995228569, -278.1572115865279216, -203.0165905177013883 ) ) ;
#36278 = CARTESIAN_POINT ( 'NONE',  ( -96.43365694755391360, -281.9441096443633228, -315.9888705991562574 ) ) ;
#36279 = CARTESIAN_POINT ( 'NONE',  ( -83.55097043383059940, -297.4358457569019833, -330.7488938313445601 ) ) ;
#36280 = CARTESIAN_POINT ( 'NONE',  ( -83.87304728066754933, -291.8850398026606285, -214.0333080337985621 ) ) ;
#36281 = CARTESIAN_POINT ( 'NONE',  ( -74.98277038719879783, -288.2496345354257983, -333.4979566671272551 ) ) ;
#36282 = CARTESIAN_POINT ( 'NONE',  ( -58.10208276912891279, -274.4422983883305278, -196.2630790804410594 ) ) ;
#36283 = CARTESIAN_POINT ( 'NONE',  ( -109.0460719088370922, -296.9003372973874662, -256.6020868879635941 ) ) ;
#36284 = ORIENTED_EDGE ( 'NONE', *, *, #75213, .F. ) ;
#36285 = DIRECTION ( 'NONE',  ( 0.000000000000000000, 0.000000000000000000, 1.000000000000000000 ) ) ;
#36286 = CARTESIAN_POINT ( 'NONE',  ( 196.6762265213135947, 24.45209518732023568, 12.85352576531901292 ) ) ;
#36287 = CARTESIAN_POINT ( 'NONE',  ( -112.2920192408740263, -280.5994772802668535, -260.3827359774746810 ) ) ;
#36288 = CARTESIAN_POINT ( 'NONE',  ( 28.05093371741104846, -282.1824570015787117, -237.1120719176228135 ) ) ;
#36289 = CARTESIAN_POINT ( 'NONE',  ( -6.660348339466530376, -282.2095739967647319, -200.8299252269443400 ) ) ;
#36290 = CIRCLE ( 'NONE', #18177, 7.500000000000013323 ) ;
#36291 = CARTESIAN_POINT ( 'NONE',  ( 19.52718689039347666, -281.2619335770755242, -316.5256332902911254 ) ) ;
#36292 = CARTESIAN_POINT ( 'NONE',  ( -82.05036154857259589, -281.2961159945497798, -211.0344171992517204 ) ) ;
#36293 = CARTESIAN_POINT ( 'NONE',  ( -2.569570151768911792, -273.0007637543885721, -205.3872252979172117 ) ) ;
#36294 = CARTESIAN_POINT ( 'NONE',  ( 208.4784300167292201, 27.68468858954510736, 14.12814564770236991 ) ) ;
#36295 = FACE_OUTER_BOUND ( 'NONE', #50091, .T. ) ;
#36296 = CARTESIAN_POINT ( 'NONE',  ( 23.39670155592854073, -276.9849378309200461, -317.4463042332989176 ) ) ;
#36297 = CARTESIAN_POINT ( 'NONE',  ( 185.4166944662832179, 215.0000000000000568, 23.37680765314684095 ) ) ;
#36298 = CARTESIAN_POINT ( 'NONE',  ( 32.33589937920237389, -277.9153491264229388, -298.2507209485288513 ) ) ;
#36299 = CARTESIAN_POINT ( 'NONE',  ( -14.78112057482514352, -275.3402855213526550, -343.4208032984566330 ) ) ;
#36300 = ORIENTED_EDGE ( 'NONE', *, *, #53136, .T. ) ;
#36301 = DIRECTION ( 'NONE',  ( 1.000000000000000000, 0.000000000000000000, 0.000000000000000000 ) ) ;
#36302 = CARTESIAN_POINT ( 'NONE',  ( -58.01086106323934644, -285.2976270958839677, -342.8805384401403558 ) ) ;
#36303 = CARTESIAN_POINT ( 'NONE',  ( 14.99816214458775754, -292.0106829026373134, -219.1696597901038501 ) ) ;
#36304 = CARTESIAN_POINT ( 'NONE',  ( 37.92544965862923334, -286.7026646452790715, -254.5439495920884951 ) ) ;
#36305 = CARTESIAN_POINT ( 'NONE',  ( -108.7445966686949390, -282.5375701906197605, -289.8923581134595793 ) ) ;
#36307 = CARTESIAN_POINT ( 'NONE',  ( -5.154285822760023450, -284.5589061960181425, -203.2256437759452012 ) ) ;
#36306 = CARTESIAN_POINT ( 'NONE',  ( -36.20246861896865909, -281.6123175184255274, -343.9415302566496280 ) ) ;
#36308 = CARTESIAN_POINT ( 'NONE',  ( 3.624500841363582637, -283.6928452341866773, -331.3233504130445226 ) ) ;
#36309 = CARTESIAN_POINT ( 'NONE',  ( 32.85893579925581776, -273.2091214645902255, -243.9627967802626358 ) ) ;
#36310 = CARTESIAN_POINT ( 'NONE',  ( -104.7151389405291013, -283.4177850857029171, -234.6495996259006347 ) ) ;
#36311 = CARTESIAN_POINT ( 'NONE',  ( -33.51083836963886853, -297.0041143780780999, -345.2760001670768020 ) ) ;
#36312 = CARTESIAN_POINT ( 'NONE',  ( -103.7989916403977446, -283.0178173581813894, -235.1291395622011464 ) ) ;
#36313 = CARTESIAN_POINT ( 'NONE',  ( -102.3703112844064123, -279.9513551358339782, -236.5655819975815461 ) ) ;
#36314 = ADVANCED_FACE ( 'NONE', ( #60207 ), #82882, .F. ) ;
#36315 = CARTESIAN_POINT ( 'NONE',  ( 35.59164309125711867, -289.3192266991597990, -252.1744229241828634 ) ) ;
#36316 = DIRECTION ( 'NONE',  ( 0.000000000000000000, 0.000000000000000000, 1.000000000000000000 ) ) ;
#36317 = EDGE_CURVE ( 'NONE', #38347, #68325, #65603, .T. ) ;
#36318 = PLANE ( 'NONE',  #73123 ) ;
#36319 = CARTESIAN_POINT ( 'NONE',  ( 38.21512075694161581, -295.4354221114915049, -267.4669025318149806 ) ) ;
#36320 = CARTESIAN_POINT ( 'NONE',  ( -57.15233001207183605, -275.3074325462387719, -342.7513550718061310 ) ) ;
#36321 = CARTESIAN_POINT ( 'NONE',  ( -97.17080362110569070, -289.1014366118644716, -318.5963624766644102 ) ) ;
#36322 = CARTESIAN_POINT ( 'NONE',  ( -7.685326729214589037, -293.0567239932221923, -337.9539803973815424 ) ) ;
#36323 = CARTESIAN_POINT ( 'NONE',  ( -110.8438349787734438, -277.2695470187993010, -267.8749848083858183 ) ) ;
#36324 = CARTESIAN_POINT ( 'NONE',  ( -80.42599838442818339, -295.6008569065406277, -209.9077580954645157 ) ) ;
#36325 = CARTESIAN_POINT ( 'NONE',  ( -69.24673890687128619, -292.9386211861154834, -204.1406347487781545 ) ) ;
#36326 = CARTESIAN_POINT ( 'NONE',  ( -95.95921662488163406, -280.4090924074130839, -317.1477375740089997 ) ) ;
#36327 = CARTESIAN_POINT ( 'NONE',  ( -67.96585304046065801, -293.9268371757372051, -340.2529559365293608 ) ) ;
#36328 = CARTESIAN_POINT ( 'NONE',  ( -96.39636366464982586, -291.5374628736277032, -314.6426468297410679 ) ) ;
#36329 = CARTESIAN_POINT ( 'NONE',  ( -97.53165900483173800, -289.4194283210287040, -223.9596579359920270 ) ) ;
#36330 = CARTESIAN_POINT ( 'NONE',  ( -23.65794943948747431, -290.2992700861602771, -342.7190446257720282 ) ) ;
#36331 = PLANE ( 'NONE',  #80424 ) ;
#36332 = CARTESIAN_POINT ( 'NONE',  ( -90.70354437180714058, -290.6356243643067501, -320.4862157060960044 ) ) ;
#36333 = FACE_OUTER_BOUND ( 'NONE', #40669, .T. ) ;
#36334 = CARTESIAN_POINT ( 'NONE',  ( 7.713428883546115777, -289.6576352789380167, -332.3784887220405722 ) ) ;
#36335 = CARTESIAN_POINT ( 'NONE',  ( -45.07886518987283608, -277.9748772883688730, -195.3523184816838238 ) ) ;
#36336 = CARTESIAN_POINT ( 'NONE',  ( -112.0664190169488137, -279.1174459378747770, -251.8148457990174052 ) ) ;
#36337 = CARTESIAN_POINT ( 'NONE',  ( 39.61968665131914236, -281.1776067918901276, -267.0625175803532443 ) ) ;
#36338 = CARTESIAN_POINT ( 'NONE',  ( 17.45259208004352303, -284.8347823806874430, -219.1309666521230213 ) ) ;
#36339 = LINE ( 'NONE', #14120, #92808 ) ;
#36340 = CARTESIAN_POINT ( 'NONE',  ( 34.65931849064713077, -279.4565546235372153, -252.2340400334468598 ) ) ;
#36341 = CARTESIAN_POINT ( 'NONE',  ( -46.24221349494202116, -283.9390585771792530, -195.8911138921568238 ) ) ;
#36342 = DIRECTION ( 'NONE',  ( 0.000000000000000000, 0.000000000000000000, -1.000000000000000000 ) ) ;
#36343 = CARTESIAN_POINT ( 'NONE',  ( -112.5498342827859375, -277.1948496265815152, -257.4597881898287710 ) ) ;
#36344 = ADVANCED_FACE ( 'NONE', ( #81947 ), #2442, .F. ) ;
#36345 = CARTESIAN_POINT ( 'NONE',  ( -106.3947958612632050, -283.9022967309953742, -236.9970283271693177 ) ) ;
#36346 = CARTESIAN_POINT ( 'NONE',  ( -50.00635066727710409, -298.8278255376194465, -198.2291897246198289 ) ) ;
#36347 = CARTESIAN_POINT ( 'NONE',  ( -107.7711184354598544, -292.4418267014910953, -248.2699836233372537 ) ) ;
#36348 = CARTESIAN_POINT ( 'NONE',  ( -73.68076834684288201, -275.0051361215985253, -203.0856402590743244 ) ) ;
#36349 = CARTESIAN_POINT ( 'NONE',  ( 34.64721688629088447, -275.0565429930813934, -258.0523117833445212 ) ) ;
#36350 = CARTESIAN_POINT ( 'NONE',  ( -42.50260136110413356, -297.1174249626574806, -345.1833456158858553 ) ) ;
#36351 = CARTESIAN_POINT ( 'NONE',  ( -99.86902646110527826, -290.1229547493315408, -315.3207015565205324 ) ) ;
#36352 = CARTESIAN_POINT ( 'NONE',  ( 21.38827459945243348, -280.2818767912389717, -317.9220772282041594 ) ) ;
#36353 = CARTESIAN_POINT ( 'NONE',  ( -11.15125625941679566, -292.2174285290663533, -197.8960977580323117 ) ) ;
#36355 = CARTESIAN_POINT ( 'NONE',  ( -66.64725845036390695, -290.7173074597851610, -203.2448554221591621 ) ) ;
#36354 = AXIS2_PLACEMENT_3D ( 'NONE', #6563, #5628, #42043 ) ;
#36356 = B_SPLINE_CURVE_WITH_KNOTS ( 'NONE', 3,
 ( #21151, #57162, #56216, #35830, #63342, #27809 ),
 .UNSPECIFIED., .F., .F.,
 ( 4, 2, 4 ),
 ( 0.000000000000000000, 0.001588326293797077092, 0.003176652587594154184 ),
 .UNSPECIFIED. ) ;
#36357 = CARTESIAN_POINT ( 'NONE',  ( -0.4656461207899255106, -292.5618946539481726, -335.6840724772069393 ) ) ;
#36358 = EDGE_LOOP ( 'NONE', ( #19150, #54542, #38939, #56183 ) ) ;
#36359 = DIRECTION ( 'NONE',  ( -1.000000000000000000, 8.928268813181216143E-16, 0.000000000000000000 ) ) ;
#36360 = CARTESIAN_POINT ( 'NONE',  ( -107.0584599558214478, -290.3496887501069637, -248.4657962912532980 ) ) ;
#36361 = FACE_OUTER_BOUND ( 'NONE', #64581, .T. ) ;
#36362 = CARTESIAN_POINT ( 'NONE',  ( 9.657213943495289499, -287.6224896700454678, -209.6657945352397121 ) ) ;
#36363 = CARTESIAN_POINT ( 'NONE',  ( -37.37352853689063181, -300.5519495502701375, -200.3611179825600459 ) ) ;
#36364 = CARTESIAN_POINT ( 'NONE',  ( -69.44048843942523774, -294.5230718174798312, -340.1070506103724256 ) ) ;
#36365 = CARTESIAN_POINT ( 'NONE',  ( -113.8611157496324751, -285.8359972113440222, -272.8500083645006384 ) ) ;
#36366 = CARTESIAN_POINT ( 'NONE',  ( -108.9799035729099614, -284.2003328795066750, -284.3956401234800069 ) ) ;
#36367 = CARTESIAN_POINT ( 'NONE',  ( -13.54335403933255400, -278.2577663074001748, -340.1596332506368867 ) ) ;
#36368 = CARTESIAN_POINT ( 'NONE',  ( 27.20253989103627745, -292.0753591847402504, -307.8562894171354856 ) ) ;
#36369 = CARTESIAN_POINT ( 'NONE',  ( 20.49953952209563823, -295.9558177055138799, -316.5588679779123709 ) ) ;
#36370 = CARTESIAN_POINT ( 'NONE',  ( 12.00336940515391859, -275.1430749594844656, -324.7641723426035583 ) ) ;
#36371 = EDGE_LOOP ( 'NONE', ( #54611, #52907, #75468, #7871 ) ) ;
#36372 = DIRECTION ( 'NONE',  ( -0.000000000000000000, -0.000000000000000000, 1.000000000000000000 ) ) ;
#36373 = CARTESIAN_POINT ( 'NONE',  ( -19.29635662870749968, -294.4929693733215004, -345.2498696573192092 ) ) ;
#36374 = CARTESIAN_POINT ( 'NONE',  ( 32.76361034346400913, -289.7991338785600988, -295.3922913539431647 ) ) ;
#36375 = CARTESIAN_POINT ( 'NONE',  ( -54.90415217815425564, -295.8263339674465442, -197.3935939614778761 ) ) ;
#36376 = CARTESIAN_POINT ( 'NONE',  ( -3.593475819944103922, -299.5450462478421514, -193.6641989976668299 ) ) ;
#36377 = CARTESIAN_POINT ( 'NONE',  ( 27.74512343043636164, -287.7506908613603969, -236.9689384534894430 ) ) ;
#36378 = ADVANCED_FACE ( 'NONE', ( #17105 ), #10912, .T. ) ;
#36379 = CARTESIAN_POINT ( 'NONE',  ( -59.60824655745756928, -276.3924387684125463, -343.8255387760003714 ) ) ;
#36380 = CARTESIAN_POINT ( 'NONE',  ( -79.41425143792584151, -296.2557669218658134, -334.7289143769236830 ) ) ;
#36381 = CARTESIAN_POINT ( 'NONE',  ( -6.156899895186679572, -286.7863184127784280, -339.4104750969341922 ) ) ;
#36382 = CARTESIAN_POINT ( 'NONE',  ( -36.27048488967021456, -295.3723825001221144, -347.3456204804983827 ) ) ;
#36383 = CARTESIAN_POINT ( 'NONE',  ( -66.57643662309044430, -291.9916345885015403, -203.4476091154623703 ) ) ;
#36384 = CARTESIAN_POINT ( 'NONE',  ( 197.6900603589809009, 68.42838418738361383, -10.08352334802372496 ) ) ;
#36385 = LINE ( 'NONE', #51049, #73489 ) ;
#36386 = DIRECTION ( 'NONE',  ( -0.000000000000000000, -0.000000000000000000, 1.000000000000000000 ) ) ;
#36387 = CARTESIAN_POINT ( 'NONE',  ( -37.99609804505431043, -287.5642081643197230, -194.0572549159202538 ) ) ;
#36388 = CARTESIAN_POINT ( 'NONE',  ( 25.18497378105905682, -285.6952119285918457, -320.2651865833026363 ) ) ;
#36389 = ORIENTED_EDGE ( 'NONE', *, *, #53514, .F. ) ;
#36390 = CARTESIAN_POINT ( 'NONE',  ( -97.61182796767998582, -278.5406794153579426, -222.6031398282109990 ) ) ;
#36391 = CARTESIAN_POINT ( 'NONE',  ( -48.57947521258299162, -285.1957341605266834, -344.3458517822152771 ) ) ;
#36392 = CARTESIAN_POINT ( 'NONE',  ( -112.5602352529624568, -282.9537688751075279, -284.0973899021352054 ) ) ;
#36393 = CARTESIAN_POINT ( 'NONE',  ( 23.11723423016862000, -286.2273906548497280, -313.7895816412628847 ) ) ;
#36394 = CARTESIAN_POINT ( 'NONE',  ( 35.31577387817176117, -277.6868993481881489, -291.8824373098256046 ) ) ;
#36395 = CARTESIAN_POINT ( 'NONE',  ( -91.89501436541394241, -297.7388628330472784, -221.7614847793745412 ) ) ;
#36396 = VERTEX_POINT ( 'NONE', #52151 ) ;
#36397 = CARTESIAN_POINT ( 'NONE',  ( -42.44054460876731127, -293.8026256444777573, -343.6771821389189654 ) ) ;
#36398 = CARTESIAN_POINT ( 'NONE',  ( -64.71381235846634183, -280.3554992246197344, -198.4434247771710886 ) ) ;
#36400 = CARTESIAN_POINT ( 'NONE',  ( -91.36656658136038800, -278.6059421941404253, -221.1147326024030519 ) ) ;
#36399 = CARTESIAN_POINT ( 'NONE',  ( -109.6218116890025271, -278.6916863063167966, -259.7836677673691383 ) ) ;
#36401 = CARTESIAN_POINT ( 'NONE',  ( -60.78974241462493211, -274.8346646958725046, -197.2873410775770537 ) ) ;
#36402 = CARTESIAN_POINT ( 'NONE',  ( -38.55391650943938942, -275.9873527451235873, -347.0424262818040120 ) ) ;
#36403 = CARTESIAN_POINT ( 'NONE',  ( -84.59855605908614962, -218.1032794253833345, -349.8295654733143465 ) ) ;
#36404 = ADVANCED_FACE ( 'NONE', ( #88592 ), #16633, .F. ) ;
#36405 = CARTESIAN_POINT ( 'NONE',  ( -90.29058621344924518, -297.2085371877467992, -325.5249781917722771 ) ) ;
#36406 = CARTESIAN_POINT ( 'NONE',  ( 175.2296996224750103, 133.0000000000000000, 0.000000000000000000 ) ) ;
#36407 = DIRECTION ( 'NONE',  ( -0.000000000000000000, 1.000000000000000000, 1.224646799147353207E-16 ) ) ;
#36408 = CARTESIAN_POINT ( 'NONE',  ( -101.2675758579773628, -286.1219871243400803, -234.3723955102004481 ) ) ;
#36409 = CARTESIAN_POINT ( 'NONE',  ( -62.88221399330386419, -287.4842605982757391, -198.7953708380715625 ) ) ;
#36410 = CARTESIAN_POINT ( 'NONE',  ( 10.17523427537661895, -287.7253086583515369, -325.9801229707090329 ) ) ;
#36411 = CARTESIAN_POINT ( 'NONE',  ( -4.196030428723147132, -282.1344808644357158, -339.8082347460974688 ) ) ;
#36412 = CARTESIAN_POINT ( 'NONE',  ( -107.9870926799286082, -277.2315822329670141, -249.0147148451659973 ) ) ;
#36413 = CARTESIAN_POINT ( 'NONE',  ( -110.1870792805642623, -286.2271010746590036, -284.6585379884362510 ) ) ;
#36414 = CARTESIAN_POINT ( 'NONE',  ( -54.63690488973530535, -278.3058510332486435, -198.6733560630677573 ) ) ;
#36415 = CARTESIAN_POINT ( 'NONE',  ( -45.94934448409083672, -278.4786179343786330, -343.3994261518290614 ) ) ;
#36416 = CARTESIAN_POINT ( 'NONE',  ( 0.6391080398062483070, -275.0658396896797058, -207.9476046015776092 ) ) ;
#36417 = CARTESIAN_POINT ( 'NONE',  ( 23.81588913860320744, -286.9645263509295887, -316.4887452234615921 ) ) ;
#36418 = CARTESIAN_POINT ( 'NONE',  ( -71.65743201224400138, -284.2968648249295711, -339.1113133748129940 ) ) ;
#36419 = CARTESIAN_POINT ( 'NONE',  ( 19.74206998457583495, -282.7462015964781585, -322.0236625296275292 ) ) ;
#36420 = ORIENTED_EDGE ( 'NONE', *, *, #24999, .T. ) ;
#36421 = VERTEX_POINT ( 'NONE', #74386 ) ;
#36422 = DIRECTION ( 'NONE',  ( 0.000000000000000000, 0.000000000000000000, 1.000000000000000000 ) ) ;
#36423 = CARTESIAN_POINT ( 'NONE',  ( -9.986839191855487741, -290.5591411672682511, -341.0153256683562972 ) ) ;
#36424 = CARTESIAN_POINT ( 'NONE',  ( -87.07664730730149927, -288.4124882830251408, -328.5661898010961295 ) ) ;
#36425 = CARTESIAN_POINT ( 'NONE',  ( -37.13892041667711652, -297.2519284402460471, -197.1968135573092695 ) ) ;
#36426 = CARTESIAN_POINT ( 'NONE',  ( 36.60842445409088697, -292.6355088390661194, -249.2254012382605026 ) ) ;
#36427 = CARTESIAN_POINT ( 'NONE',  ( -20.99418713197473707, -287.3184175860797609, -342.2183832333910800 ) ) ;
#36428 = CARTESIAN_POINT ( 'NONE',  ( 22.12749083094972136, -292.4013691240335788, -314.4223179443346226 ) ) ;
#36429 = CARTESIAN_POINT ( 'NONE',  ( 33.76947212699940337, -288.5180270808524483, -252.1354027589475777 ) ) ;
#36430 = CARTESIAN_POINT ( 'NONE',  ( 35.78497577281001440, -296.2662352645559167, -287.0191576251351080 ) ) ;
#36431 = CARTESIAN_POINT ( 'NONE',  ( 34.05194201517003449, -289.8489573497968195, -293.3382481384838343 ) ) ;
#36432 = CARTESIAN_POINT ( 'NONE',  ( -106.6662369310979130, -288.9305696963664900, -241.3070817583218002 ) ) ;
#36433 = CIRCLE ( 'NONE', #71258, 2.999999999999997780 ) ;
#36434 = CARTESIAN_POINT ( 'NONE',  ( -112.3862957294052478, -292.5394277079515177, -271.3649819998132671 ) ) ;
#36435 = CARTESIAN_POINT ( 'NONE',  ( -108.2595005624916951, -285.7339114465795546, -252.0834258337313258 ) ) ;
#36436 = CARTESIAN_POINT ( 'NONE',  ( -6.659168104624491491, -294.4541666545368912, -201.7278554629307621 ) ) ;
#36437 = LINE ( 'NONE', #13282, #501 ) ;
#36438 = DIRECTION ( 'NONE',  ( 0.000000000000000000, 1.000000000000000000, 0.000000000000000000 ) ) ;
#36439 = CARTESIAN_POINT ( 'NONE',  ( -112.6969001285957006, -274.5317257255920822, -270.3862698198935846 ) ) ;
#36440 = CARTESIAN_POINT ( 'NONE',  ( -3.555882753585494882, -281.7914482473875069, -335.2682982919924939 ) ) ;
#36441 = CARTESIAN_POINT ( 'NONE',  ( -54.16233559640447481, -281.2678529830369030, -343.5040780991286056 ) ) ;
#36442 = CARTESIAN_POINT ( 'NONE',  ( -44.79016990575826895, -294.3411911617103556, -346.8910703211512327 ) ) ;
#36443 = CARTESIAN_POINT ( 'NONE',  ( 31.12057963426378748, -273.4186716975830791, -242.1036699288960961 ) ) ;
#36444 = CARTESIAN_POINT ( 'NONE',  ( -81.69661911889993178, -275.7412690584095571, -330.1436853111102891 ) ) ;
#36445 = CARTESIAN_POINT ( 'NONE',  ( -110.5892369044117061, -297.7808603486535048, -276.9604793670855543 ) ) ;
#36446 = CARTESIAN_POINT ( 'NONE',  ( -38.33143454498044633, -272.6147074871836367, -193.9567547502762466 ) ) ;
#36447 = CARTESIAN_POINT ( 'NONE',  ( 33.87388428204629776, -294.7346217578486858, -251.8215533801229640 ) ) ;
#36448 = CARTESIAN_POINT ( 'NONE',  ( 82.64890176555634582, -299.5541904835127980, -193.4651424135224147 ) ) ;
#36449 = CARTESIAN_POINT ( 'NONE',  ( -9.159250691535568478, -295.4768390451197888, -337.8903180535593833 ) ) ;
#36450 = CARTESIAN_POINT ( 'NONE',  ( 202.8019728163925492, 61.40723988820082013, 8.999999999999994671 ) ) ;
#36452 = CARTESIAN_POINT ( 'NONE',  ( -107.6028088719952649, -296.2903010737892373, -290.1696161102805718 ) ) ;
#36451 = CARTESIAN_POINT ( 'NONE',  ( 36.12190479245951025, -285.3571910632523441, -253.5256369598023980 ) ) ;
#36453 = CARTESIAN_POINT ( 'NONE',  ( -108.2271400225182134, -284.1678567040683561, -300.5683431800719063 ) ) ;
#36454 = CARTESIAN_POINT ( 'NONE',  ( 33.84149516489766540, -286.8448202923074746, -240.9183114128727539 ) ) ;
#36455 = CARTESIAN_POINT ( 'NONE',  ( 35.43658105321669183, -291.3272050204694779, -252.8893424519120856 ) ) ;
#36456 = CARTESIAN_POINT ( 'NONE',  ( -7.590052577300235193, -279.6295167762784786, -199.5019549692357828 ) ) ;
#36457 = CARTESIAN_POINT ( 'NONE',  ( -69.91165696735023971, -274.9809262143061233, -337.9199732462171255 ) ) ;
#36458 = DIRECTION ( 'NONE',  ( -5.880589007913310608E-16, 0.000000000000000000, 1.000000000000000000 ) ) ;
#36459 = CARTESIAN_POINT ( 'NONE',  ( 31.35162347390982163, -286.0022478705710114, -244.3649491040047224 ) ) ;
#36461 = CARTESIAN_POINT ( 'NONE',  ( 175.2296996224750103, 134.0000000000000284, 0.000000000000000000 ) ) ;
#36460 = CARTESIAN_POINT ( 'NONE',  ( -62.67457298357670226, -288.2944788387416679, -342.8033148382984336 ) ) ;
#36462 = FACE_OUTER_BOUND ( 'NONE', #25091, .T. ) ;
#36463 = CARTESIAN_POINT ( 'NONE',  ( -97.04372138491163469, -297.5514353866338411, -313.7659610498172356 ) ) ;
#36464 = CARTESIAN_POINT ( 'NONE',  ( -38.18177614580379498, -281.4670832233994133, -193.9549626837489598 ) ) ;
#36466 = CARTESIAN_POINT ( 'NONE',  ( 34.58865079827489808, -281.0530422292969206, -257.7868544879223123 ) ) ;
#36465 = CARTESIAN_POINT ( 'NONE',  ( -108.2935150985727830, -294.8996634671069046, -244.9791016358023796 ) ) ;
#36467 = CARTESIAN_POINT ( 'NONE',  ( 24.88753236352268061, -294.3209627146312641, -315.7322275433445498 ) ) ;
#36468 = ADVANCED_FACE ( 'NONE', ( #3351 ), #446, .T. ) ;
#36469 = CARTESIAN_POINT ( 'NONE',  ( -108.6561274243400419, -280.8541387050315734, -246.9742846930662381 ) ) ;
#36470 = CARTESIAN_POINT ( 'NONE',  ( -92.91515624540760143, -296.2879147817570811, -222.6448787601670745 ) ) ;
#36471 = ORIENTED_EDGE ( 'NONE', *, *, #88813, .F. ) ;
#36472 = DIRECTION ( 'NONE',  ( -0.000000000000000000, -0.000000000000000000, -1.000000000000000000 ) ) ;
#36473 = CARTESIAN_POINT ( 'NONE',  ( -69.69987050817832142, -285.4601682883286458, -337.6418301774566544 ) ) ;
#36474 = CARTESIAN_POINT ( 'NONE',  ( 222.8344101925596306, 0.000000000000000000, 22.50000000000000000 ) ) ;
#36475 = CARTESIAN_POINT ( 'NONE',  ( -37.30987171927208834, -283.5523547857346784, -195.3611179825600175 ) ) ;
#36476 = CARTESIAN_POINT ( 'NONE',  ( 26.80140507305364395, -274.1918399145835110, -228.0548433232394814 ) ) ;
#36477 = CARTESIAN_POINT ( 'NONE',  ( -109.6998281673912459, -290.5178377968475161, -260.3270114090263974 ) ) ;
#36478 = CARTESIAN_POINT ( 'NONE',  ( 35.39094872883214293, -283.2272651635992133, -282.2215371733696543 ) ) ;
#36479 = CARTESIAN_POINT ( 'NONE',  ( -94.40985545298124748, -274.8081166465035494, -223.5474842818036052 ) ) ;
#36480 = CARTESIAN_POINT ( 'NONE',  ( -52.73586600945811398, -284.8462156810082888, -345.0438560502974497 ) ) ;
#36481 = CARTESIAN_POINT ( 'NONE',  ( 36.09993931412886781, -280.3598372342331686, -271.3342546248802023 ) ) ;
#36482 = CARTESIAN_POINT ( 'NONE',  ( -93.72846963032985457, -281.2394580579449439, -220.8892438720545499 ) ) ;
#36483 = CARTESIAN_POINT ( 'NONE',  ( -102.7201589957636543, -273.2509871067296672, -229.6836411608153412 ) ) ;
#36484 = CARTESIAN_POINT ( 'NONE',  ( -21.35271907222038124, -274.0850939294836621, -195.0394578224199051 ) ) ;
#36485 = CARTESIAN_POINT ( 'NONE',  ( 30.03161579577744789, -295.0515150704758867, -238.5827869729036195 ) ) ;
#36486 = CARTESIAN_POINT ( 'NONE',  ( 129.9467878515196162, -299.5541904835127980, -195.3611179825600175 ) ) ;
#36487 = LINE ( 'NONE', #85741, #2770 ) ;
#36488 = EDGE_CURVE ( 'NONE', #40445, #76858, #32306, .T. ) ;
#36489 = CARTESIAN_POINT ( 'NONE',  ( -27.92522668614256531, -293.0735382079603824, -345.5909149364619566 ) ) ;
#36490 = CARTESIAN_POINT ( 'NONE',  ( -63.32274966100137448, -273.2119769330540180, -202.0616450105656838 ) ) ;
#36491 = AXIS2_PLACEMENT_3D ( 'NONE', #64374, #26936, #71921 ) ;
#36492 = CARTESIAN_POINT ( 'NONE',  ( -74.35964818113419028, -293.0891981603970180, -203.6349666226969362 ) ) ;
#36494 = CARTESIAN_POINT ( 'NONE',  ( 17.19607135086742744, -294.0138978930153257, -216.4938751055042587 ) ) ;
#36493 = CARTESIAN_POINT ( 'NONE',  ( -95.99890600148557951, -275.6948066931273615, -223.6242672951989618 ) ) ;
#36495 = CARTESIAN_POINT ( 'NONE',  ( 27.29204555773020147, -290.0584838156564160, -308.1797603603603761 ) ) ;
#36496 = CARTESIAN_POINT ( 'NONE',  ( -81.93169923006281863, -275.6612755205580925, -330.4590414379638332 ) ) ;
#36497 = CARTESIAN_POINT ( 'NONE',  ( -96.40085331815474490, -279.8470819201439213, -315.6748093526999810 ) ) ;
#36498 = CARTESIAN_POINT ( 'NONE',  ( -17.86686179102301963, -292.8789093712503018, -342.2084900074823963 ) ) ;
#36499 = CARTESIAN_POINT ( 'NONE',  ( 24.92886264784288741, -283.9922253867258064, -313.5427504955195559 ) ) ;
#36500 = ORIENTED_EDGE ( 'NONE', *, *, #69967, .F. ) ;
#36501 = CARTESIAN_POINT ( 'NONE',  ( -101.7918859083870728, -283.7499483021175024, -304.7945536219049245 ) ) ;
#36502 = CARTESIAN_POINT ( 'NONE',  ( -71.11092043020893527, -280.6965132133107090, -201.5052375403541305 ) ) ;
#36503 = CARTESIAN_POINT ( 'NONE',  ( -85.86277093032305174, -282.5022165188523786, -329.6377103750797346 ) ) ;
#36504 = CARTESIAN_POINT ( 'NONE',  ( -68.58776078581355762, -280.5927399623715246, -200.2289890805708410 ) ) ;
#36505 = EDGE_CURVE ( 'NONE', #75307, #73161, #51773, .T. ) ;
#36506 = DIRECTION ( 'NONE',  ( 0.000000000000000000, 0.000000000000000000, 1.000000000000000000 ) ) ;
#36507 = CARTESIAN_POINT ( 'NONE',  ( 31.91557222956466333, -276.6572711153784780, -238.2019694202430173 ) ) ;
#36508 = CARTESIAN_POINT ( 'NONE',  ( -92.08974858914540107, -293.6948066931273047, -226.7417163044926838 ) ) ;
#36509 = ORIENTED_EDGE ( 'NONE', *, *, #37177, .T. ) ;
#36510 = CARTESIAN_POINT ( 'NONE',  ( -104.8701366780603053, -274.9777367177613314, -238.1130377222687287 ) ) ;
#36511 = CARTESIAN_POINT ( 'NONE',  ( -100.5817118619040400, -276.0356198849154339, -310.1130789898172679 ) ) ;
#36512 = CARTESIAN_POINT ( 'NONE',  ( -99.21907647818083831, -292.9042021024465043, -226.2571010356958539 ) ) ;
#36513 = CARTESIAN_POINT ( 'NONE',  ( 34.16555331793885131, -293.1015729161529748, -285.6068254659196555 ) ) ;
#36514 = CARTESIAN_POINT ( 'NONE',  ( -62.74925240929006520, -288.8817083902563922, -343.0396539042784525 ) ) ;
#36515 = CARTESIAN_POINT ( 'NONE',  ( 208.1233865313629394, 36.80875831278186183, 13.45150779440604794 ) ) ;
#36517 = CARTESIAN_POINT ( 'NONE',  ( -94.04973101028605242, -282.2891591118892052, -317.5907659872622730 ) ) ;
#36516 = CARTESIAN_POINT ( 'NONE',  ( 38.85486018996409996, -292.0548243258436401, -264.6435584202449718 ) ) ;
#36518 = CARTESIAN_POINT ( 'NONE',  ( -70.50328470984743490, -291.3544868212671304, -336.7918843677855421 ) ) ;
#36519 = CARTESIAN_POINT ( 'NONE',  ( 17.98709336804638426, -283.5528532863116880, -318.7343346335289880 ) ) ;
#36520 = CARTESIAN_POINT ( 'NONE',  ( -54.43751496834735804, -290.2077171707551315, -345.2525055622558057 ) ) ;
#36521 = CARTESIAN_POINT ( 'NONE',  ( 18.87944378451639338, -281.3831051958953822, -223.6815336760596722 ) ) ;
#36522 = CARTESIAN_POINT ( 'NONE',  ( -19.39527459654731345, -293.6213151031814732, -344.8867495324243464 ) ) ;
#36523 = CARTESIAN_POINT ( 'NONE',  ( 12.31926571097654133, -289.1836920822031516, -328.9951293747710110 ) ) ;
#36524 = CARTESIAN_POINT ( 'NONE',  ( -20.50376113063230932, -289.3339898784125808, -345.4891115516581976 ) ) ;
#36525 = CARTESIAN_POINT ( 'NONE',  ( -96.57606785617630862, -285.3157047089517846, -227.6749393446403644 ) ) ;
#36526 = ORIENTED_EDGE ( 'NONE', *, *, #36918, .T. ) ;
#36527 = DIRECTION ( 'NONE',  ( 0.000000000000000000, 1.000000000000000000, 0.000000000000000000 ) ) ;
#36528 = CARTESIAN_POINT ( 'NONE',  ( -32.07434690690416090, -296.8468130020423814, -345.9556422431013516 ) ) ;
#36529 = CARTESIAN_POINT ( 'NONE',  ( -76.84206035037567517, -294.2538731055311132, -335.9438991138271149 ) ) ;
#36530 = EDGE_CURVE ( 'NONE', #16501, #44165, #17170, .T. ) ;
#36531 = CARTESIAN_POINT ( 'NONE',  ( -93.26212900985719045, -278.2810089578179031, -223.0521492308486700 ) ) ;
#36532 = CARTESIAN_POINT ( 'NONE',  ( -85.76463616281066038, -272.9096813799963002, -210.5719369476023246 ) ) ;
#36533 = CARTESIAN_POINT ( 'NONE',  ( -90.92454900864993306, -294.3095183062736169, -321.0269811628870116 ) ) ;
#36534 = CARTESIAN_POINT ( 'NONE',  ( 36.71310783501684227, -277.3281547737376513, -271.5795866355633734 ) ) ;
#36535 = CARTESIAN_POINT ( 'NONE',  ( 53.24685640498476857, -297.4411105498125494, -196.3754083438691680 ) ) ;
#36536 = CARTESIAN_POINT ( 'NONE',  ( 34.03030215777685896, -294.5319224616985707, -253.1853297622871253 ) ) ;
#36537 = CARTESIAN_POINT ( 'NONE',  ( -107.8965870705577714, -297.3697980464898478, -290.2667453949376295 ) ) ;
#36538 = CARTESIAN_POINT ( 'NONE',  ( 204.6539576904058606, 287.9062406767683910, -5.225551010890931103 ) ) ;
#36539 = CARTESIAN_POINT ( 'NONE',  ( -81.86368492034900157, -295.4474594603536275, -209.7339231300119309 ) ) ;
#36540 = CARTESIAN_POINT ( 'NONE',  ( -43.29015940290972253, -298.6304444905814535, -193.6403276531499102 ) ) ;
#36541 = CARTESIAN_POINT ( 'NONE',  ( -111.8761160808900712, -274.6594503038225525, -262.0171689033327311 ) ) ;
#36542 = CARTESIAN_POINT ( 'NONE',  ( -50.78292581272314266, -290.1692093377737365, -342.4042244765716987 ) ) ;
#36543 = CARTESIAN_POINT ( 'NONE',  ( -55.80455848221016879, -295.6296250512015718, -341.0620141482948497 ) ) ;
#36544 = CARTESIAN_POINT ( 'NONE',  ( -106.0654729793480016, -280.1271758439433484, -301.3983442815521130 ) ) ;
#36545 = CARTESIAN_POINT ( 'NONE',  ( -113.8917448642033463, -277.2215908492424887, -271.5836930016295696 ) ) ;
#36546 = CARTESIAN_POINT ( 'NONE',  ( -1.688774056714934524, -281.9407952177457446, -338.4946754226625671 ) ) ;
#36547 = CARTESIAN_POINT ( 'NONE',  ( 32.46401906989120079, -274.4860853738308037, -237.9779001241196568 ) ) ;
#36548 = CARTESIAN_POINT ( 'NONE',  ( -64.60509204537189021, -281.4907336159563442, -339.6288713715461540 ) ) ;
#36549 = CARTESIAN_POINT ( 'NONE',  ( -81.75587349860425945, -277.8582113541465333, -208.4432561216914621 ) ) ;
#36550 = CARTESIAN_POINT ( 'NONE',  ( -85.60753638395715370, -277.3865062877884498, -212.6700588687814957 ) ) ;
#36551 = CARTESIAN_POINT ( 'NONE',  ( -103.7288933501302637, -271.5528551873201764, -238.6102834815369533 ) ) ;
#36552 = CARTESIAN_POINT ( 'NONE',  ( -1.924503310254754851, -278.5832811827476121, -336.4861826383494758 ) ) ;
#36553 = CARTESIAN_POINT ( 'NONE',  ( 199.3803347170859865, 17.19615242270659294, -9.999999999999994671 ) ) ;
#36554 = CIRCLE ( 'NONE', #68331, 5.000000000000004441 ) ;
#36555 = CARTESIAN_POINT ( 'NONE',  ( 18.22031444830711067, -290.8646583116623106, -219.4566060044820688 ) ) ;
#36556 = CIRCLE ( 'NONE', #84942, 7.500000000000012434 ) ;
#36557 = CARTESIAN_POINT ( 'NONE',  ( -51.68530585684888479, -289.2307918871019865, -346.0133550591836524 ) ) ;
#36558 = CARTESIAN_POINT ( 'NONE',  ( -5.904785239958090237, -276.4646039017158046, -202.0841173688888830 ) ) ;
#36559 = CARTESIAN_POINT ( 'NONE',  ( -91.62711212189105936, -271.2786216151463350, -218.5920247042811866 ) ) ;
#36560 = CARTESIAN_POINT ( 'NONE',  ( -99.20813169897998307, -284.3570358326381324, -224.7027244813578761 ) ) ;
#36561 = DIRECTION ( 'NONE',  ( -1.000000000000000000, 0.000000000000000000, 0.000000000000000000 ) ) ;
#36562 = CIRCLE ( 'NONE', #65334, 2.999999999999993783 ) ;
#36563 = CARTESIAN_POINT ( 'NONE',  ( -85.12579157651852313, -281.7112199555536449, -328.2349310359689980 ) ) ;
#36564 = DIRECTION ( 'NONE',  ( 0.000000000000000000, 1.000000000000000000, 0.000000000000000000 ) ) ;
#36565 = CARTESIAN_POINT ( 'NONE',  ( 22.92268566804259677, -291.7660446965438155, -228.4422569640934455 ) ) ;
#36566 = CARTESIAN_POINT ( 'NONE',  ( -22.18487566183325654, -284.3877777815829404, -197.6369298623386896 ) ) ;
#36567 = CARTESIAN_POINT ( 'NONE',  ( 208.0514444522711131, 35.78458379568167658, 14.36594018319230592 ) ) ;
#36568 = DIRECTION ( 'NONE',  ( -1.000000000000000000, 0.000000000000000000, 0.000000000000000000 ) ) ;
#36569 = CARTESIAN_POINT ( 'NONE',  ( 24.24440325228689019, -290.9710883034318272, -227.5348283827006526 ) ) ;
#36570 = CARTESIAN_POINT ( 'NONE',  ( -67.62416511008005671, -281.9222153161818483, -340.4016781501875926 ) ) ;
#36571 = CARTESIAN_POINT ( 'NONE',  ( -41.88570400320441678, -278.7104610007943961, -344.0338310570593876 ) ) ;
#36572 = CARTESIAN_POINT ( 'NONE',  ( -105.4241671716930995, -285.3010193932071843, -305.5878671253857419 ) ) ;
#36573 = CARTESIAN_POINT ( 'NONE',  ( -98.10706653902032315, -285.1137375108239098, -229.9065725649641365 ) ) ;
#36574 = CARTESIAN_POINT ( 'NONE',  ( -51.37562253531062595, -278.6604086069558548, -342.5997775589087837 ) ) ;
#36575 = CARTESIAN_POINT ( 'NONE',  ( -110.5130208671179020, -279.3872127908599623, -267.9130364060530383 ) ) ;
#36576 = ADVANCED_FACE ( 'NONE', ( #56374 ), #88185, .T. ) ;
#36577 = CARTESIAN_POINT ( 'NONE',  ( -79.82680273196537257, -287.4782616354280549, -208.4921339988828208 ) ) ;
#36578 = ORIENTED_EDGE ( 'NONE', *, *, #43123, .F. ) ;
#36579 = CARTESIAN_POINT ( 'NONE',  ( -109.4382868577820886, -296.0417583861024582, -297.5500918960469221 ) ) ;
#36580 = CARTESIAN_POINT ( 'NONE',  ( 33.89065833062556976, -289.8232291058309329, -292.8447225331511845 ) ) ;
#36581 = LINE ( 'NONE', #71190, #15570 ) ;
#36582 = CARTESIAN_POINT ( 'NONE',  ( 13.84574458161073096, -284.9090924074130839, -334.4957818155094174 ) ) ;
#36583 = VERTEX_POINT ( 'NONE', #61602 ) ;
#36584 = CARTESIAN_POINT ( 'NONE',  ( 32.67336439791520775, -292.3406053428197424, -300.5663890819524227 ) ) ;
#36585 = CARTESIAN_POINT ( 'NONE',  ( 7.332005941075407485, -288.1935156473381880, -211.6880588197431052 ) ) ;
#36586 = CARTESIAN_POINT ( 'NONE',  ( -108.2036977293781206, -280.5913093958762943, -248.9940566479791073 ) ) ;
#36587 = CARTESIAN_POINT ( 'NONE',  ( 21.95943204025457263, -289.6290520084179434, -318.5686651770561753 ) ) ;
#36588 = CARTESIAN_POINT ( 'NONE',  ( -69.85372365634481184, -285.4804333070601956, -337.9620477735047643 ) ) ;
#36589 = CARTESIAN_POINT ( 'NONE',  ( -112.4839403549753740, -278.5085738127202717, -287.1731297069448487 ) ) ;
#36590 = VERTEX_POINT ( 'NONE', #5714 ) ;
#36591 = CARTESIAN_POINT ( 'NONE',  ( 28.31113909985324639, -292.1282277802108638, -307.8702154671547078 ) ) ;
#36592 = CARTESIAN_POINT ( 'NONE',  ( 12.99377416014388054, -280.5661413056571405, -212.0915716254347956 ) ) ;
#36593 = CARTESIAN_POINT ( 'NONE',  ( -62.46971173697773594, -275.5821315465273642, -200.5080685700372101 ) ) ;
#36594 = CARTESIAN_POINT ( 'NONE',  ( 196.7032892706336895, 294.4729419525710341, -7.987695993747508716 ) ) ;
#36595 = CARTESIAN_POINT ( 'NONE',  ( -85.33152481854864391, -293.9090924074130839, -210.2361428286349110 ) ) ;
#36596 = CARTESIAN_POINT ( 'NONE',  ( -94.31169722839038627, -271.4820000931889581, -220.0779851703954932 ) ) ;
#36597 = FACE_OUTER_BOUND ( 'NONE', #18935, .T. ) ;
#36598 = CARTESIAN_POINT ( 'NONE',  ( -54.50116472288227243, -279.3334604347061827, -199.2909844019335424 ) ) ;
#36599 = CARTESIAN_POINT ( 'NONE',  ( 37.52092034518254593, -276.9620950208469594, -286.6581229933371446 ) ) ;
#36600 = CARTESIAN_POINT ( 'NONE',  ( -70.75114926502246249, -299.0278412241978003, -204.7789325566142509 ) ) ;
#36601 = CARTESIAN_POINT ( 'NONE',  ( -37.32636916822458062, -282.1106815811281763, -347.1388483921566603 ) ) ;
#36602 = CARTESIAN_POINT ( 'NONE',  ( -88.64898494609887791, -293.0808336801002270, -216.9466971967346183 ) ) ;
#36603 = CARTESIAN_POINT ( 'NONE',  ( -72.97425534808641601, -299.1092219085675765, -202.8266578592474900 ) ) ;
#36604 = CARTESIAN_POINT ( 'NONE',  ( -82.74762329647232662, -298.6521798275545621, -208.5998954309416149 ) ) ;
#36605 = CARTESIAN_POINT ( 'NONE',  ( -20.40918813156419276, -296.8344807796837017, -343.3070488997238385 ) ) ;
#36606 = CARTESIAN_POINT ( 'NONE',  ( -54.12501131020716372, -281.2678529809568886, -343.3415255826482166 ) ) ;
#36607 = CARTESIAN_POINT ( 'NONE',  ( -104.6782312795411372, -270.9983245579026061, -238.1487232867053194 ) ) ;
#36608 = CARTESIAN_POINT ( 'NONE',  ( -69.47425100821460831, -287.2364620996675058, -201.2531989504296348 ) ) ;
#36609 = CARTESIAN_POINT ( 'NONE',  ( -23.74125767497766404, -287.7947294931971669, -342.4495110409590666 ) ) ;
#36610 = CARTESIAN_POINT ( 'NONE',  ( -106.2395333457863842, -263.2123202082037210, -317.5511267182615711 ) ) ;
#36611 = ORIENTED_EDGE ( 'NONE', *, *, #84552, .T. ) ;
#36612 = CARTESIAN_POINT ( 'NONE',  ( -98.72036414668833970, -289.7368448932155616, -224.8280436247866021 ) ) ;
#36613 = CARTESIAN_POINT ( 'NONE',  ( 7.989752088668538477, -288.0793214224137273, -327.6074884054769996 ) ) ;
#36614 = ORIENTED_EDGE ( 'NONE', *, *, #19380, .F. ) ;
#36615 = CARTESIAN_POINT ( 'NONE',  ( -107.6482779210042082, -286.0254304302478658, -239.5936985957671652 ) ) ;
#36616 = CARTESIAN_POINT ( 'NONE',  ( -95.28720915859398133, -278.2604657757648283, -314.7954005812092078 ) ) ;
#36617 = CARTESIAN_POINT ( 'NONE',  ( 19.19710981558070273, -291.7647337768821671, -218.5455268920495087 ) ) ;
#36618 = CARTESIAN_POINT ( 'NONE',  ( -111.3910719121094104, -284.9433730509019256, -291.0976395125927638 ) ) ;
#36619 = CARTESIAN_POINT ( 'NONE',  ( 38.49145981554141116, -282.9593322185109514, -261.4118835478699907 ) ) ;
#36620 = CARTESIAN_POINT ( 'NONE',  ( -35.89533557317339074, -283.3677901277861793, -347.3394982626378464 ) ) ;
#36621 = CARTESIAN_POINT ( 'NONE',  ( 31.99534397646523232, -281.5796089010634091, -247.3006495722195837 ) ) ;
#36622 = CARTESIAN_POINT ( 'NONE',  ( 203.7386562182569207, 295.8239156117444395, -54.00000000004033041 ) ) ;
#36623 = AXIS2_PLACEMENT_3D ( 'NONE', #92071, #4048, #32918 ) ;
#36624 = CARTESIAN_POINT ( 'NONE',  ( -29.49651792000635098, -278.9528598573265867, -344.8342786300242437 ) ) ;
#36625 = CARTESIAN_POINT ( 'NONE',  ( -32.21414366731176671, -123.8110585969327246, -363.4835760948135430 ) ) ;
#36626 = CARTESIAN_POINT ( 'NONE',  ( -94.98170178195216806, -238.2700655660910911, -338.7697016782443029 ) ) ;
#36627 = CARTESIAN_POINT ( 'NONE',  ( -100.8528764064363088, -272.2470669890015529, -233.9421604980510949 ) ) ;
#36628 = CARTESIAN_POINT ( 'NONE',  ( -24.92392925399193260, -294.4056183075323361, -346.3448827658697269 ) ) ;
#36629 = CARTESIAN_POINT ( 'NONE',  ( -69.32173866297239329, -196.4524155619022565, -356.9615413897211624 ) ) ;
#36630 = PRESENTATION_LAYER_ASSIGNMENT (  '', '', ( #83513 ) ) ;
#36631 = CARTESIAN_POINT ( 'NONE',  ( -97.41536935755578952, -271.8747392567533439, -222.9854645269756759 ) ) ;
#36632 = CARTESIAN_POINT ( 'NONE',  ( -47.46423532620976005, -299.7827042058585789, -196.7672158356132286 ) ) ;
#36633 = CARTESIAN_POINT ( 'NONE',  ( 34.49626605500665733, -289.0712801857098384, -285.9298822864070644 ) ) ;
#36634 = ORIENTED_EDGE ( 'NONE', *, *, #54849, .F. ) ;
#36635 = CARTESIAN_POINT ( 'NONE',  ( -90.54034823450652425, -296.7245948484388691, -325.7761734532048763 ) ) ;
#36636 = TOROIDAL_SURFACE ( 'NONE', #20008, 24.50000000000000355, 0.5000000000000000000 ) ;
#36637 = CARTESIAN_POINT ( 'NONE',  ( -91.57110656692699990, -285.7457798657515013, -221.3259721704485798 ) ) ;
#36638 = CARTESIAN_POINT ( 'NONE',  ( -1.434003112007405933, -273.4373226177796710, -202.5958628330114664 ) ) ;
#36639 = CARTESIAN_POINT ( 'NONE',  ( -13.82173177068103165, -295.5573199341579880, -343.5114420324887305 ) ) ;
#36640 = CARTESIAN_POINT ( 'NONE',  ( 4.103099884259711061, -293.0865707134055356, -205.4762506825485104 ) ) ;
#36641 = CARTESIAN_POINT ( 'NONE',  ( -28.10845212519906511, -292.3391532594212094, -197.8966477725577988 ) ) ;
#36642 = VERTEX_POINT ( 'NONE', #84286 ) ;
#36643 = CARTESIAN_POINT ( 'NONE',  ( -46.72683698870894631, -275.8540350931214675, -195.3862328366419661 ) ) ;
#36644 = CARTESIAN_POINT ( 'NONE',  ( 38.98356100422601855, -274.4289974030442636, -276.8774997145287102 ) ) ;
#36645 = ADVANCED_FACE ( 'NONE', ( #12831 ), #19901, .T. ) ;
#36646 = VERTEX_POINT ( 'NONE', #70587 ) ;
#36647 = CARTESIAN_POINT ( 'NONE',  ( -112.6560118505323231, -278.2574206360756079, -254.5724272502640133 ) ) ;
#36648 = CARTESIAN_POINT ( 'NONE',  ( -2.518364395896292240, -272.9207702641687661, -205.2936475767278637 ) ) ;
#36649 = CARTESIAN_POINT ( 'NONE',  ( -74.44163729380342431, -274.6262819062446852, -207.0739856390532907 ) ) ;
#36650 = CARTESIAN_POINT ( 'NONE',  ( 33.73465197011300631, -276.2612301697394059, -252.7100380938230444 ) ) ;
#36651 = CARTESIAN_POINT ( 'NONE',  ( -94.34139303504771590, -275.0017138394551353, -220.1116500895910235 ) ) ;
#36652 = CARTESIAN_POINT ( 'NONE',  ( 37.10665934446651448, -273.7253860698702397, -282.3433314819762927 ) ) ;
#36653 = CARTESIAN_POINT ( 'NONE',  ( -6.714656554497850038, -295.2905109197137676, -336.7378975856260013 ) ) ;
#36654 = CARTESIAN_POINT ( 'NONE',  ( 26.29316446448969202, -292.6298897485842190, -307.3202700872212176 ) ) ;
#36655 = DIRECTION ( 'NONE',  ( 0.000000000000000000, 0.000000000000000000, 1.000000000000000000 ) ) ;
#36656 = CARTESIAN_POINT ( 'NONE',  ( -113.0039659906297231, -278.8689225160429146, -284.3886998550344742 ) ) ;
#36657 = CARTESIAN_POINT ( 'NONE',  ( 25.27473730832239340, -275.2014886801561602, -232.7374641728282256 ) ) ;
#36658 =( BOUNDED_CURVE ( )  B_SPLINE_CURVE ( 3, ( #46829, #82824, #93213, #35469 ),
 .UNSPECIFIED., .F., .F. ) 
 B_SPLINE_CURVE_WITH_KNOTS ( ( 4, 4 ),
 ( 4.712388980384695003, 7.853981633974477461 ),
 .UNSPECIFIED. ) 
 CURVE ( )  GEOMETRIC_REPRESENTATION_ITEM ( )  RATIONAL_B_SPLINE_CURVE ( ( 1.000000000000000000, 0.3333333333333369231, 0.3333333333333369231, 1.000000000000000000 ) ) 
 REPRESENTATION_ITEM ( '' )  );
#36659 = CARTESIAN_POINT ( 'NONE',  ( -109.5065036537534979, -283.5595722876867057, -244.9536504930260605 ) ) ;
#36660 = CARTESIAN_POINT ( 'NONE',  ( -110.5150792763383976, -298.3312968259965601, -287.6122056707797583 ) ) ;
#36661 = CARTESIAN_POINT ( 'NONE',  ( 207.9853864603112470, 36.43026381062074393, 14.84047931273563847 ) ) ;
#36662 =( BOUNDED_SURFACE ( )  B_SPLINE_SURFACE ( 3, 2, ( 
 ( #92182, #27337, #5098 ),
 ( #13605, #56224, #69957 ),
 ( #43849, #36294, #29673 ),
 ( #64755, #65211, #79406 ),
 ( #315, #21628, #93580 ),
 ( #87398, #15927, #1244 ),
 ( #7413, #6499, #14542 ),
 ( #72292, #29199, #80309 ) ),
 .UNSPECIFIED., .F., .F., .F. ) 
 B_SPLINE_SURFACE_WITH_KNOTS ( ( 4, 2, 2, 4 ),
 ( 3, 3 ),
 ( 0.005169333131382364971, 0.006119585499877708973, 0.006594711684125380974, 0.007069837868373052975 ),
 ( 0.000000000000000000, 0.8323599711382757560 ),
 .UNSPECIFIED. ) 
 GEOMETRIC_REPRESENTATION_ITEM ( )  RATIONAL_B_SPLINE_SURFACE ( (
 ( 1.000000000000000000, 0.7562074088418379025, 0.9182612059639423396),
 ( 1.000000000000000000, 0.7715893842249162971, 0.9234184755582816040),
 ( 1.000000000000000000, 0.7884922460007639522, 0.9290856680301792236),
 ( 1.000000000000000000, 0.8086550841627961894, 0.9358458655730139686),
 ( 1.000000000000000000, 0.8144484737901919180, 0.9377882735817015813),
 ( 1.000000000000000000, 0.8225010067395548408, 0.9404881272937839487),
 ( 1.000000000000000000, 0.8247405859259469008, 0.9412390135326735852),
 ( 1.000000000000000000, 0.8247174150534301029, 0.9412312448011987964) ) ) 
 REPRESENTATION_ITEM ( '' )  SURFACE ( )  );
#36663 = CARTESIAN_POINT ( 'NONE',  ( -14.50591883633044787, -285.5529060375538961, -200.8016571277058802 ) ) ;
#36664 = CARTESIAN_POINT ( 'NONE',  ( -91.72748636521008336, -276.0802501658214396, -320.6368910297986190 ) ) ;
#36665 = CARTESIAN_POINT ( 'NONE',  ( -104.8188806823624759, -276.7337208366897698, -299.8522059376028892 ) ) ;
#36666 = CARTESIAN_POINT ( 'NONE',  ( -99.83276915398350582, -285.9910701708554370, -311.9238242501832588 ) ) ;
#36667 = CARTESIAN_POINT ( 'NONE',  ( 20.98779644816013601, -276.1338285978082467, -225.7893376335632070 ) ) ;
#36668 = DIRECTION ( 'NONE',  ( 1.000000000000000000, 0.000000000000000000, -0.000000000000000000 ) ) ;
#36669 = CARTESIAN_POINT ( 'NONE',  ( 18.30492762548804109, -274.6695298937160032, -322.4177528629518861 ) ) ;
#36670 = CARTESIAN_POINT ( 'NONE',  ( 13.89264076929903702, -282.7684531189440804, -215.2893454459286886 ) ) ;
#36671 = CARTESIAN_POINT ( 'NONE',  ( 194.3522748274950231, 20.00000000000003908, 14.59659268673782506 ) ) ;
#36672 = CARTESIAN_POINT ( 'NONE',  ( 27.67731376174091196, -289.9833601075466731, -308.8558192926971060 ) ) ;
#36673 = CARTESIAN_POINT ( 'NONE',  ( 36.64245771789629202, -291.3901424460152612, -257.7559160641364997 ) ) ;
#36674 = CARTESIAN_POINT ( 'NONE',  ( 198.6884013828325521, 64.61450673763174279, -9.555809373750800972 ) ) ;
#36675 = CARTESIAN_POINT ( 'NONE',  ( -106.7667882966642878, -271.5555031615079997, -246.2488677674949429 ) ) ;
#36676 = CARTESIAN_POINT ( 'NONE',  ( -69.53214204160927636, -289.7635455518257572, -203.4543259998931717 ) ) ;
#36677 = CARTESIAN_POINT ( 'NONE',  ( 69.94643833976951441, 44.42656045538938514, -317.4108715071801612 ) ) ;
#36678 = CARTESIAN_POINT ( 'NONE',  ( -68.86555813957184569, -295.6375985272496791, -202.2938146962868871 ) ) ;
#36679 = CARTESIAN_POINT ( 'NONE',  ( -9.831514472739019794, -287.1791487432359418, -341.5362360918209106 ) ) ;
#36680 = CARTESIAN_POINT ( 'NONE',  ( -111.9983135034200075, -282.9748233684695720, -255.9327804085828575 ) ) ;
#36681 = CARTESIAN_POINT ( 'NONE',  ( -89.29754886500192868, -285.2260625297558363, -322.5475412255105425 ) ) ;
#36682 = CARTESIAN_POINT ( 'NONE',  ( -108.2472038397971090, -285.1175623923704165, -288.3891869536726063 ) ) ;
#36683 = CARTESIAN_POINT ( 'NONE',  ( -68.65041975955305986, -291.4414453965063672, -338.9184353557639042 ) ) ;
#36684 = AXIS2_PLACEMENT_3D ( 'NONE', #16737, #87756, #45131 ) ;
#36685 = CARTESIAN_POINT ( 'NONE',  ( 11.76893841246079830, -275.0457258637568430, -211.0137858955411900 ) ) ;
#36686 = CIRCLE ( 'NONE', #88103, 0.4999999999999989453 ) ;
#36687 = CARTESIAN_POINT ( 'NONE',  ( 29.08487555839656125, -286.1080076658741405, -306.4819257647617405 ) ) ;
#36688 = CARTESIAN_POINT ( 'NONE',  ( -72.84068338500294715, -277.5091989908727328, -338.7046018065634030 ) ) ;
#36689 = CARTESIAN_POINT ( 'NONE',  ( 35.04719340458458987, -295.7671070719212025, -288.5736109239401799 ) ) ;
#36690 = CARTESIAN_POINT ( 'NONE',  ( -48.18343439339133027, -267.2165102598997919, -440.1639404234019253 ) ) ;
#36691 = CARTESIAN_POINT ( 'NONE',  ( 208.5780117385097014, 37.30339377898572195, 12.92477606492831477 ) ) ;
#36692 = CARTESIAN_POINT ( 'NONE',  ( -74.05759101585547910, -282.2353711043031694, -334.0837607528757189 ) ) ;
#36693 = EDGE_CURVE ( 'NONE', #30954, #72640, #77201, .T. ) ;
#36694 = CARTESIAN_POINT ( 'NONE',  ( -85.93000077804580883, -275.7228669243882564, -327.7808359982562934 ) ) ;
#36695 = EDGE_CURVE ( 'NONE', #49216, #48324, #79171, .T. ) ;
#36696 = CARTESIAN_POINT ( 'NONE',  ( -89.67316056524549595, -271.8103758208579279, -214.7540714163802420 ) ) ;
#36697 = CARTESIAN_POINT ( 'NONE',  ( 34.22283718884786197, -274.7034733493816816, -255.3865698946083853 ) ) ;
#36698 = CIRCLE ( 'NONE', #39702, 1.000000000000000888 ) ;
#36699 = CARTESIAN_POINT ( 'NONE',  ( 34.31746227650188530, -294.8469177054485613, -253.1121476736348654 ) ) ;
#36700 = CARTESIAN_POINT ( 'NONE',  ( 33.67716207303073617, -294.7286348754522010, -288.2421039859326584 ) ) ;
#36701 = CARTESIAN_POINT ( 'NONE',  ( 23.49500095417907630, -294.3563020352347621, -224.1064653835943261 ) ) ;
#36702 = CARTESIAN_POINT ( 'NONE',  ( 13.08346084051852820, -295.6803385282574368, -327.9691999329367036 ) ) ;
#36703 = CARTESIAN_POINT ( 'NONE',  ( -107.8351052943669828, -296.6365429268314529, -251.3477277009112925 ) ) ;
#36704 = CARTESIAN_POINT ( 'NONE',  ( -103.3927626519137419, -292.0794411334230176, -305.9994266604252857 ) ) ;
#36705 = CARTESIAN_POINT ( 'NONE',  ( -104.4159720515098684, -284.2269055385384036, -308.2850021935161067 ) ) ;
#36706 = CARTESIAN_POINT ( 'NONE',  ( -65.74186983552057484, -271.8242307191454188, -200.1066203008331001 ) ) ;
#36707 = CARTESIAN_POINT ( 'NONE',  ( 39.35486919638645986, -287.2929035427188751, -262.9593731745756600 ) ) ;
#36708 = CARTESIAN_POINT ( 'NONE',  ( -37.79500041815310851, -279.0377113513160907, -345.0172797319620486 ) ) ;
#36709 = CARTESIAN_POINT ( 'NONE',  ( -103.8387429771259463, -283.7657820774043103, -239.1718336466684605 ) ) ;
#36710 = CARTESIAN_POINT ( 'NONE',  ( 29.64716386366463041, -285.1064498332107746, -236.6343816037604881 ) ) ;
#36711 = CARTESIAN_POINT ( 'NONE',  ( -81.49943007281909502, -277.5979657031264765, -208.7948905180417682 ) ) ;
#36712 = CARTESIAN_POINT ( 'NONE',  ( -99.29329069375972949, -236.7418906163237580, -339.9611904871904358 ) ) ;
#36713 = CARTESIAN_POINT ( 'NONE',  ( -108.4239255739651782, -284.2830928118351608, -253.4162636694933326 ) ) ;
#36714 = CARTESIAN_POINT ( 'NONE',  ( 23.42291074594950118, -282.1315420025921412, -223.6956084102434090 ) ) ;
#36715 = B_SPLINE_CURVE_WITH_KNOTS ( 'NONE', 3,
 ( #72329, #93615, #351, #34938, #42018, #56746 ),
 .UNSPECIFIED., .F., .F.,
 ( 4, 2, 4 ),
 ( 0.000000000000000000, 0.0005961333682660641207, 0.001192266736532128241 ),
 .UNSPECIFIED. ) ;
#36716 = CARTESIAN_POINT ( 'NONE',  ( -67.97103996706708529, -288.5033034504162970, -340.7504904369728820 ) ) ;
#36717 = CARTESIAN_POINT ( 'NONE',  ( -42.72905994652735018, -278.7191898495472628, -346.3704382653254470 ) ) ;
#36718 = CARTESIAN_POINT ( 'NONE',  ( -9.376382623895057833, -278.0093201266830079, -341.5737523231353521 ) ) ;
#36719 = CARTESIAN_POINT ( 'NONE',  ( -51.82528398430984140, -279.6950906817163514, -198.7606225066397201 ) ) ;
#36720 = CARTESIAN_POINT ( 'NONE',  ( -27.08865172859196235, -276.1628889193509622, -196.3717911181254863 ) ) ;
#36721 = CARTESIAN_POINT ( 'NONE',  ( 26.51174344813501449, -294.1191112121877040, -313.3929404336130347 ) ) ;
#36722 = CARTESIAN_POINT ( 'NONE',  ( -2.623322973350376675, -286.6111685825279665, -336.4977058661108344 ) ) ;
#36723 = CARTESIAN_POINT ( 'NONE',  ( -103.9209820452293513, -292.6377788681243715, -233.2984732700124653 ) ) ;
#36724 = CARTESIAN_POINT ( 'NONE',  ( -45.13721603296350082, -294.0733770383077967, -343.3052652123174653 ) ) ;
#36725 = CARTESIAN_POINT ( 'NONE',  ( 17.98567555085146097, -293.8975469755371819, -318.0348663922093806 ) ) ;
#36726 = CARTESIAN_POINT ( 'NONE',  ( -70.77542480646489764, -292.7010869421544612, -201.3417108164417186 ) ) ;
#36727 = CARTESIAN_POINT ( 'NONE',  ( 20.59163003303796913, -281.5767518879754334, -225.7580228462045113 ) ) ;
#36728 = CARTESIAN_POINT ( 'NONE',  ( -36.88527894149524400, -296.9780751899973552, -193.6703088412876923 ) ) ;
#36729 = CARTESIAN_POINT ( 'NONE',  ( -12.24914102296441420, -289.3856352070126263, -343.1058186220211041 ) ) ;
#36730 = CARTESIAN_POINT ( 'NONE',  ( -98.80063803479879425, -282.0937129488573305, -314.7557629154503616 ) ) ;
#36731 = CARTESIAN_POINT ( 'NONE',  ( 20.55979956657802177, -288.5720723814009148, -321.1073080936008068 ) ) ;
#36732 = CARTESIAN_POINT ( 'NONE',  ( -83.66455760767969707, -285.7296347783826036, -213.8482704037640758 ) ) ;
#36733 = CARTESIAN_POINT ( 'NONE',  ( 197.0526034356786909, 285.3763918475410719, -111.7597976791601440 ) ) ;
#36734 = CARTESIAN_POINT ( 'NONE',  ( -57.42940174176641932, -168.5846715610379931, -362.5153972683089592 ) ) ;
#36735 = CARTESIAN_POINT ( 'NONE',  ( 179.1287263462807573, 251.3206971305780257, -164.1895290402175362 ) ) ;
#36736 = CARTESIAN_POINT ( 'NONE',  ( -92.32304736588534411, -278.4369178665999698, -222.0755825259350331 ) ) ;
#36737 = CARTESIAN_POINT ( 'NONE',  ( 15.49165899291676141, -279.7411057749791325, -219.4667166436613570 ) ) ;
#36738 = CARTESIAN_POINT ( 'NONE',  ( 23.61869896377583444, -274.5911370579396475, -223.3335545625459702 ) ) ;
#36739 = CARTESIAN_POINT ( 'NONE',  ( -110.3740896168006174, -272.9989044831370961, -270.3668062096999734 ) ) ;
#36740 = CARTESIAN_POINT ( 'NONE',  ( -81.88057515096950567, -278.0330392942730668, -208.2733180284720618 ) ) ;
#36741 = CARTESIAN_POINT ( 'NONE',  ( -45.85146970287838286, -281.1805351109912863, -344.5714084857896182 ) ) ;
#36742 = CARTESIAN_POINT ( 'NONE',  ( -69.08391957842276554, -297.2240279907319405, -339.4145181524082204 ) ) ;
#36743 = CARTESIAN_POINT ( 'NONE',  ( -34.86146857238223618, -292.5764957798779164, -197.3416897922132023 ) ) ;
#36744 = CARTESIAN_POINT ( 'NONE',  ( -78.46413158314939551, -288.3029789028551022, -331.3337140688640829 ) ) ;
#36745 = CARTESIAN_POINT ( 'NONE',  ( -7.737501600269742319, -275.0813584043654032, -199.3334482253517024 ) ) ;
#36746 = CARTESIAN_POINT ( 'NONE',  ( -108.7795722901818181, -296.9177619382888906, -255.2800064297944687 ) ) ;
#36747 = VERTEX_POINT ( 'NONE', #78155 ) ;
#36748 = CARTESIAN_POINT ( 'NONE',  ( 139.1539576904058606, 275.5000000000000568, -10.49999999999999822 ) ) ;
#36749 = AXIS2_PLACEMENT_3D ( 'NONE', #41054, #62418, #10797 ) ;
#36750 = CARTESIAN_POINT ( 'NONE',  ( -103.5439180514777746, -280.9530209141566388, -233.9388646535291230 ) ) ;
#36751 = CIRCLE ( 'NONE', #54927, 2.939656322713313230 ) ;
#36752 = AXIS2_PLACEMENT_3D ( 'NONE', #29330, #93248, #36422 ) ;
#36753 = CARTESIAN_POINT ( 'NONE',  ( 20.75249025025642169, -282.0049406448960099, -225.6272876952578770 ) ) ;
#36754 = CARTESIAN_POINT ( 'NONE',  ( -99.43405333055756046, -280.8995585493619842, -226.5602767991605333 ) ) ;
#36755 = CARTESIAN_POINT ( 'NONE',  ( 12.06662934367147244, -281.4032824717512540, -324.4187300865832526 ) ) ;
#36756 = CARTESIAN_POINT ( 'NONE',  ( -74.60743724592036585, -272.0269079481059862, -206.7255040913486255 ) ) ;
#36757 = FACE_OUTER_BOUND ( 'NONE', #65310, .T. ) ;
#36758 = CARTESIAN_POINT ( 'NONE',  ( -43.54160339317392214, -248.0334966641272842, -465.6442049081569508 ) ) ;
#36759 = AXIS2_PLACEMENT_3D ( 'NONE', #47035, #60812, #19578 ) ;
#36760 = CARTESIAN_POINT ( 'NONE',  ( 39.15551659369661763, -276.2575460780564640, -262.5864954224175563 ) ) ;
#36761 = ORIENTED_EDGE ( 'NONE', *, *, #25349, .F. ) ;
#36762 = CARTESIAN_POINT ( 'NONE',  ( 22.03347999966414150, -276.9242011569562010, -224.5189540467830511 ) ) ;
#36763 = CARTESIAN_POINT ( 'NONE',  ( -71.32522730692068080, -276.0668272448311882, -338.7988720054276541 ) ) ;
#36764 = VERTEX_POINT ( 'NONE', #47832 ) ;
#36765 = DIRECTION ( 'NONE',  ( 1.124465274301078034E-16, 1.000000000000000000, 0.000000000000000000 ) ) ;
#36766 = CARTESIAN_POINT ( 'NONE',  ( -102.9718258805812781, -286.0398257718971990, -307.4950212589780563 ) ) ;
#36767 = CIRCLE ( 'NONE', #32238, 0.5000000000000004441 ) ;
#36768 = CARTESIAN_POINT ( 'NONE',  ( -89.92528967113392468, -290.4827866808067824, -219.4929763052819567 ) ) ;
#36769 = CARTESIAN_POINT ( 'NONE',  ( 35.75473705710635386, -286.5979917014230409, -246.3114117091276398 ) ) ;
#36770 = CARTESIAN_POINT ( 'NONE',  ( -36.20007475029898814, -281.2775027747325112, -344.3656496525327384 ) ) ;
#36772 = CARTESIAN_POINT ( 'NONE',  ( 7.819583032856252558, -284.7537931863032554, -211.1201959393978029 ) ) ;
#36771 = CARTESIAN_POINT ( 'NONE',  ( -69.28119369061114696, -282.0555552826351118, -336.6716682828496801 ) ) ;
#36773 = CARTESIAN_POINT ( 'NONE',  ( 34.62302802845156435, -282.9473799628081565, -284.8538604442662745 ) ) ;
#36774 = CARTESIAN_POINT ( 'NONE',  ( 31.87779560526152167, -273.1734711437652550, -241.3536662796325913 ) ) ;
#36775 = CARTESIAN_POINT ( 'NONE',  ( -65.56194681057962725, -284.0891331744151671, -199.5653484693689848 ) ) ;
#36776 = CARTESIAN_POINT ( 'NONE',  ( -112.3117419303367654, -298.5973368378957957, -266.8548584266072226 ) ) ;
#36777 = VECTOR ( 'NONE', #15963, 1000.000000000000000 ) ;
#36778 = CARTESIAN_POINT ( 'NONE',  ( -108.0442996236418622, -279.2420133269375810, -289.4543333536269643 ) ) ;
#36779 = CARTESIAN_POINT ( 'NONE',  ( -112.3764240251258855, -286.4849981587564116, -275.6156172564502640 ) ) ;
#36780 = DIRECTION ( 'NONE',  ( -0.000000000000000000, -0.000000000000000000, 1.000000000000000000 ) ) ;
#36781 = CARTESIAN_POINT ( 'NONE',  ( 157.7374095173865385, -21.37379927922774314, 13.00000000000000178 ) ) ;
#36782 = CARTESIAN_POINT ( 'NONE',  ( 36.06695296336238954, -295.7011276235264177, -288.3173934333239004 ) ) ;
#36783 = AXIS2_PLACEMENT_3D ( 'NONE', #54393, #3755, #69543 ) ;
#36784 = CARTESIAN_POINT ( 'NONE',  ( -75.04000715050869985, -275.5542320894206796, -335.1981313066179951 ) ) ;
#36785 = CARTESIAN_POINT ( 'NONE',  ( -8.303650606907879705, -287.8786717017288765, -341.5157111399344103 ) ) ;
#36786 = CARTESIAN_POINT ( 'NONE',  ( 21.64537437584522550, -291.3360073274541264, -226.0106336735533716 ) ) ;
#36787 = CARTESIAN_POINT ( 'NONE',  ( -45.98259260431741779, -275.8486937439034250, -343.3954984292109884 ) ) ;
#36788 = CARTESIAN_POINT ( 'NONE',  ( -85.29374223801329435, -293.8620258123667668, -327.0984375345110493 ) ) ;
#36789 = CARTESIAN_POINT ( 'NONE',  ( -49.78861539303773043, -293.2053837619742467, -197.8779746303997058 ) ) ;
#36790 = CARTESIAN_POINT ( 'NONE',  ( -85.33152481854862970, -275.9090924074130839, -210.2361428286348826 ) ) ;
#36791 = DIRECTION ( 'NONE',  ( 0.000000000000000000, 1.000000000000000000, 0.000000000000000000 ) ) ;
#36792 = CARTESIAN_POINT ( 'NONE',  ( -25.03884946062321504, -293.3780089964228637, -345.7230450274479381 ) ) ;
#36793 = CARTESIAN_POINT ( 'NONE',  ( 34.48434176199818779, -289.3735293157934052, -287.3157670210113110 ) ) ;
#36794 = CARTESIAN_POINT ( 'NONE',  ( -109.8221491066610866, -288.4995110242126657, -293.3489331880157920 ) ) ;
#36795 = CARTESIAN_POINT ( 'NONE',  ( 18.28274548461518734, -289.6591956413274147, -318.6172661711337355 ) ) ;
#36796 = DIRECTION ( 'NONE',  ( 1.000000000000000000, 0.000000000000000000, -0.000000000000000000 ) ) ;
#36797 = CARTESIAN_POINT ( 'NONE',  ( -71.23851263373516929, -290.3144726487295202, -335.2105069138991666 ) ) ;
#36798 = DIRECTION ( 'NONE',  ( -0.000000000000000000, -0.000000000000000000, -1.000000000000000000 ) ) ;
#36799 = CARTESIAN_POINT ( 'NONE',  ( 19.34082124355152743, -289.4612870093533843, -321.9083279324900104 ) ) ;
#36800 = CARTESIAN_POINT ( 'NONE',  ( -104.6939055459116759, -277.0178205906348694, -236.4501987292175045 ) ) ;
#36801 = CARTESIAN_POINT ( 'NONE',  ( -62.04486340233327013, -280.0729714785089755, -197.3974378045095364 ) ) ;
#36802 = CARTESIAN_POINT ( 'NONE',  ( 37.96486863945008849, -281.0184492793648019, -254.3398145777974264 ) ) ;
#36803 = CARTESIAN_POINT ( 'NONE',  ( 16.48206017951068958, -284.8170321380278551, -218.1308252914413686 ) ) ;
#36804 = CARTESIAN_POINT ( 'NONE',  ( -112.3417001281054297, -274.5519904173220311, -270.3865538441530134 ) ) ;
#36805 = CARTESIAN_POINT ( 'NONE',  ( -67.79164321634486612, -277.7878204436214560, -202.6445037518199399 ) ) ;
#36806 = EDGE_CURVE ( 'NONE', #26725, #36954, #18980, .T. ) ;
#36807 = CARTESIAN_POINT ( 'NONE',  ( -37.34053867939269367, -281.0519445936344027, -345.3738477710438133 ) ) ;
#36808 = CARTESIAN_POINT ( 'NONE',  ( 197.1939413472297531, 281.6276417382965178, -110.3312367469949464 ) ) ;
#36809 = CARTESIAN_POINT ( 'NONE',  ( -92.84312659188438488, -276.3098641460309750, -322.8039304740246962 ) ) ;
#36810 = CARTESIAN_POINT ( 'NONE',  ( -102.2495113585714250, -284.0095371113371812, -229.5142264162927006 ) ) ;
#36811 = CARTESIAN_POINT ( 'NONE',  ( -54.25877517958490159, -274.6320935663379714, -199.1823690604259411 ) ) ;
#36812 = CARTESIAN_POINT ( 'NONE',  ( -93.17494621273786493, -292.8324584107060105, -222.1004813491875893 ) ) ;
#36813 = CARTESIAN_POINT ( 'NONE',  ( 30.22961323696181068, -300.1966590518934481, -193.8395018425161709 ) ) ;
#36814 = CARTESIAN_POINT ( 'NONE',  ( 25.29614986399421284, -274.7016079911401789, -232.7320200206928007 ) ) ;
#36815 = CARTESIAN_POINT ( 'NONE',  ( 7.272559309870788802, -296.4447451376365166, -330.7132379572404943 ) ) ;
#36816 = CARTESIAN_POINT ( 'NONE',  ( -8.231165223220649807, -288.8480277823040865, -341.6605635237885963 ) ) ;
#36817 = VECTOR ( 'NONE', #7329, 1000.000000000000000 ) ;
#36818 = CARTESIAN_POINT ( 'NONE',  ( 12.06932601694004248, -278.8129495320926594, -213.1958777518001682 ) ) ;
#36819 = CARTESIAN_POINT ( 'NONE',  ( -37.79290030657497113, -291.8799680262281413, -193.3624399228993411 ) ) ;
#36821 = EDGE_CURVE ( 'NONE', #24854, #31130, #3835, .T. ) ;
#36820 = CARTESIAN_POINT ( 'NONE',  ( -109.1718583294079679, -289.4223191808246156, -284.7024570135646400 ) ) ;
#36822 = AXIS2_PLACEMENT_3D ( 'NONE', #52500, #52964, #81377 ) ;
#36823 = CARTESIAN_POINT ( 'NONE',  ( 26.39254997012500326, -292.0839678361840015, -309.9927494513522674 ) ) ;
#36824 = ORIENTED_EDGE ( 'NONE', *, *, #47352, .T. ) ;
#36825 = CARTESIAN_POINT ( 'NONE',  ( 197.3616393129065898, 72.09241014521839475, 11.67163425240527452 ) ) ;
#36826 = TOROIDAL_SURFACE ( 'NONE', #36752, 24.50000000000000355, 0.5000000000000000000 ) ;
#36827 = CARTESIAN_POINT ( 'NONE',  ( -107.0126802088411182, -289.7664392164821265, -292.5272007342535403 ) ) ;
#36828 = CARTESIAN_POINT ( 'NONE',  ( 185.8264795993290193, 250.5000000000000568, 23.09031830825835385 ) ) ;
#36829 = CARTESIAN_POINT ( 'NONE',  ( 18.17302546201613467, -287.7654569333693075, -217.2662141498794028 ) ) ;
#36830 = CARTESIAN_POINT ( 'NONE',  ( -53.35057174420112602, -294.3376638359845288, -200.3683826091709648 ) ) ;
#36831 = CARTESIAN_POINT ( 'NONE',  ( -44.78477869464024508, -294.2027940696279416, -346.8173774530810078 ) ) ;
#36832 = CARTESIAN_POINT ( 'NONE',  ( -34.48053704472732051, -284.3320607180696129, -346.8144502818275896 ) ) ;
#36833 = CARTESIAN_POINT ( 'NONE',  ( -72.37214735263843579, -285.4082075762343038, -206.3010760867753390 ) ) ;
#36834 = CIRCLE ( 'NONE', #71667, 0.5000000000000004441 ) ;
#36835 = CARTESIAN_POINT ( 'NONE',  ( 0.8545650129210551338, -275.8885338214997773, -207.5734694588424247 ) ) ;
#36836 = CARTESIAN_POINT ( 'NONE',  ( -20.50106539893686275, -292.8550685056684415, -343.1346769554493790 ) ) ;
#36837 = UNCERTAINTY_MEASURE_WITH_UNIT (LENGTH_MEASURE( 1.000000000000000082E-05 ), #76509, 'distance_accuracy_value', 'NONE');
#36838 = CARTESIAN_POINT ( 'NONE',  ( 35.23659445264143386, -274.2025218373474900, -259.3438418468474538 ) ) ;
#36839 = EDGE_LOOP ( 'NONE', ( #77606, #15709, #75972, #24644 ) ) ;
#36840 = CARTESIAN_POINT ( 'NONE',  ( 196.0351550650564434, 41.34106363718652943, 11.96389409883855848 ) ) ;
#36841 = CARTESIAN_POINT ( 'NONE',  ( -65.59968739739146315, -295.0784319070454558, -341.9800181438119466 ) ) ;
#36842 = CARTESIAN_POINT ( 'NONE',  ( -52.40372891949215273, -287.7779160959167370, -197.4608471762732904 ) ) ;
#36843 = AXIS2_PLACEMENT_3D ( 'NONE', #29822, #42607, #71522 ) ;
#36844 = CARTESIAN_POINT ( 'NONE',  ( -107.4958552754885943, -298.0301750027059029, -239.2477230367415757 ) ) ;
#36845 = CARTESIAN_POINT ( 'NONE',  ( 33.80760680919627248, -287.9817675162150294, -253.5240536369941537 ) ) ;
#36846 = CARTESIAN_POINT ( 'NONE',  ( -80.10508841278016234, -276.6740518776620661, -334.1755084955324264 ) ) ;
#36847 = CARTESIAN_POINT ( 'NONE',  ( 4.179250514901015734, -295.1600395455890862, -335.1487979821375234 ) ) ;
#36848 = CARTESIAN_POINT ( 'NONE',  ( -96.34334640992992149, -288.0440245773420429, -317.9116936895005097 ) ) ;
#36849 = CARTESIAN_POINT ( 'NONE',  ( 6.605412711137148563, -294.8062076753766974, -333.6273014008230007 ) ) ;
#36850 = CARTESIAN_POINT ( 'NONE',  ( -32.16002058906382643, -292.4525599200878219, -197.5114314398128101 ) ) ;
#36851 = DIRECTION ( 'NONE',  ( 0.000000000000000000, 0.000000000000000000, -1.000000000000000000 ) ) ;
#36852 = VECTOR ( 'NONE', #42959, 1000.000000000000000 ) ;
#36853 = DIRECTION ( 'NONE',  ( 1.000000000000000000, 0.000000000000000000, 0.000000000000000000 ) ) ;
#36854 = CARTESIAN_POINT ( 'NONE',  ( 174.1105135456032542, 240.3386868885705496, -177.2113801462826643 ) ) ;
#36855 = CARTESIAN_POINT ( 'NONE',  ( 33.21091871336700052, -288.6979250818966420, -241.1536667946379566 ) ) ;
#36856 = CARTESIAN_POINT ( 'NONE',  ( -111.2586520408596868, -282.4809262143061233, -234.7283546768995564 ) ) ;
#36857 = EDGE_LOOP ( 'NONE', ( #18090, #39877 ) ) ;
#36858 = CARTESIAN_POINT ( 'NONE',  ( -14.25045192895701263, -279.6923947753392099, -196.9560768477662123 ) ) ;
#36859 = CARTESIAN_POINT ( 'NONE',  ( -43.04791768223248738, -285.1243805308062633, -345.0279269821415937 ) ) ;
#36860 = CARTESIAN_POINT ( 'NONE',  ( -49.23497188951420611, -284.4782885979726075, -194.8282850317589237 ) ) ;
#36861 = CARTESIAN_POINT ( 'NONE',  ( -70.63810939896589502, -287.5745296107767786, -336.9535029898096354 ) ) ;
#36862 = CARTESIAN_POINT ( 'NONE',  ( 22.64019871995547462, -276.7844792345271685, -224.0531067116369570 ) ) ;
#36863 = AXIS2_PLACEMENT_3D ( 'NONE', #88858, #24007, #16910 ) ;
#36864 = CARTESIAN_POINT ( 'NONE',  ( -44.58141681695952485, -298.4505642652458732, -197.6087337851072334 ) ) ;
#36865 = CARTESIAN_POINT ( 'NONE',  ( -39.72167468022215076, -293.7674540402812795, -343.8282385825488063 ) ) ;
#36866 = CARTESIAN_POINT ( 'NONE',  ( -86.74559198605830090, -280.0376532944069368, -211.3632058533457894 ) ) ;
#36868 = CARTESIAN_POINT ( 'NONE',  ( -110.0666238457801853, -278.0047955269531030, -262.4617719167286509 ) ) ;
#36867 = CARTESIAN_POINT ( 'NONE',  ( 34.70715861495462207, -275.7111269127703395, -282.4122724066306773 ) ) ;
#36869 = CARTESIAN_POINT ( 'NONE',  ( -24.22605246357979780, -275.2953893996891566, -194.7461205898380854 ) ) ;
#36870 = CARTESIAN_POINT ( 'NONE',  ( -4.141159238860603331, -275.5449661269385615, -339.5074353515473149 ) ) ;
#36871 = CARTESIAN_POINT ( 'NONE',  ( 153.3814170967218615, 207.2574094406980976, -217.2232996820281130 ) ) ;
#36872 = CARTESIAN_POINT ( 'NONE',  ( -59.62836778256614423, -275.3404975800690977, -342.0270585912988395 ) ) ;
#36873 = CARTESIAN_POINT ( 'NONE',  ( -113.3551985198493668, -297.8793511262754237, -278.1427858135329529 ) ) ;
#36874 = CARTESIAN_POINT ( 'NONE',  ( 10.64812456238590066, -278.9090924074130839, -330.4860931364851808 ) ) ;
#36875 = CARTESIAN_POINT ( 'NONE',  ( -69.18520112214993389, -196.4157418647702968, -356.4528236438462159 ) ) ;
#36876 = CARTESIAN_POINT ( 'NONE',  ( -33.23503331000667060, -287.1846106216869998, -197.1170884104619461 ) ) ;
#36877 = CARTESIAN_POINT ( 'NONE',  ( -35.19956408150198257, -287.8388036625057111, -194.3916777255585941 ) ) ;
#36878 = CARTESIAN_POINT ( 'NONE',  ( -38.61837901735849954, -285.3843446657514278, -197.2578343958313667 ) ) ;
#36879 = CARTESIAN_POINT ( 'NONE',  ( -99.86356443370645763, -276.4153224812768030, -309.6670332139806874 ) ) ;
#36880 = CARTESIAN_POINT ( 'NONE',  ( -100.6752999083492739, -286.9384364619213557, -231.5369026772743837 ) ) ;
#36881 = CARTESIAN_POINT ( 'NONE',  ( -109.2793814135444421, -277.2416644144022939, -254.3134942990032528 ) ) ;
#36882 = CARTESIAN_POINT ( 'NONE',  ( -1.213292271919899745, -277.8776866301691939, -334.4185682969979894 ) ) ;
#36883 = CARTESIAN_POINT ( 'NONE',  ( 35.66376543588182813, -276.0965471303533718, -274.3097109336476365 ) ) ;
#36884 = CARTESIAN_POINT ( 'NONE',  ( 36.75640753453114229, -286.5915451010758375, -289.7899409132114101 ) ) ;
#36885 = CARTESIAN_POINT ( 'NONE',  ( 39.45873257429219905, -282.3853018712736116, -272.7802824541742552 ) ) ;
#36886 = CARTESIAN_POINT ( 'NONE',  ( 38.81125129804725304, -282.1817532547462974, -281.3271971504478302 ) ) ;
#36887 = ORIENTED_EDGE ( 'NONE', *, *, #60388, .T. ) ;
#36888 = ORIENTED_EDGE ( 'NONE', *, *, #42791, .F. ) ;
#36889 = CARTESIAN_POINT ( 'NONE',  ( 195.8507069399275053, 41.77510181472468531, 14.13525600223613310 ) ) ;
#36890 = CARTESIAN_POINT ( 'NONE',  ( 18.72638111791853177, -290.1165214094963289, -321.3380371559483137 ) ) ;
#36891 = CARTESIAN_POINT ( 'NONE',  ( -106.8056060178617344, -289.6512339624493961, -238.1715188204582603 ) ) ;
#36892 = CARTESIAN_POINT ( 'NONE',  ( -67.14230893970606928, -272.7103626360679982, -203.4494586486582932 ) ) ;
#36893 = CARTESIAN_POINT ( 'NONE',  ( 6.445004935181720462, -291.9787336868825491, -207.1469008630812141 ) ) ;
#36894 = CARTESIAN_POINT ( 'NONE',  ( 20.06739938321959116, -285.3847274916469701, -224.1361075000812377 ) ) ;
#36895 = CARTESIAN_POINT ( 'NONE',  ( 35.52023449991650494, -288.8733082969592942, -279.2080941264615035 ) ) ;
#36896 = CARTESIAN_POINT ( 'NONE',  ( -85.33152481854864391, -299.9090924074131408, -210.2361428286349110 ) ) ;
#36897 = TOROIDAL_SURFACE ( 'NONE', #89789, 204.0731808058633590, 35.00000000000000000 ) ;
#36898 = CARTESIAN_POINT ( 'NONE',  ( -41.62032255882137122, -291.1061843189511933, -345.2518576254083769 ) ) ;
#36899 = CARTESIAN_POINT ( 'NONE',  ( -108.1473928269375193, -288.2239917012337287, -295.7461585387530931 ) ) ;
#36900 = CARTESIAN_POINT ( 'NONE',  ( -9.649097243101797616, -290.6905552127029750, -340.0750330642770791 ) ) ;
#36901 = CARTESIAN_POINT ( 'NONE',  ( -94.46102003390205937, -284.8475454532908202, -316.2154575172493765 ) ) ;
#36902 = CARTESIAN_POINT ( 'NONE',  ( -111.1302534931136705, -292.7367265589002159, -255.9664317823821023 ) ) ;
#36903 = CARTESIAN_POINT ( 'NONE',  ( 82.13382245134783943, -300.7353340821118195, -193.7454283942308280 ) ) ;
#36904 = CARTESIAN_POINT ( 'NONE',  ( 153.6949411230407918, 20.34881949282723923, -12.70049028465532182 ) ) ;
#36905 = VECTOR ( 'NONE', #72898, 1000.000000000000000 ) ;
#36906 = CARTESIAN_POINT ( 'NONE',  ( -29.27652873796473187, -300.0725136216683495, -194.7984956000887280 ) ) ;
#36907 = CARTESIAN_POINT ( 'NONE',  ( -26.72943433756234910, -282.1110169046190208, -342.8002470040619869 ) ) ;
#36908 = CARTESIAN_POINT ( 'NONE',  ( -94.08863254628134598, -281.8717741505666368, -319.4192907530908769 ) ) ;
#36909 = CARTESIAN_POINT ( 'NONE',  ( 8.801014963468832164, -293.6344376790679007, -331.8022171262888946 ) ) ;
#36910 = CARTESIAN_POINT ( 'NONE',  ( -104.1097020931474617, -271.2180401522759894, -238.4235550751121764 ) ) ;
#36911 = CARTESIAN_POINT ( 'NONE',  ( 29.30914618979764441, -274.0741951566227499, -303.6280945954125059 ) ) ;
#36912 = CARTESIAN_POINT ( 'NONE',  ( -80.02799379651372647, -298.7759356325807403, -210.5353391772223119 ) ) ;
#36913 = CARTESIAN_POINT ( 'NONE',  ( 183.0442525570908288, 296.7472757692770529, -7.499999999999996447 ) ) ;
#36915 = CARTESIAN_POINT ( 'NONE',  ( -105.5931858780995896, -295.2266800366576263, -236.9588919460001932 ) ) ;
#36914 = CIRCLE ( 'NONE', #64195, 16.36528803885689598 ) ;
#36916 = AXIS2_PLACEMENT_3D ( 'NONE', #43824, #15904, #80286 ) ;
#36917 = CARTESIAN_POINT ( 'NONE',  ( 20.16551058940973817, -295.6210030010713012, -316.2973931938221313 ) ) ;
#36918 = EDGE_CURVE ( 'NONE', #75392, #52994, #77675, .T. ) ;
#36919 = CARTESIAN_POINT ( 'NONE',  ( 175.2296996224750103, 160.0000000000000568, -10.55076157886938937 ) ) ;
#36920 = CARTESIAN_POINT ( 'NONE',  ( -63.61746002073931550, -296.2063128363726037, -338.6949943381572439 ) ) ;
#36921 = CARTESIAN_POINT ( 'NONE',  ( 150.8012326218627948, 131.0000000000000568, 11.50000000000000000 ) ) ;
#36923 = CARTESIAN_POINT ( 'NONE',  ( -104.9619019494661245, -296.1837140179526386, -297.8658140476903782 ) ) ;
#36922 = CARTESIAN_POINT ( 'NONE',  ( -94.55095229357320363, -283.2492345915375154, -221.2369024467940903 ) ) ;
#36924 = AXIS2_PLACEMENT_3D ( 'NONE', #69727, #6271, #26165 ) ;
#36925 = CARTESIAN_POINT ( 'NONE',  ( -111.4914709271562003, -284.2920650769411282, -291.1171168851585662 ) ) ;
#36926 = CARTESIAN_POINT ( 'NONE',  ( 16.81163618459275000, -284.2091697568932318, -323.1305958465078447 ) ) ;
#36927 = CARTESIAN_POINT ( 'NONE',  ( 24.68875090346103462, -286.6132069863242009, -224.7763898775358200 ) ) ;
#36928 = CARTESIAN_POINT ( 'NONE',  ( -44.44960301515508405, -289.9619948487066381, -195.8140171833827878 ) ) ;
#36929 = CARTESIAN_POINT ( 'NONE',  ( -14.26648824407761396, -279.5409997918751515, -197.0134952603672218 ) ) ;
#36930 = CARTESIAN_POINT ( 'NONE',  ( 31.95455697924147387, -273.4809262143061233, -303.7686719486574134 ) ) ;
#36931 = CARTESIAN_POINT ( 'NONE',  ( -48.18343439339133027, -265.6166469183335153, -497.0604155083543105 ) ) ;
#36932 = CARTESIAN_POINT ( 'NONE',  ( 22.32328254390262501, -285.7518421287712158, -227.5294096280811686 ) ) ;
#36933 = CARTESIAN_POINT ( 'NONE',  ( -102.0478770743834929, -288.9296200951868627, -311.6244275673911943 ) ) ;
#36934 = DIRECTION ( 'NONE',  ( 0.000000000000000000, 1.000000000000000000, 0.000000000000000000 ) ) ;
#36935 = CARTESIAN_POINT ( 'NONE',  ( -96.58593854714524696, -279.3246251290308919, -318.6384823448831867 ) ) ;
#36937 = CARTESIAN_POINT ( 'NONE',  ( 35.58682598292216426, -281.2673555978400373, -274.0377422451885536 ) ) ;
#36936 = CARTESIAN_POINT ( 'NONE',  ( -65.02326372284356637, -293.4320866481708094, -340.4616835367447152 ) ) ;
#36938 = CARTESIAN_POINT ( 'NONE',  ( -24.90572107143746550, -295.0645394442873908, -346.4043043483591759 ) ) ;
#36939 = CARTESIAN_POINT ( 'NONE',  ( 6.724355481774723309, -284.7256879460035748, -208.9167217821592430 ) ) ;
#36940 = EDGE_CURVE ( 'NONE', #13683, #61737, #25592, .T. ) ;
#36941 = CARTESIAN_POINT ( 'NONE',  ( -69.13826660988181061, -281.6341555427423486, -202.4208243649676717 ) ) ;
#36942 = CARTESIAN_POINT ( 'NONE',  ( -110.2835078175194070, -295.7042042218030815, -263.2649739798760038 ) ) ;
#36943 = ORIENTED_EDGE ( 'NONE', *, *, #81253, .T. ) ;
#36944 = CARTESIAN_POINT ( 'NONE',  ( 200.4871970924047275, 61.71654497091388691, -9.999999999999998224 ) ) ;
#36945 = CARTESIAN_POINT ( 'NONE',  ( 34.30644308138853660, -283.2611589842876469, -249.4233440177841601 ) ) ;
#36946 = DIRECTION ( 'NONE',  ( 0.9951408606192333473, 0.000000000000000000, -0.09846150276129089773 ) ) ;
#36947 = CARTESIAN_POINT ( 'NONE',  ( -82.08285599513421005, -294.9094976428775681, -214.2051214447836571 ) ) ;
#36948 = CARTESIAN_POINT ( 'NONE',  ( 22.63873250808064341, -274.1044569133171080, -222.3141468171702684 ) ) ;
#36949 = CARTESIAN_POINT ( 'NONE',  ( -109.6232494068969316, -290.2495149318017980, -280.6673531531192793 ) ) ;
#36950 = CARTESIAN_POINT ( 'NONE',  ( 14.42537766125526488, -283.8284502065166066, -322.8817930029990748 ) ) ;
#36951 = CARTESIAN_POINT ( 'NONE',  ( -24.47679064279848404, -275.8190786879782195, -197.6389279314454654 ) ) ;
#36952 = CARTESIAN_POINT ( 'NONE',  ( 6.481749951803364773, -284.0681167762502355, -332.7630064512111971 ) ) ;
#36953 = CARTESIAN_POINT ( 'NONE',  ( 34.32482175247959333, -280.5549554248458435, -286.2053645005437943 ) ) ;
#36954 = VERTEX_POINT ( 'NONE', #85241 ) ;
#36955 = CARTESIAN_POINT ( 'NONE',  ( -3.824187849458207555, -274.3154723379626603, -201.0243446290846521 ) ) ;
#36956 = CARTESIAN_POINT ( 'NONE',  ( 36.97054912080180600, -295.4054481140806843, -265.1924673239111030 ) ) ;
#36957 = DIRECTION ( 'NONE',  ( 0.000000000000000000, 0.000000000000000000, 1.000000000000000000 ) ) ;
#36958 = DIRECTION ( 'NONE',  ( 1.000000000000000000, 0.000000000000000000, 0.000000000000000000 ) ) ;
#36959 = CARTESIAN_POINT ( 'NONE',  ( 5.889451509615496683, -292.6128637411753743, -332.6453887780560876 ) ) ;
#36960 = CARTESIAN_POINT ( 'NONE',  ( -92.95655378125168511, -272.7333711148331190, -222.9606251350134301 ) ) ;
#36961 = CARTESIAN_POINT ( 'NONE',  ( 185.4166944662832179, 250.5000000000000568, 23.37680765314684450 ) ) ;
#36962 = CARTESIAN_POINT ( 'NONE',  ( -83.85915103086674094, -292.9469145962386278, -209.8062095858481655 ) ) ;
#36964 = CARTESIAN_POINT ( 'NONE',  ( 26.15512029855018383, -294.1886004579299083, -227.4173669537807712 ) ) ;
#36963 = CARTESIAN_POINT ( 'NONE',  ( -106.6662871844225293, -281.4805209788417528, -237.0123917617630980 ) ) ;
#36965 = CARTESIAN_POINT ( 'NONE',  ( -79.17879856468479716, -291.6177795230280481, -332.4693228246752597 ) ) ;
#36966 = CARTESIAN_POINT ( 'NONE',  ( -37.84707834972281404, -275.0583030169848371, -345.2055143726373103 ) ) ;
#36967 = CARTESIAN_POINT ( 'NONE',  ( -94.70027095998874245, -279.8124312193276069, -317.8290373671133580 ) ) ;
#36968 = CARTESIAN_POINT ( 'NONE',  ( -2.490811265811056607, -292.6672015917673662, -336.1389998699629587 ) ) ;
#36969 = CARTESIAN_POINT ( 'NONE',  ( 27.26432475088252616, -283.9392126661333009, -310.0379450181517313 ) ) ;
#36970 = VERTEX_POINT ( 'NONE', #48301 ) ;
#36971 = CARTESIAN_POINT ( 'NONE',  ( -95.13577766700244354, -283.5904542133199584, -315.0125967312922057 ) ) ;
#36972 = CARTESIAN_POINT ( 'NONE',  ( 5.998200796796139045, -281.7048132604465422, -207.0907023297529008 ) ) ;
#36973 = CARTESIAN_POINT ( 'NONE',  ( 34.21111404242772380, -280.6951801885720101, -297.7144267780789733 ) ) ;
#36974 = TOROIDAL_SURFACE ( 'NONE', #88330, 1.000000000000000000, 0.5000000000000000000 ) ;
#36975 = CARTESIAN_POINT ( 'NONE',  ( 10.38916068597229803, -277.3531791362818808, -330.5504237604178570 ) ) ;
#36976 = DIRECTION ( 'NONE',  ( 1.000000000000000000, 0.000000000000000000, 0.000000000000000000 ) ) ;
#36977 = CARTESIAN_POINT ( 'NONE',  ( 36.22242171068192818, -277.3291043189938136, -290.6837035835468441 ) ) ;
#36978 = CARTESIAN_POINT ( 'NONE',  ( -67.68488546085839630, -285.9805209788416391, -333.4427485647536855 ) ) ;
#36979 = ORIENTED_EDGE ( 'NONE', *, *, #72569, .F. ) ;
#36980 = CARTESIAN_POINT ( 'NONE',  ( -112.1750334612141984, -274.5519907627465273, -270.3865268295556348 ) ) ;
#36981 = CARTESIAN_POINT ( 'NONE',  ( -102.0203561698286876, -276.0713964293829008, -307.7278154579086049 ) ) ;
#36982 = CARTESIAN_POINT ( 'NONE',  ( -95.81366283558585906, -292.9736842513708552, -221.8126232103016946 ) ) ;
#36983 = CARTESIAN_POINT ( 'NONE',  ( -75.02505197771870371, -290.8847456637496407, -207.6613210053333205 ) ) ;
#36984 = CARTESIAN_POINT ( 'NONE',  ( 35.01245512179372099, -287.3922101514290262, -296.6771863954621722 ) ) ;
#36985 = CARTESIAN_POINT ( 'NONE',  ( 222.4306832106270804, -141.7221692137691775, 21.50000000000000000 ) ) ;
#36987 = CARTESIAN_POINT ( 'NONE',  ( -105.3266632753537522, -283.3347995887914976, -241.5160031345323262 ) ) ;
#36986 = CARTESIAN_POINT ( 'NONE',  ( 36.14253679120695750, -291.8617747428961593, -249.3688743060224908 ) ) ;
#36988 = CARTESIAN_POINT ( 'NONE',  ( -109.3117356732567629, -292.6493620579727803, -252.1110151878432362 ) ) ;
#36989 = CARTESIAN_POINT ( 'NONE',  ( -104.1054789661079951, -283.4507865373743698, -239.0423711642947922 ) ) ;
#36990 = CARTESIAN_POINT ( 'NONE',  ( 27.29668544199265767, -283.3412964415218198, -305.3342875222486441 ) ) ;
#36991 = CARTESIAN_POINT ( 'NONE',  ( -107.5114081177776910, -291.0934486694390557, -301.6210938016452019 ) ) ;
#36992 = CARTESIAN_POINT ( 'NONE',  ( -4.325365113249699967, -280.9918637714453098, -205.1712226753450921 ) ) ;
#36993 = CARTESIAN_POINT ( 'NONE',  ( 31.83402857222822391, -291.9217358041721582, -237.3329715404935598 ) ) ;
#36994 = CIRCLE ( 'NONE', #26449, 2.738891987356051327 ) ;
#36995 = CARTESIAN_POINT ( 'NONE',  ( 39.41572584169161075, -288.2980425069398507, -265.8177318945975003 ) ) ;
#36996 = CARTESIAN_POINT ( 'NONE',  ( 24.09685428922209738, -288.6616747870603490, -316.6734374510982093 ) ) ;
#36997 = CARTESIAN_POINT ( 'NONE',  ( -2.188249144733531715, -286.6975704660616771, -206.3260084878871226 ) ) ;
#36998 = ORIENTED_EDGE ( 'NONE', *, *, #38856, .T. ) ;
#36999 = CARTESIAN_POINT ( 'NONE',  ( 194.6960821673052919, 25.58662921606750018, 14.03832098086475710 ) ) ;
#37000 = CARTESIAN_POINT ( 'NONE',  ( 38.47554935220361472, -295.4116289293041859, -270.2871325723973541 ) ) ;
#37001 = CARTESIAN_POINT ( 'NONE',  ( -36.29808382088275920, -293.7241940474278294, -346.8738709653217143 ) ) ;
#37002 = CARTESIAN_POINT ( 'NONE',  ( -108.7182843014649336, -277.3945864456988488, -286.8116003028404748 ) ) ;
#37003 = CARTESIAN_POINT ( 'NONE',  ( -87.38962092380074864, -296.7242667153077491, -211.9084106621063484 ) ) ;
#37004 = CARTESIAN_POINT ( 'NONE',  ( 33.98410035876713664, -291.7897037976191541, -251.8317375574839048 ) ) ;
#37005 = CARTESIAN_POINT ( 'NONE',  ( -8.597701657243348450, -276.1935715257366155, -202.1026798337757100 ) ) ;
#37006 = CARTESIAN_POINT ( 'NONE',  ( -104.6306431716327552, -295.2035005546922548, -239.4129797224479148 ) ) ;
#37007 = CARTESIAN_POINT ( 'NONE',  ( 26.57282121197138380, -294.2647322262678813, -234.1732512066087111 ) ) ;
#37008 = CARTESIAN_POINT ( 'NONE',  ( 30.87824537295921701, -294.9908543258464988, -297.3378299978240307 ) ) ;
#37009 = CARTESIAN_POINT ( 'NONE',  ( -43.54160339317392214, -248.0334966641272842, -463.3306390303819740 ) ) ;
#37010 = CARTESIAN_POINT ( 'NONE',  ( 27.96881088667049298, -292.0482342388298775, -307.6759528381567179 ) ) ;
#37011 = CARTESIAN_POINT ( 'NONE',  ( -53.44865136905574587, -290.2051414032908951, -341.8032243980975977 ) ) ;
#37012 = CARTESIAN_POINT ( 'NONE',  ( -12.99719401820812870, -295.0603300179528219, -339.2579291907965171 ) ) ;
#37013 = CARTESIAN_POINT ( 'NONE',  ( -109.7636072712097217, -280.7987700860118707, -249.5410754765287891 ) ) ;
#37014 = CARTESIAN_POINT ( 'NONE',  ( -112.2313437181619662, -277.4347271936559309, -254.6506584485609324 ) ) ;
#37015 = CARTESIAN_POINT ( 'NONE',  ( 9.454885671036437955, -274.0253381202152809, -209.3415117578530840 ) ) ;
#37016 = CARTESIAN_POINT ( 'NONE',  ( -70.88528326492306064, -281.5780024296843749, -336.8294352962802805 ) ) ;
#37017 = CARTESIAN_POINT ( 'NONE',  ( -113.2450508922976695, -277.0441683364643382, -263.0699910422949301 ) ) ;
#37018 = CARTESIAN_POINT ( 'NONE',  ( -28.41678812943368371, -278.1648302364130814, -195.6738277291115367 ) ) ;
#37019 = EDGE_CURVE ( 'NONE', #2276, #62468, #76734, .T. ) ;
#37020 = CARTESIAN_POINT ( 'NONE',  ( -98.32135777670937671, -271.6959551582586982, -229.0773264192933425 ) ) ;
#37021 = CARTESIAN_POINT ( 'NONE',  ( 27.60217406688886399, -277.0503887539096013, -232.7446843780067809 ) ) ;
#37022 = CARTESIAN_POINT ( 'NONE',  ( 195.2074068093847075, 24.86248909206367941, 13.30112067542677146 ) ) ;
#37023 = CARTESIAN_POINT ( 'NONE',  ( -91.60967520620930316, -289.3043573793663654, -218.0050431614291711 ) ) ;
#37024 = CARTESIAN_POINT ( 'NONE',  ( -112.6399703681933602, -290.7542311198969855, -254.2001374818672161 ) ) ;
#37025 = CARTESIAN_POINT ( 'NONE',  ( -41.12656548946259960, -276.0049114333808689, -195.2387825725652988 ) ) ;
#37026 = CARTESIAN_POINT ( 'NONE',  ( -92.57874459094192332, -271.2609296130669918, -219.6087962519301300 ) ) ;
#37027 = CARTESIAN_POINT ( 'NONE',  ( -109.1556968857388341, -283.4009858888555868, -297.8390650868544185 ) ) ;
#37028 = DIRECTION ( 'NONE',  ( 0.000000000000000000, 0.000000000000000000, -1.000000000000000000 ) ) ;
#37029 = CARTESIAN_POINT ( 'NONE',  ( -28.31812375890616096, -280.9376230016517866, -344.8679413759246586 ) ) ;
#37030 = CARTESIAN_POINT ( 'NONE',  ( 197.7335303680046650, 24.96166607582782859, 12.00000000000001599 ) ) ;
#37031 = CARTESIAN_POINT ( 'NONE',  ( -38.89065619811597685, -290.8272126874965693, -196.9803899876711739 ) ) ;
#37032 = CARTESIAN_POINT ( 'NONE',  ( -60.33916665240547417, -283.8903411549292173, -199.7779612652877006 ) ) ;
#37033 = CARTESIAN_POINT ( 'NONE',  ( 195.3536225096696342, 25.92713179672681179, 14.83384749020537718 ) ) ;
#37034 = CYLINDRICAL_SURFACE ( 'NONE', #18572, 25.00000000000000355 ) ;
#37035 = CARTESIAN_POINT ( 'NONE',  ( -11.54911720562293631, -290.3877722157725998, -199.8803114367731837 ) ) ;
#37036 = CARTESIAN_POINT ( 'NONE',  ( -64.60998207719204345, -279.0141852448809914, -338.9929373764626348 ) ) ;
#37037 = CARTESIAN_POINT ( 'NONE',  ( -58.36297363748835920, -284.5229353502094796, -344.0784934699102564 ) ) ;
#37039 = CARTESIAN_POINT ( 'NONE',  ( -17.17187656040842469, -286.3197412667005892, -200.1500332567303815 ) ) ;
#37038 = CARTESIAN_POINT ( 'NONE',  ( 37.30883395524732293, -273.4819731783036332, -258.5894353023925305 ) ) ;
#37040 = CARTESIAN_POINT ( 'NONE',  ( 1.195336417150171027, -277.9522902252868448, -333.1128814005253389 ) ) ;
#37041 = CARTESIAN_POINT ( 'NONE',  ( -29.68638422648549735, -277.7557249646909554, -343.1720013271563516 ) ) ;
#37042 = EDGE_CURVE ( 'NONE', #33465, #50614, #20389, .T. ) ;
#37043 = EDGE_CURVE ( 'NONE', #66639, #20110, #18660, .T. ) ;
#37044 = CARTESIAN_POINT ( 'NONE',  ( -105.1853664718594104, -286.1318357377056145, -302.3335683525842228 ) ) ;
#37045 = EDGE_LOOP ( 'NONE', ( #48702, #47761, #19120 ) ) ;
#37046 = CARTESIAN_POINT ( 'NONE',  ( 208.6208076322478746, 32.98517505407394168, 10.50000000000000000 ) ) ;
#37047 = CARTESIAN_POINT ( 'NONE',  ( -88.60701418124442341, -295.5810413484387027, -327.8857968831457015 ) ) ;
#37048 = CARTESIAN_POINT ( 'NONE',  ( -15.34337880032020962, -290.7460032282443194, -341.7448019072086254 ) ) ;
#37049 = DIRECTION ( 'NONE',  ( 0.000000000000000000, 0.000000000000000000, -1.000000000000000000 ) ) ;
#37050 =( GEOMETRIC_REPRESENTATION_CONTEXT ( 3 ) GLOBAL_UNCERTAINTY_ASSIGNED_CONTEXT ( ( #65568 ) ) GLOBAL_UNIT_ASSIGNED_CONTEXT ( ( #41729, #13350, #533 ) ) REPRESENTATION_CONTEXT ( 'NONE', 'WORKASPACE' ) );
#37051 = CARTESIAN_POINT ( 'NONE',  ( -2.659677404128715672, -276.9805209788415823, -198.2697987213421698 ) ) ;
#37052 = CARTESIAN_POINT ( 'NONE',  ( -42.39589846619059443, -278.9101452985017886, -193.8369545496461797 ) ) ;
#37053 = CARTESIAN_POINT ( 'NONE',  ( 3.778266276815157809, -292.9088607313422017, -334.5760871410036543 ) ) ;
#37054 = CARTESIAN_POINT ( 'NONE',  ( -22.33740751207839281, -287.7677717395167178, -198.1590493296342856 ) ) ;
#37055 = VECTOR ( 'NONE', #85639, 1000.000000000000000 ) ;
#37056 = CARTESIAN_POINT ( 'NONE',  ( -110.2809383260595837, -280.1478595245853285, -282.9993998429006297 ) ) ;
#37057 = CARTESIAN_POINT ( 'NONE',  ( 37.70801145274374022, -288.7964701229394677, -256.0032948246492310 ) ) ;
#37058 = CARTESIAN_POINT ( 'NONE',  ( -77.16815995366074787, -285.5857159162177936, -333.9745020412080407 ) ) ;
#37059 = CARTESIAN_POINT ( 'NONE',  ( -109.6069270068814632, -279.0565546539431239, -243.6226454669128998 ) ) ;
#37060 = CARTESIAN_POINT ( 'NONE',  ( -72.41605985728138251, -295.6057489726476888, -204.4555097736812570 ) ) ;
#37061 = CARTESIAN_POINT ( 'NONE',  ( 36.02963489785773987, -291.4018435801146438, -252.3067169072024001 ) ) ;
#37062 = CARTESIAN_POINT ( 'NONE',  ( -75.00608125737090859, -279.3980205264095389, -203.2016480720518814 ) ) ;
#37063 = CARTESIAN_POINT ( 'NONE',  ( -105.5234224581892590, -274.8020826622042136, -240.8689019982741115 ) ) ;
#37064 = CARTESIAN_POINT ( 'NONE',  ( 155.0741174296433371, 18.62644422905808383, 11.41100038914543902 ) ) ;
#37065 = CARTESIAN_POINT ( 'NONE',  ( -95.95921662488163406, -286.4090924074130839, -317.1477375740089997 ) ) ;
#37066 = CARTESIAN_POINT ( 'NONE',  ( -18.77557742772152594, -272.5277445104795220, -196.6232070001437080 ) ) ;
#37067 = DIRECTION ( 'NONE',  ( 1.000000000000000000, -0.000000000000000000, 0.000000000000000000 ) ) ;
#37068 = CARTESIAN_POINT ( 'NONE',  ( -89.51313367784943864, -278.8002414177943251, -219.1413082511308801 ) ) ;
#37069 = CARTESIAN_POINT ( 'NONE',  ( 31.50518791976868016, -277.1920656444571591, -304.0694068053545607 ) ) ;
#37070 = CARTESIAN_POINT ( 'NONE',  ( -93.20344372429528335, -298.6540565034932229, -222.4372358611114464 ) ) ;
#37071 = CARTESIAN_POINT ( 'NONE',  ( -58.43364339371257898, -282.3769531223773583, -344.2266799187236188 ) ) ;
#37072 = CARTESIAN_POINT ( 'NONE',  ( 35.00591514310363550, -289.5161752955698944, -286.0346310265603620 ) ) ;
#37073 = CARTESIAN_POINT ( 'NONE',  ( 18.73489159201515974, -300.2623009399910075, -194.0402399066217640 ) ) ;
#37074 = CARTESIAN_POINT ( 'NONE',  ( -68.03254280119637087, -298.8632833253699346, -200.1185621499464276 ) ) ;
#37075 = CARTESIAN_POINT ( 'NONE',  ( -42.49107612656045774, -297.1174249618367753, -345.0170779197919160 ) ) ;
#37076 = CARTESIAN_POINT ( 'NONE',  ( 19.88017639712701268, -280.2205166894802915, -318.6063603022816437 ) ) ;
#37077 = CARTESIAN_POINT ( 'NONE',  ( -51.85716681453614285, -271.8857467313417828, -197.0883042514022918 ) ) ;
#37078 = CARTESIAN_POINT ( 'NONE',  ( 24.04655775694280351, -288.5463040692736740, -225.2177661935517676 ) ) ;
#37079 = CARTESIAN_POINT ( 'NONE',  ( -48.11995633477735623, -288.1126874506833815, -342.9248059595465747 ) ) ;
#37080 = CARTESIAN_POINT ( 'NONE',  ( -108.9069067375272795, -267.5952716126691371, -307.0082179899138737 ) ) ;
#37081 = ORIENTED_EDGE ( 'NONE', *, *, #80410, .F. ) ;
#37082 = CARTESIAN_POINT ( 'NONE',  ( -71.65823418849379323, -288.0714155168222419, -338.6325013365311634 ) ) ;
#37083 = CARTESIAN_POINT ( 'NONE',  ( 34.03044012539324115, -287.4230921559598073, -285.8503994474906449 ) ) ;
#37084 = ORIENTED_EDGE ( 'NONE', *, *, #93228, .T. ) ;
#37085 = CARTESIAN_POINT ( 'NONE',  ( -23.85383805456077155, -287.3001291021022894, -194.8116234015328416 ) ) ;
#37086 = CARTESIAN_POINT ( 'NONE',  ( -35.11273941336074245, -277.3566764664938091, -343.3482347976537881 ) ) ;
#37087 = CARTESIAN_POINT ( 'NONE',  ( -3.445535714056276788, -291.4094686568123507, -201.5531595875512210 ) ) ;
#37088 = CARTESIAN_POINT ( 'NONE',  ( 30.62782783204197656, -281.7372433270249417, -234.2829683179864446 ) ) ;
#37089 = CARTESIAN_POINT ( 'NONE',  ( -3.978391424313769242, -282.0042829910108821, -201.7202262214031521 ) ) ;
#37090 = CARTESIAN_POINT ( 'NONE',  ( -50.08582698513463782, -283.5436691762438386, -346.3315869451657250 ) ) ;
#37091 = CARTESIAN_POINT ( 'NONE',  ( 35.37298409981235636, -281.7902707737217156, -263.1450363258826997 ) ) ;
#37092 = CARTESIAN_POINT ( 'NONE',  ( 84.90983274801601510, 83.18529645481817170, -302.4082324711995398 ) ) ;
#37093 = CARTESIAN_POINT ( 'NONE',  ( -111.7927560011644914, -280.6559419418501307, -262.3084274197423156 ) ) ;
#37094 = CARTESIAN_POINT ( 'NONE',  ( 188.3549636017863520, 271.3458732071474060, -139.1533289483813576 ) ) ;
#37095 = CARTESIAN_POINT ( 'NONE',  ( -56.56367322532989306, -168.9367680551909814, -360.8783654570042927 ) ) ;
#37096 = CARTESIAN_POINT ( 'NONE',  ( -65.86669663844585898, -272.8663103139484178, -202.9895638861965210 ) ) ;
#37097 = CARTESIAN_POINT ( 'NONE',  ( 37.02471903805842857, -292.8120597285326312, -250.5830679493484183 ) ) ;
#37098 = CARTESIAN_POINT ( 'NONE',  ( 189.7233545045971539, 267.9684856506630126, -137.6739583361996040 ) ) ;
#37100 = CARTESIAN_POINT ( 'NONE',  ( -26.37592589864985726, -287.3102865826921857, -343.3934915310548490 ) ) ;
#37099 = CARTESIAN_POINT ( 'NONE',  ( -29.87027394958076698, -272.8296904090437351, -194.2199591836160266 ) ) ;
#37101 = CARTESIAN_POINT ( 'NONE',  ( -12.57417428062716169, -296.5872186386752105, -340.3969617874859637 ) ) ;
#37102 = CARTESIAN_POINT ( 'NONE',  ( 34.77128114826058436, -289.0539340169237335, -284.6023332639597925 ) ) ;
#37103 = VERTEX_POINT ( 'NONE', #4292 ) ;
#37104 = CARTESIAN_POINT ( 'NONE',  ( -33.43478769535590800, -295.9453769504820571, -347.0394190793486473 ) ) ;
#37105 = CARTESIAN_POINT ( 'NONE',  ( -37.28711696444914736, -286.5451654788275846, -197.2871505300908552 ) ) ;
#37106 = CARTESIAN_POINT ( 'NONE',  ( -96.68808551110006988, -272.1274988696171704, -221.7659545690757739 ) ) ;
#37107 = CARTESIAN_POINT ( 'NONE',  ( 39.06441415852493293, -294.2468602763872809, -261.7338714033780889 ) ) ;
#37108 = CARTESIAN_POINT ( 'NONE',  ( 21.25949860412116621, -293.3715980453160341, -220.4869418272108135 ) ) ;
#37109 = CARTESIAN_POINT ( 'NONE',  ( -95.11569292176378099, -291.3470766790228481, -225.7386375359353394 ) ) ;
#37110 = ORIENTED_EDGE ( 'NONE', *, *, #49629, .T. ) ;
#37111 = CARTESIAN_POINT ( 'NONE',  ( -30.00352153186533499, -276.0644967538614196, -195.1582900283677304 ) ) ;
#37112 = CARTESIAN_POINT ( 'NONE',  ( 21.55545504677984425, -273.6848999524676174, -221.3801642117571475 ) ) ;
#37113 = EDGE_CURVE ( 'NONE', #33595, #93585, #74616, .T. ) ;
#37114 = ORIENTED_EDGE ( 'NONE', *, *, #27099, .T. ) ;
#37115 = CARTESIAN_POINT ( 'NONE',  ( -111.7695086378747789, -277.8150088739178045, -289.9072141217940839 ) ) ;
#37116 = CARTESIAN_POINT ( 'NONE',  ( 34.90869018961016934, -273.7549116749230507, -255.2553582066626063 ) ) ;
#37117 = CARTESIAN_POINT ( 'NONE',  ( -9.547515864598405955, -274.8246755435575892, -339.2105763082400927 ) ) ;
#37118 = CARTESIAN_POINT ( 'NONE',  ( -76.74189542565464706, -274.5906516487507361, -208.5399995537629820 ) ) ;
#37119 = CARTESIAN_POINT ( 'NONE',  ( -81.22153907556885599, -274.3806759470620023, -211.6632869166898274 ) ) ;
#37120 = CARTESIAN_POINT ( 'NONE',  ( -35.51649072041123389, -299.6747635556786236, -194.1606252097353718 ) ) ;
#37121 = CARTESIAN_POINT ( 'NONE',  ( 36.60956285555379708, -273.3872414189284541, -255.8829444495767689 ) ) ;
#37122 = CARTESIAN_POINT ( 'NONE',  ( -63.59786828688794458, -296.0549178954017862, -338.6386902729140616 ) ) ;
#37123 = PRODUCT_DEFINITION_FORMATION_WITH_SPECIFIED_SOURCE ( 'ANY', '', #26218, .NOT_KNOWN. ) ;
#37124 = CARTESIAN_POINT ( 'NONE',  ( 34.64017021627132209, -292.3278390651728387, -285.7180687391007723 ) ) ;
#37125 = CARTESIAN_POINT ( 'NONE',  ( 157.5411741086738004, 250.0000000000000568, 16.22085278731065472 ) ) ;
#37126 = CARTESIAN_POINT ( 'NONE',  ( -17.36782872132000932, -277.2934187614466737, -344.6616655181607030 ) ) ;
#37127 = CARTESIAN_POINT ( 'NONE',  ( -31.34182623798868050, -274.2966847972199389, -197.5954511542159082 ) ) ;
#37128 = VECTOR ( 'NONE', #93669, 1000.000000000000114 ) ;
#37129 = CARTESIAN_POINT ( 'NONE',  ( -75.84396329312608032, -284.2345484348117566, -204.1875322436704607 ) ) ;
#37130 = CARTESIAN_POINT ( 'NONE',  ( -111.3389064082464444, -298.7215197947444381, -257.1534728006878936 ) ) ;
#37131 = DIRECTION ( 'NONE',  ( -0.000000000000000000, -1.000000000000000000, -0.000000000000000000 ) ) ;
#37132 = CARTESIAN_POINT ( 'NONE',  ( -101.1271035063300019, -284.2397861864604351, -234.4240390724175711 ) ) ;
#37133 = CARTESIAN_POINT ( 'NONE',  ( -106.2188952785525089, -276.4346918008217244, -297.4518174912482209 ) ) ;
#37134 = CARTESIAN_POINT ( 'NONE',  ( -110.0771958099321779, -276.9806140440716717, -281.5379952495150064 ) ) ;
#37135 = CARTESIAN_POINT ( 'NONE',  ( -31.02541847299138666, -284.9726307840362551, -345.1454264232606306 ) ) ;
#37136 = CARTESIAN_POINT ( 'NONE',  ( 32.90083767457183939, -277.0380784229789128, -291.6912475501101198 ) ) ;
#37137 = CYLINDRICAL_SURFACE ( 'NONE', #23090, 11.68950434577434372 ) ;
#37138 = CARTESIAN_POINT ( 'NONE',  ( 37.11953329148045100, -274.1573449175235169, -286.6073447017477065 ) ) ;
#37139 = CARTESIAN_POINT ( 'NONE',  ( -95.41760529303932969, -281.2091043533106927, -222.6208934255556358 ) ) ;
#37140 = DIRECTION ( 'NONE',  ( -0.000000000000000000, -0.000000000000000000, -1.000000000000000000 ) ) ;
#37141 = CARTESIAN_POINT ( 'NONE',  ( -10.52827084031595639, -288.3192551652211364, -199.6629480257257114 ) ) ;
#37142 = CARTESIAN_POINT ( 'NONE',  ( 158.3977298502249766, 17.52828139914420191, -10.67961748035033587 ) ) ;
#37143 = CARTESIAN_POINT ( 'NONE',  ( 32.23614578605712921, -291.9184178325068046, -298.4963633471092521 ) ) ;
#37144 = CARTESIAN_POINT ( 'NONE',  ( 82.17437182012335484, -297.5505941057896280, -195.5323370396037035 ) ) ;
#37145 = CARTESIAN_POINT ( 'NONE',  ( -55.37646185865559545, -296.6099646319331100, -199.1616506149183010 ) ) ;
#37146 = CARTESIAN_POINT ( 'NONE',  ( -109.5574381313751644, -288.4686289342589589, -287.5585790842105780 ) ) ;
#37147 = CARTESIAN_POINT ( 'NONE',  ( 189.0118003482855613, 275.4351431090623237, -122.7278359107281887 ) ) ;
#37148 = CARTESIAN_POINT ( 'NONE',  ( -37.81013033203306861, -296.0461271000310148, -195.3625764867553016 ) ) ;
#37149 = CARTESIAN_POINT ( 'NONE',  ( -41.74011743944212327, -287.5864703687000201, -346.5540194227464212 ) ) ;
#37150 = CARTESIAN_POINT ( 'NONE',  ( -8.159353768194760548, -284.2635759339248125, -338.1463013005608218 ) ) ;
#37151 = CARTESIAN_POINT ( 'NONE',  ( -95.03233181523984285, -283.4689498841880777, -220.8275482326354506 ) ) ;
#37152 = CARTESIAN_POINT ( 'NONE',  ( -45.68841944365056662, -284.5851508454682630, -343.5268660307907567 ) ) ;
#37153 = CARTESIAN_POINT ( 'NONE',  ( -58.98617070704653997, -284.1421791984462857, -340.3008443430176158 ) ) ;
#37154 = CARTESIAN_POINT ( 'NONE',  ( -71.14553320370634992, -291.4760290429610450, -337.7087807191740012 ) ) ;
#37155 = CARTESIAN_POINT ( 'NONE',  ( -88.02564103446042054, -273.6993168240351793, -212.3516357369291825 ) ) ;
#37156 = CARTESIAN_POINT ( 'NONE',  ( 17.58100758195860536, -286.3542267474915661, -322.2534139018941346 ) ) ;
#37157 = CARTESIAN_POINT ( 'NONE',  ( 13.96447640051007610, -274.7484070352196568, -212.8731763715531144 ) ) ;
#37158 = CARTESIAN_POINT ( 'NONE',  ( 35.24135088202188371, -295.3066135317819203, -252.8839762770671484 ) ) ;
#37159 = CARTESIAN_POINT ( 'NONE',  ( -48.18343439339133027, -256.0722001994441825, -452.3316844814242472 ) ) ;
#37160 = CARTESIAN_POINT ( 'NONE',  ( 10.64812456238590066, -290.9090924074130839, -330.4860931364851808 ) ) ;
#37161 = CARTESIAN_POINT ( 'NONE',  ( -59.11007243505797959, -282.0245136325808630, -340.6099320266833388 ) ) ;
#37162 = CARTESIAN_POINT ( 'NONE',  ( -83.75484944032145052, -275.6869242708368120, -329.5529688687923908 ) ) ;
#37163 = CARTESIAN_POINT ( 'NONE',  ( -98.99531427405814554, -271.6352340948325832, -225.3119947928427109 ) ) ;
#37164 = CARTESIAN_POINT ( 'NONE',  ( 26.85230179668491601, -275.3787197170688614, -305.4386597724418380 ) ) ;
#37165 = CARTESIAN_POINT ( 'NONE',  ( 21.53618899909647055, -294.4557530579195941, -226.0429284211115259 ) ) ;
#37166 = CARTESIAN_POINT ( 'NONE',  ( 0.01880844349002916416, -293.5039402878927035, -207.3722233468175773 ) ) ;
#37168 = EDGE_CURVE ( 'NONE', #47196, #64642, #50429, .T. ) ;
#37167 = CARTESIAN_POINT ( 'NONE',  ( -107.1217038909655912, -285.9866456125935770, -295.1859555809152766 ) ) ;
#37169 = CARTESIAN_POINT ( 'NONE',  ( 36.53159358878502871, -295.2237751869107569, -289.8891176156973870 ) ) ;
#37170 = CARTESIAN_POINT ( 'NONE',  ( 24.40646849695092513, -294.2637080330470098, -225.1896452906121624 ) ) ;
#37171 = CARTESIAN_POINT ( 'NONE',  ( -69.72597773767806473, -295.3242280397142281, -335.7848030533413635 ) ) ;
#37172 = CARTESIAN_POINT ( 'NONE',  ( -72.07701453124620627, -291.5116069881614749, -336.8471122894359837 ) ) ;
#37173 = CARTESIAN_POINT ( 'NONE',  ( -52.91553849778298257, -283.4129980048540460, -345.8242004598414496 ) ) ;
#37174 = CARTESIAN_POINT ( 'NONE',  ( -20.87629721956141893, -296.3365913390894661, -194.8064469063934894 ) ) ;
#37175 = CARTESIAN_POINT ( 'NONE',  ( -65.87538817740572483, -285.5223501403916657, -198.8289333778589025 ) ) ;
#37176 = CARTESIAN_POINT ( 'NONE',  ( -79.54156228122062089, -279.6047886331531345, -331.9952902659023266 ) ) ;
#37177 = EDGE_CURVE ( 'NONE', #60489, #78013, #83826, .T. ) ;
#37178 = CARTESIAN_POINT ( 'NONE',  ( -57.48872647716817852, -284.5812856528338557, -199.7304081365564628 ) ) ;
#37179 = CARTESIAN_POINT ( 'NONE',  ( 25.74824362719364146, -286.0993400141191501, -311.0112308093402476 ) ) ;
#37180 = CARTESIAN_POINT ( 'NONE',  ( -56.22551449035876203, -277.9511249168207883, -196.9332559652179668 ) ) ;
#37181 = DIRECTION ( 'NONE',  ( -1.000000000000000000, -0.000000000000000000, -0.000000000000000000 ) ) ;
#37182 = CARTESIAN_POINT ( 'NONE',  ( -108.4866588822361280, -283.8400249096803236, -287.0405797903704297 ) ) ;
#37183 = CARTESIAN_POINT ( 'NONE',  ( 37.48101548385013615, -282.9643855393206309, -286.8403346246170145 ) ) ;
#37184 = CARTESIAN_POINT ( 'NONE',  ( -29.01465186027991905, -288.0079456625308580, -346.7262120174191296 ) ) ;
#37185 = CARTESIAN_POINT ( 'NONE',  ( -82.06016339930624781, -279.2508283923674526, -332.0595738483911532 ) ) ;
#37186 = CARTESIAN_POINT ( 'NONE',  ( -35.70515885984242743, -278.3472253223114876, -346.8635030127408072 ) ) ;
#37187 = CARTESIAN_POINT ( 'NONE',  ( -72.12783937481628982, -279.4117044711398421, -206.1822700587617021 ) ) ;
#37188 = CARTESIAN_POINT ( 'NONE',  ( -46.40289275953759329, -275.9164964099653048, -196.2683275814586068 ) ) ;
#37189 = CARTESIAN_POINT ( 'NONE',  ( 11.11878729026226686, -292.7017228325184419, -210.4545615941174219 ) ) ;
#37190 = CARTESIAN_POINT ( 'NONE',  ( 19.05196499571339785, -286.2545813980258913, -319.3424753718862803 ) ) ;
#37191 = CIRCLE ( 'NONE', #49288, 24.00000000000000355 ) ;
#37192 = CARTESIAN_POINT ( 'NONE',  ( -107.6370626030929571, -292.5302789497656022, -240.9501943634475651 ) ) ;
#37193 = CARTESIAN_POINT ( 'NONE',  ( 21.56669368202042847, -293.0817289457330617, -313.9962782670322099 ) ) ;
#37194 = CARTESIAN_POINT ( 'NONE',  ( -28.89774648281880687, -294.6090157395627784, -342.9434300135208673 ) ) ;
#37195 = CARTESIAN_POINT ( 'NONE',  ( -113.0526920475670352, -291.4783708322835309, -282.5815194711419167 ) ) ;
#37196 = CARTESIAN_POINT ( 'NONE',  ( 33.05984951545999451, -282.4633875713348630, -290.0465053594404594 ) ) ;
#37197 = CARTESIAN_POINT ( 'NONE',  ( -46.08094623810074353, -296.8641019593885062, -194.1697924476801518 ) ) ;
#37198 = CARTESIAN_POINT ( 'NONE',  ( 37.04791602180043952, -288.4477338975623866, -289.8418211521286594 ) ) ;
#37199 = CARTESIAN_POINT ( 'NONE',  ( 12.84458278802912190, -280.5005193778989110, -327.1904458860697673 ) ) ;
#37200 = CARTESIAN_POINT ( 'NONE',  ( 35.05403498052020694, -288.2177055046319651, -296.6811252165226165 ) ) ;
#37201 = CARTESIAN_POINT ( 'NONE',  ( -49.42920682756628281, -286.2272189558863715, -198.2958577122393820 ) ) ;
#37202 = CARTESIAN_POINT ( 'NONE',  ( 179.6752721478330557, 254.2973581424797374, -166.6431896918319637 ) ) ;
#37203 = CARTESIAN_POINT ( 'NONE',  ( -64.79168948216373281, -181.8610138526347839, -360.2174547310475532 ) ) ;
#37204 = CARTESIAN_POINT ( 'NONE',  ( -76.76410942417290073, -208.0616896646858152, -353.4147769976461291 ) ) ;
#37205 = CARTESIAN_POINT ( 'NONE',  ( -110.0657075408640821, -277.6382604475187463, -278.7983081019125393 ) ) ;
#37206 = CARTESIAN_POINT ( 'NONE',  ( -92.97013546518614646, -276.7955974803167578, -318.1073561200034874 ) ) ;
#37207 = CARTESIAN_POINT ( 'NONE',  ( 30.72698958417520387, -298.3906325157475976, -193.4281377556751522 ) ) ;
#37208 = CARTESIAN_POINT ( 'NONE',  ( 200.4462836145382312, 285.9195334705995606, -96.58237528659300608 ) ) ;
#37209 = CARTESIAN_POINT ( 'NONE',  ( -22.66146481047934813, -278.8110956830652185, -195.3199634834428196 ) ) ;
#37210 = CARTESIAN_POINT ( 'NONE',  ( 22.38921990735957479, -295.9489660591522693, -317.3521110250798642 ) ) ;
#37211 = CARTESIAN_POINT ( 'NONE',  ( -4.811308010211996056, -292.9848514098938494, -204.9272918964365147 ) ) ;
#37212 = CARTESIAN_POINT ( 'NONE',  ( -97.63572512416159555, -274.1307999741873118, -222.8484800435509499 ) ) ;
#37213 = CARTESIAN_POINT ( 'NONE',  ( 6.122885099020168198, -287.1335185242441526, -329.6872779768310693 ) ) ;
#37214 = CARTESIAN_POINT ( 'NONE',  ( 30.71440275779965035, -299.3751842690778062, -193.4171149168752493 ) ) ;
#37215 = CARTESIAN_POINT ( 'NONE',  ( -81.94579477330741213, -297.5917719608419816, -212.5088625246573315 ) ) ;
#37216 = ORIENTED_EDGE ( 'NONE', *, *, #20271, .F. ) ;
#37217 = DIRECTION ( 'NONE',  ( 0.9452808130703184153, -0.000000000000000000, -0.3262578496237564796 ) ) ;
#37218 = CARTESIAN_POINT ( 'NONE',  ( -53.47727111639837005, -281.7670297583512706, -196.4905116048815614 ) ) ;
#37219 = CARTESIAN_POINT ( 'NONE',  ( -110.6607936354956792, -279.6640070631573280, -267.9115927433266506 ) ) ;
#37220 = CARTESIAN_POINT ( 'NONE',  ( -109.5932499090205710, -280.6141581524346407, -246.6633948029254668 ) ) ;
#37221 = CARTESIAN_POINT ( 'NONE',  ( 0.9894731810292046736, -273.0536950562868128, -207.4212347213027101 ) ) ;
#37222 = ADVANCED_FACE ( 'NONE', ( #11861 ), #5254, .T. ) ;
#37223 = DIRECTION ( 'NONE',  ( 0.000000000000000000, 0.000000000000000000, 1.000000000000000000 ) ) ;
#37224 = EDGE_CURVE ( 'NONE', #69256, #92724, #76610, .T. ) ;
#37225 = DIRECTION ( 'NONE',  ( 0.000000000000000000, 1.000000000000000000, 0.000000000000000000 ) ) ;
#37226 = CARTESIAN_POINT ( 'NONE',  ( -64.81808472547032807, -279.8497032214888236, -202.7294072695395926 ) ) ;
#37227 = CARTESIAN_POINT ( 'NONE',  ( 32.87635832453768359, -276.7540506009354999, -301.5634109616956948 ) ) ;
#37228 = CARTESIAN_POINT ( 'NONE',  ( 35.95664103302951276, -277.7570510616286583, -286.3068623283666057 ) ) ;
#37229 = CARTESIAN_POINT ( 'NONE',  ( -62.23134649491931469, -275.9442275230288715, -342.6604208264586191 ) ) ;
#37230 = ORIENTED_EDGE ( 'NONE', *, *, #18442, .T. ) ;
#37231 = DIRECTION ( 'NONE',  ( 0.000000000000000000, -0.000000000000000000, 1.000000000000000000 ) ) ;
#37232 = CARTESIAN_POINT ( 'NONE',  ( -13.90895442258618431, -284.7294743734213398, -341.9803418662686454 ) ) ;
#37233 = CARTESIAN_POINT ( 'NONE',  ( -81.81912626926953180, -290.6259927298177104, -212.2077736812288435 ) ) ;
#37234 = CARTESIAN_POINT ( 'NONE',  ( 38.45779427508252724, -286.7375759682649914, -257.3317933329411176 ) ) ;
#37235 = CARTESIAN_POINT ( 'NONE',  ( -65.72474233370687102, -281.6683844946635418, -338.7296945338605383 ) ) ;
#37237 = CARTESIAN_POINT ( 'NONE',  ( 35.11753903505927354, -285.4106169121541825, -253.2480271490028940 ) ) ;
#37236 = CARTESIAN_POINT ( 'NONE',  ( 8.144035905089078042, -280.9911625579424026, -328.2744583910110237 ) ) ;
#37238 = CARTESIAN_POINT ( 'NONE',  ( 31.43704377151221863, -282.4155690147152313, -244.5908916414939824 ) ) ;
#37239 = CARTESIAN_POINT ( 'NONE',  ( -112.3417001280813565, -270.5523135751784594, -270.3357089863371812 ) ) ;
#37240 = CARTESIAN_POINT ( 'NONE',  ( -70.14439826573801895, -281.8769492942743113, -339.1535044043376388 ) ) ;
#37241 = CARTESIAN_POINT ( 'NONE',  ( -22.46859069622999527, -296.8618801463102272, -343.8716020072762944 ) ) ;
#37242 = CARTESIAN_POINT ( 'NONE',  ( -74.63590070761051720, -280.4843582892498262, -207.2746477157267577 ) ) ;
#37243 = CARTESIAN_POINT ( 'NONE',  ( -94.44099627240861139, -287.2286414266218912, -221.3984778033835710 ) ) ;
#37244 = CARTESIAN_POINT ( 'NONE',  ( 210.2447652224009573, 1.019566348684628698, -7.291626467228960351 ) ) ;
#37245 = CARTESIAN_POINT ( 'NONE',  ( -78.82466731291643214, -293.4184390265403977, -207.1441659699051741 ) ) ;
#37246 = CARTESIAN_POINT ( 'NONE',  ( 8.791087937605919223, -274.4199449409945260, -329.5607401776369443 ) ) ;
#37247 = CARTESIAN_POINT ( 'NONE',  ( 10.12015998139964523, -287.6141237037815017, -330.8566964078613069 ) ) ;
#37248 = CARTESIAN_POINT ( 'NONE',  ( 35.70242817470591490, -291.8145452261563833, -259.8256666000236805 ) ) ;
#37249 = CARTESIAN_POINT ( 'NONE',  ( -98.06567382502505836, -276.6649003716942730, -311.7596988370123086 ) ) ;
#37250 = CARTESIAN_POINT ( 'NONE',  ( -109.6753463270026003, -294.9083027293222585, -253.6665346802094518 ) ) ;
#37251 = CARTESIAN_POINT ( 'NONE',  ( -110.8615624681319645, -291.8921702570154366, -268.4656389857661907 ) ) ;
#37252 = CARTESIAN_POINT ( 'NONE',  ( -147.0026986695708047, -210.7421749798627673, -21.50000000000000000 ) ) ;
#37253 = CARTESIAN_POINT ( 'NONE',  ( -41.92345788835077514, -293.5886472342795059, -346.5820305606991951 ) ) ;
#37254 = CARTESIAN_POINT ( 'NONE',  ( 33.79502637761630268, -288.8954811245253609, -250.7140683692962284 ) ) ;
#37255 = CARTESIAN_POINT ( 'NONE',  ( -112.6586249066970140, -288.9244592299990586, -259.9102210491147957 ) ) ;
#37256 = CARTESIAN_POINT ( 'NONE',  ( 34.27870761690637380, -289.1987015317446890, -287.2694624750785124 ) ) ;
#37257 = DIRECTION ( 'NONE',  ( 0.000000000000000000, 0.000000000000000000, 1.000000000000000000 ) ) ;
#37258 = CARTESIAN_POINT ( 'NONE',  ( -82.63825224533155733, -290.4924902514837868, -327.8139168065159765 ) ) ;
#37259 = CARTESIAN_POINT ( 'NONE',  ( 219.8344101925596021, 0.000000000000000000, -7.000000000000000888 ) ) ;
#37260 = CARTESIAN_POINT ( 'NONE',  ( -80.30515343051358457, -290.8247594925233557, -333.8456154741436990 ) ) ;
#37261 = CARTESIAN_POINT ( 'NONE',  ( -4.354366754540068385, -278.5048357423264633, -202.5955776277986615 ) ) ;
#37262 = CARTESIAN_POINT ( 'NONE',  ( -104.7771072349043067, -279.3664035069019178, -233.2368649963776477 ) ) ;
#37263 = CARTESIAN_POINT ( 'NONE',  ( 8.537341559538260682, -280.3278088705010873, -208.4817666927683604 ) ) ;
#37264 = CARTESIAN_POINT ( 'NONE',  ( 35.33271381935216482, -285.3133092422007167, -251.7773406110986798 ) ) ;
#37265 = CARTESIAN_POINT ( 'NONE',  ( 208.1147618731698401, 29.48222340873819292, 14.79012820594046218 ) ) ;
#37266 = CARTESIAN_POINT ( 'NONE',  ( 12.14659068537289599, -278.8889627864730301, -215.0278138133120649 ) ) ;
#37267 = CARTESIAN_POINT ( 'NONE',  ( -6.306978966449482193, -280.6442960714742867, -338.6388356855028974 ) ) ;
#37268 = CARTESIAN_POINT ( 'NONE',  ( -88.01846039707731961, -229.9137307660017484, -344.5856827696274536 ) ) ;
#37269 = CARTESIAN_POINT ( 'NONE',  ( -111.8120368226499295, -276.8220449022496155, -287.0007306086178573 ) ) ;
#37270 = CARTESIAN_POINT ( 'NONE',  ( -111.4190244139907122, -283.7243002278159452, -250.3111566686916376 ) ) ;
#37271 = CARTESIAN_POINT ( 'NONE',  ( -35.82142624576487577, -299.0128965477977090, -197.1255714116523734 ) ) ;
#37272 = CARTESIAN_POINT ( 'NONE',  ( -80.92927823114250430, -274.8987345943192508, -207.5376944864815982 ) ) ;
#37273 = CARTESIAN_POINT ( 'NONE',  ( 35.39967989315321262, -275.1273696347490727, -263.4229568557001926 ) ) ;
#37274 = CARTESIAN_POINT ( 'NONE',  ( -28.63930020621857153, -296.9420813785833388, -344.9069457492344100 ) ) ;
#37275 = CARTESIAN_POINT ( 'NONE',  ( 16.68746894093080968, -288.4760545915963235, -325.2973537541544715 ) ) ;
#37276 = CARTESIAN_POINT ( 'NONE',  ( 26.64518807274798462, -279.0946793915359763, -230.0760469442941201 ) ) ;
#37277 = CARTESIAN_POINT ( 'NONE',  ( -67.01348336552244689, -291.5071411942748227, -199.3077205688790627 ) ) ;
#37278 = CARTESIAN_POINT ( 'NONE',  ( -103.0618413403168177, -289.1744323941791777, -302.6763076990845320 ) ) ;
#37279 = CARTESIAN_POINT ( 'NONE',  ( 36.62938245601388587, -291.7119545675024597, -282.8193912004442154 ) ) ;
#37280 = VERTEX_POINT ( 'NONE', #27971 ) ;
#37281 = CARTESIAN_POINT ( 'NONE',  ( 198.9495682819174647, 68.47409081099804951, 9.196090786366733383 ) ) ;
#37282 = CARTESIAN_POINT ( 'NONE',  ( -108.7241931824519554, -289.8538284535074467, -285.9926154946443830 ) ) ;
#37283 = DIRECTION ( 'NONE',  ( 0.000000000000000000, 0.000000000000000000, -1.000000000000000000 ) ) ;
#37284 = CARTESIAN_POINT ( 'NONE',  ( -36.57984325276299842, -287.0027419501200256, -193.5871929265269102 ) ) ;
#37285 = CARTESIAN_POINT ( 'NONE',  ( -53.28691492658256834, -297.7662352645559167, -340.3683826091709079 ) ) ;
#37286 = CARTESIAN_POINT ( 'NONE',  ( -27.78903667325146287, -293.9925540688091701, -346.5822642311194954 ) ) ;
#37287 = CARTESIAN_POINT ( 'NONE',  ( -0.5974777997168068122, -283.8896200043104727, -337.4815542766774570 ) ) ;
#37288 = CARTESIAN_POINT ( 'NONE',  ( -105.2147187587827091, -284.0243312394444501, -297.3735001381943448 ) ) ;
#37289 = CARTESIAN_POINT ( 'NONE',  ( 20.23144391921339036, -276.2266426169885563, -224.6619271695542466 ) ) ;
#37290 = CARTESIAN_POINT ( 'NONE',  ( 35.67126341593337457, -291.7733089069558901, -285.9450239843537815 ) ) ;
#37291 = EDGE_CURVE ( 'NONE', #54318, #60845, #29283, .T. ) ;
#37292 = CARTESIAN_POINT ( 'NONE',  ( -69.65200492506903629, -272.4118915382899786, -204.4583508926859565 ) ) ;
#37293 = ORIENTED_EDGE ( 'NONE', *, *, #61083, .T. ) ;
#37294 = CARTESIAN_POINT ( 'NONE',  ( -108.4555765497910471, -262.4588243622614527, -317.8183916042563055 ) ) ;
#37295 = CARTESIAN_POINT ( 'NONE',  ( 38.33568392662063218, -293.3960930538071352, -284.5276334989173961 ) ) ;
#37296 = CARTESIAN_POINT ( 'NONE',  ( 30.10454924828650292, -289.0551557443410502, -238.8600443507633031 ) ) ;
#37297 = CARTESIAN_POINT ( 'NONE',  ( -88.38938719997088356, -296.8271921599790062, -327.6654055070242180 ) ) ;
#37298 = CARTESIAN_POINT ( 'NONE',  ( -2.144580861112217463, -287.1822253493394896, -206.2336185821078800 ) ) ;
#37299 = CARTESIAN_POINT ( 'NONE',  ( -111.9493516628153600, -277.3835340378610113, -288.4860338994133713 ) ) ;
#37300 = CARTESIAN_POINT ( 'NONE',  ( 19.45999875845602745, -294.9099003179920828, -322.2738091659118140 ) ) ;
#37301 = CARTESIAN_POINT ( 'NONE',  ( 19.62821790832263247, -286.3787296932925415, -320.3279667410840830 ) ) ;
#37302 = CARTESIAN_POINT ( 'NONE',  ( -33.43166539612342802, -295.3375043451268311, -347.2537233179010059 ) ) ;
#37303 = CARTESIAN_POINT ( 'NONE',  ( -60.26963068164201331, -292.0799649252532504, -200.9798745687502048 ) ) ;
#37304 = DIRECTION ( 'NONE',  ( 0.4999999999999967248, 0.8660254037844404840, 0.000000000000000000 ) ) ;
#37305 = CARTESIAN_POINT ( 'NONE',  ( 0.000000000000000000, 0.000000000000000000, 13.99999999999999112 ) ) ;
#37306 = CARTESIAN_POINT ( 'NONE',  ( 153.8785610233898353, 204.4371874965355005, -214.4256267419547157 ) ) ;
#37307 = CARTESIAN_POINT ( 'NONE',  ( -15.62943896399615262, -287.8481154429661615, -197.1537483369301640 ) ) ;
#37308 = CARTESIAN_POINT ( 'NONE',  ( 25.22466315766302358, -290.4094976428775112, -220.5068182859052968 ) ) ;
#37309 = EDGE_LOOP ( 'NONE', ( #53841, #31143, #16046, #17128 ) ) ;
#37310 = CARTESIAN_POINT ( 'NONE',  ( -45.25462026394541937, -279.3031421062002551, -193.8183392458116145 ) ) ;
#37311 = CARTESIAN_POINT ( 'NONE',  ( 18.41213393662922826, -282.8556198275064162, -220.4458055518025503 ) ) ;
#37312 = CARTESIAN_POINT ( 'NONE',  ( 204.7385621006099541, 293.0224724744894615, -54.00000000000019185 ) ) ;
#37313 = CARTESIAN_POINT ( 'NONE',  ( -89.47089566606882727, -283.9099361480904804, -214.4218883608680244 ) ) ;
#37314 = CARTESIAN_POINT ( 'NONE',  ( -42.79331104629897453, -287.2011782544228140, -344.6528317607025542 ) ) ;
#37315 = CARTESIAN_POINT ( 'NONE',  ( -0.6644879575998082766, -276.3944040201157009, -204.0509106616867712 ) ) ;
#37316 = CARTESIAN_POINT ( 'NONE',  ( -109.1073012028064113, -297.2259518018898916, -256.5945685722813323 ) ) ;
#37317 = CARTESIAN_POINT ( 'NONE',  ( 14.65341603429722284, -292.9863700605037593, -322.3725373520155131 ) ) ;
#37318 = CARTESIAN_POINT ( 'NONE',  ( -113.6170953225393561, -279.3309410343756554, -260.1895831718448449 ) ) ;
#37319 = CARTESIAN_POINT ( 'NONE',  ( 32.51638969446961624, -275.8331972023412391, -291.5904667548300608 ) ) ;
#37320 = CARTESIAN_POINT ( 'NONE',  ( -68.73017754652568101, -274.7288321063439867, -200.3735272335182174 ) ) ;
#37321 = CARTESIAN_POINT ( 'NONE',  ( -23.01020350233489609, -275.7934125632637006, -345.7549851419325364 ) ) ;
#37322 = DIRECTION ( 'NONE',  ( -0.000000000000000000, -1.000000000000000000, -0.000000000000000000 ) ) ;
#37323 = CARTESIAN_POINT ( 'NONE',  ( 37.70720199943995965, -273.5442517067217523, -269.7586664074857481 ) ) ;
#37324 = CARTESIAN_POINT ( 'NONE',  ( -112.3141080162607324, -298.1642372451777874, -255.5375871175444331 ) ) ;
#37325 = CARTESIAN_POINT ( 'NONE',  ( -112.3417001280813849, -275.0519495502701943, -270.3929463913696054 ) ) ;
#37326 = CARTESIAN_POINT ( 'NONE',  ( 196.7806748523260012, 214.5000000000000568, -12.67104836398113576 ) ) ;
#37327 = CARTESIAN_POINT ( 'NONE',  ( -54.84340659790353101, -286.9016483771832782, -199.1192969965702559 ) ) ;
#37328 = CARTESIAN_POINT ( 'NONE',  ( -85.44336532270544637, -285.4669562479273281, -329.1846151312274742 ) ) ;
#37329 = CARTESIAN_POINT ( 'NONE',  ( -65.12428514459263340, -285.0280038265851772, -202.6905196007719212 ) ) ;
#37330 = CARTESIAN_POINT ( 'NONE',  ( -93.34689749296420302, -276.2752246297795296, -318.4221030415608311 ) ) ;
#37331 = CARTESIAN_POINT ( 'NONE',  ( -69.52356149078943304, -285.3407113747234121, -337.2720372971938900 ) ) ;
#37332 = CARTESIAN_POINT ( 'NONE',  ( -110.8488725689581429, -277.1004294037684872, -265.1262969920673527 ) ) ;
#37333 = EDGE_CURVE ( 'NONE', #78639, #9799, #560, .T. ) ;
#37334 = CARTESIAN_POINT ( 'NONE',  ( -29.66745107731571096, -278.0325191603734538, -343.3185633340101504 ) ) ;
#37335 = EDGE_CURVE ( 'NONE', #57853, #60383, #89729, .T. ) ;
#37336 = CARTESIAN_POINT ( 'NONE',  ( 197.8059408385280165, 70.97274906999653865, -10.93303304242674656 ) ) ;
#37337 = CARTESIAN_POINT ( 'NONE',  ( -110.4034719488357297, -273.0803523630808627, -267.6412165631991797 ) ) ;
#37338 = CARTESIAN_POINT ( 'NONE',  ( 19.03472298386827433, -281.6422731844011764, -218.1513704480079241 ) ) ;
#37339 = CARTESIAN_POINT ( 'NONE',  ( -5.475280587860151371, -283.1364005535865545, -340.3900991914817951 ) ) ;
#37340 = ORIENTED_EDGE ( 'NONE', *, *, #77632, .T. ) ;
#37341 = VERTEX_POINT ( 'NONE', #20848 ) ;
#37342 = CARTESIAN_POINT ( 'NONE',  ( 200.2454457599218927, 15.96501597607006850, -10.07064028581557835 ) ) ;
#37343 = CARTESIAN_POINT ( 'NONE',  ( 22.00925704606999034, -288.7718418219653245, -223.2472496350641791 ) ) ;
#37344 = CARTESIAN_POINT ( 'NONE',  ( -111.4485672590603826, -288.9969268384077736, -289.4259508522750366 ) ) ;
#37345 = CARTESIAN_POINT ( 'NONE',  ( -75.28566730507230886, -296.7298162703662001, -207.7495515911309383 ) ) ;
#37346 = CARTESIAN_POINT ( 'NONE',  ( -69.57285839711249764, -290.9875572401598447, -200.5294255433047113 ) ) ;
#37347 = CARTESIAN_POINT ( 'NONE',  ( 34.06515417399135970, -285.7932701412069605, -252.0956060185467038 ) ) ;
#37348 = CARTESIAN_POINT ( 'NONE',  ( -76.19512105307381944, -288.1573354591596399, -332.8574106658682012 ) ) ;
#37349 = CARTESIAN_POINT ( 'NONE',  ( -35.94119580413624249, -287.2751839588753455, -196.9774066180032719 ) ) ;
#37350 = CARTESIAN_POINT ( 'NONE',  ( -109.8992335756570498, -276.3074393677642320, -289.3959833164004749 ) ) ;
#37351 = CARTESIAN_POINT ( 'NONE',  ( -8.965592794820878453, -290.6812121732749574, -339.7997750843401832 ) ) ;
#37352 = CARTESIAN_POINT ( 'NONE',  ( -73.56668085324497497, -287.5314850686552290, -336.2376344362913301 ) ) ;
#37353 = CARTESIAN_POINT ( 'NONE',  ( -98.30956833429530661, -286.0548376537249737, -229.7861565585783978 ) ) ;
#37354 = CARTESIAN_POINT ( 'NONE',  ( -100.1660193917986987, -293.1090998540954047, -228.9986340924901072 ) ) ;
#37355 = LINE ( 'NONE', #66262, #53398 ) ;
#37356 = DIRECTION ( 'NONE',  ( -1.000000000000000000, 0.000000000000000000, 0.000000000000000000 ) ) ;
#37357 = CARTESIAN_POINT ( 'NONE',  ( -96.53699812076511932, -275.1692720078602292, -223.7314760895574466 ) ) ;
#37358 = CARTESIAN_POINT ( 'NONE',  ( -43.75507891956904416, -279.1663383484598171, -197.4309382420261159 ) ) ;
#37359 = CARTESIAN_POINT ( 'NONE',  ( 34.87863396652471693, -279.8122422810128000, -290.5904035344075282 ) ) ;
#37360 = CARTESIAN_POINT ( 'NONE',  ( 11.08859352418373412, -293.5985985249304804, -330.0842288860447979 ) ) ;
#37361 = CARTESIAN_POINT ( 'NONE',  ( -64.92591828202790794, -271.9267068637113312, -201.6664154785643746 ) ) ;
#37362 = CARTESIAN_POINT ( 'NONE',  ( 17.57733476761621461, -274.3391491081213189, -320.6316280927646858 ) ) ;
#37363 = CARTESIAN_POINT ( 'NONE',  ( -50.05558065664418876, -299.2016873674821227, -197.9760316823304720 ) ) ;
#37364 = DIRECTION ( 'NONE',  ( 0.000000000000000000, 0.000000000000000000, -1.000000000000000000 ) ) ;
#37365 = CARTESIAN_POINT ( 'NONE',  ( -113.2957492518303155, -294.8376403577980795, -266.7606426456421786 ) ) ;
#37366 = CARTESIAN_POINT ( 'NONE',  ( 36.29771464335428988, -294.9824560454705988, -270.7450278594627093 ) ) ;
#37367 = CARTESIAN_POINT ( 'NONE',  ( -94.89414429562873465, -296.7194265151134687, -315.5309961967191725 ) ) ;
#37368 = CARTESIAN_POINT ( 'NONE',  ( 60.30377782462292657, -249.1633071459562530, -21.50000000000000000 ) ) ;
#37370 = CARTESIAN_POINT ( 'NONE',  ( -97.18337698819165382, -295.9691845535620018, -312.1698935036170610 ) ) ;
#37369 = CARTESIAN_POINT ( 'NONE',  ( -43.50602473436414641, -283.9948892174213597, -195.2063478201638986 ) ) ;
#37371 = CARTESIAN_POINT ( 'NONE',  ( -71.73874023561099023, -283.4941621538452523, -339.2512016800052379 ) ) ;
#37372 = CARTESIAN_POINT ( 'NONE',  ( 14.77826650365005179, -284.2448253073169440, -325.0678202639791721 ) ) ;
#37373 = CARTESIAN_POINT ( 'NONE',  ( -33.72407509847515428, -285.7632304212094141, -193.4673140662763728 ) ) ;
#37374 = CARTESIAN_POINT ( 'NONE',  ( 33.54571662535364140, -291.2393223265788720, -246.2204340254771466 ) ) ;
#37375 = CARTESIAN_POINT ( 'NONE',  ( -114.1306607305792085, -277.8494598791134536, -274.4560313994116427 ) ) ;
#37376 = CARTESIAN_POINT ( 'NONE',  ( 39.58706461736020543, -273.0523547857347353, -270.3937649182068981 ) ) ;
#37377 = CARTESIAN_POINT ( 'NONE',  ( -48.18343439339132317, -256.9144228299669521, -495.6365959160108332 ) ) ;
#37378 = CARTESIAN_POINT ( 'NONE',  ( 13.42522107200286463, -285.5764883299042367, -217.2829634672676207 ) ) ;
#37379 = CARTESIAN_POINT ( 'NONE',  ( -113.8054590362175134, -289.3902066666066162, -276.9134418955106867 ) ) ;
#37380 = DIRECTION ( 'NONE',  ( 1.000000000000000000, 0.000000000000000000, 0.000000000000000000 ) ) ;
#37381 = CARTESIAN_POINT ( 'NONE',  ( -101.9243865285431241, -298.6350917238896159, -234.6467366958367506 ) ) ;
#37382 = CARTESIAN_POINT ( 'NONE',  ( -92.89304552555748273, -279.2547832978563065, -322.9027667087220266 ) ) ;
#37384 = CARTESIAN_POINT ( 'NONE',  ( 26.87162744191877906, -281.6931065999290240, -305.1279994803028899 ) ) ;
#37383 = CARTESIAN_POINT ( 'NONE',  ( -30.76026802195017851, -292.9894435751852484, -345.4283648619525593 ) ) ;
#37385 = CARTESIAN_POINT ( 'NONE',  ( 37.46051242382480950, -293.9479373214531961, -288.6818090625475293 ) ) ;
#37386 = CARTESIAN_POINT ( 'NONE',  ( -7.881574408821461653, -284.5148489674409689, -200.7252337286944339 ) ) ;
#37387 = CARTESIAN_POINT ( 'NONE',  ( -100.2285193883173235, -281.1044126408368697, -229.3984215881124840 ) ) ;
#37388 = CARTESIAN_POINT ( 'NONE',  ( 1.685113069783463979, -293.5753743016081216, -332.3914583416751043 ) ) ;
#37389 = CARTESIAN_POINT ( 'NONE',  ( -35.85140150718095953, -296.0706510178139297, -195.3616173567541807 ) ) ;
#37390 = ORIENTED_EDGE ( 'NONE', *, *, #81666, .T. ) ;
#37391 = CARTESIAN_POINT ( 'NONE',  ( 201.2104617360081704, 60.19600395700752671, -9.999999999999998224 ) ) ;
#37392 = CARTESIAN_POINT ( 'NONE',  ( 35.25562079966431384, -283.7567442868192984, -287.7786304767633396 ) ) ;
#37393 = CARTESIAN_POINT ( 'NONE',  ( -103.9953280096532779, -295.6556189317900589, -300.4060806146274558 ) ) ;
#37394 = LINE ( 'NONE', #59675, #45829 ) ;
#37395 = CARTESIAN_POINT ( 'NONE',  ( -112.3381139276884824, -270.1608578419545097, -261.8788190812425114 ) ) ;
#37396 = CARTESIAN_POINT ( 'NONE',  ( -52.50373260795684871, -273.0600028258471639, -194.9790315404535477 ) ) ;
#37397 = CARTESIAN_POINT ( 'NONE',  ( -101.6441519101626483, -289.9129493538187603, -305.0254202082359143 ) ) ;
#37398 = CARTESIAN_POINT ( 'NONE',  ( -109.5706370151317088, -280.2641284949510805, -255.6795837693958049 ) ) ;
#37399 = CARTESIAN_POINT ( 'NONE',  ( 3.354289148334625548, -276.2089456547820419, -208.7348288689008200 ) ) ;
#37400 = CARTESIAN_POINT ( 'NONE',  ( -35.89374908788306584, -284.6344323884651430, -346.5603429344531037 ) ) ;
#37401 = CARTESIAN_POINT ( 'NONE',  ( -41.05601463738571510, -278.7992868972816041, -197.0580868500661893 ) ) ;
#37402 = CARTESIAN_POINT ( 'NONE',  ( -62.43563910140775874, -279.3786325067005123, -341.0937236069890446 ) ) ;
#37403 = ORIENTED_EDGE ( 'NONE', *, *, #34428, .F. ) ;
#37404 = CARTESIAN_POINT ( 'NONE',  ( -66.22525101921424096, -273.5176931674315028, -198.9694971214037764 ) ) ;
#37405 = CARTESIAN_POINT ( 'NONE',  ( -96.26901032218887622, -293.1002669520462405, -224.8761060050186984 ) ) ;
#37406 = DIRECTION ( 'NONE',  ( -0.3024135303179394940, -0.9531768234072001134, 0.000000000000000000 ) ) ;
#37407 = DIRECTION ( 'NONE',  ( 1.000000000000000000, 0.000000000000000000, 0.000000000000000000 ) ) ;
#37408 = CARTESIAN_POINT ( 'NONE',  ( 38.26770867222952432, -291.7630473726748050, -275.9716602547186426 ) ) ;
#37409 = CARTESIAN_POINT ( 'NONE',  ( -54.21967317918562657, -273.3371222145809725, -199.2757997576158289 ) ) ;
#37410 = LINE ( 'NONE', #30319, #22837 ) ;
#37411 = CARTESIAN_POINT ( 'NONE',  ( -8.788781319167595640, -293.9391410176762633, -199.5978607045482534 ) ) ;
#37413 = CARTESIAN_POINT ( 'NONE',  ( -30.74682907686137057, -293.3387003487656557, -193.9901124214263461 ) ) ;
#37412 = CARTESIAN_POINT ( 'NONE',  ( -85.28047601435908120, -280.1948066931273047, -330.5268031993605859 ) ) ;
#37414 = CARTESIAN_POINT ( 'NONE',  ( 18.23554217258606513, -288.8521129944070935, -220.2301350138416183 ) ) ;
#37415 = CARTESIAN_POINT ( 'NONE',  ( 36.65831020759688386, -273.4075654051913489, -259.1379700485984472 ) ) ;
#37416 = CARTESIAN_POINT ( 'NONE',  ( 33.47549543653630622, -277.7707624468934000, -293.3010179413162746 ) ) ;
#37417 = CARTESIAN_POINT ( 'NONE',  ( 35.47108514671395341, -291.8330373702094676, -285.9015887351851575 ) ) ;
#37418 = CARTESIAN_POINT ( 'NONE',  ( -96.74347011726838730, -281.0521018647543201, -223.3320290363749052 ) ) ;
#37419 = VERTEX_POINT ( 'NONE', #6657 ) ;
#37420 = CARTESIAN_POINT ( 'NONE',  ( -88.91222810340087790, -283.4677924453893638, -322.1289812723898649 ) ) ;
#37421 = CARTESIAN_POINT ( 'NONE',  ( 14.94051194281458272, -281.8481122527446701, -214.1809348605969205 ) ) ;
#37422 = CARTESIAN_POINT ( 'NONE',  ( -83.65540756307696313, -282.4663591245457042, -331.4445557061848717 ) ) ;
#37423 = CARTESIAN_POINT ( 'NONE',  ( -37.11558689573416103, -277.9905979907121036, -347.1385107681607565 ) ) ;
#37424 = EDGE_CURVE ( 'NONE', #60290, #22436, #86161, .T. ) ;
#37425 = CARTESIAN_POINT ( 'NONE',  ( 37.53464399305568833, -276.8866896574489260, -255.6559880793029436 ) ) ;
#37426 = CARTESIAN_POINT ( 'NONE',  ( 30.91033621190086578, -284.2662352645559167, -285.9065529553535612 ) ) ;
#37427 = ORIENTED_EDGE ( 'NONE', *, *, #24079, .F. ) ;
#37428 = VERTEX_POINT ( 'NONE', #9 ) ;
#37429 = CARTESIAN_POINT ( 'NONE',  ( -72.62788948468970318, -299.5851584109141754, -204.1658256102697351 ) ) ;
#37430 = CARTESIAN_POINT ( 'NONE',  ( -34.86053410962789911, -293.1637250275788915, -197.0940046946069515 ) ) ;
#37431 = CARTESIAN_POINT ( 'NONE',  ( -39.22395163547692931, -275.0960027690621246, -344.9821869586905336 ) ) ;
#37432 = CARTESIAN_POINT ( 'NONE',  ( -20.69626094271407979, -290.6015799094691943, -344.5561741243666347 ) ) ;
#37433 = CARTESIAN_POINT ( 'NONE',  ( 2.302737598095225824, -291.9469556524445579, -208.8828204492067186 ) ) ;
#37434 = CARTESIAN_POINT ( 'NONE',  ( 28.84760934183840320, -287.5712474710974220, -309.5848635329697913 ) ) ;
#37435 = CARTESIAN_POINT ( 'NONE',  ( 185.4166944662832179, 275.5000000000000568, 23.37680765314684450 ) ) ;
#37436 = CARTESIAN_POINT ( 'NONE',  ( -106.3053458097900545, -283.2990620952488712, -244.0845887565276371 ) ) ;
#37437 = CARTESIAN_POINT ( 'NONE',  ( -110.7883500286502994, -282.9532948857978454, -276.3858478210781868 ) ) ;
#37438 = EDGE_CURVE ( 'NONE', #85642, #69004, #5153, .T. ) ;
#37439 = CARTESIAN_POINT ( 'NONE',  ( -34.30963654725553624, -281.4062089212936826, -196.9179096800454545 ) ) ;
#37440 = CARTESIAN_POINT ( 'NONE',  ( -103.5892900021988225, -290.9858905439799059, -309.2486624744716437 ) ) ;
#37441 = CARTESIAN_POINT ( 'NONE',  ( -110.0280072607155120, -279.1483716307774898, -262.4806057647502371 ) ) ;
#37442 = CARTESIAN_POINT ( 'NONE',  ( -6.035099822276707826, -291.2494487402477716, -200.4333443729489659 ) ) ;
#37443 = CARTESIAN_POINT ( 'NONE',  ( 35.69234767254293672, -288.0520029906149944, -246.3124450938470034 ) ) ;
#37444 = CARTESIAN_POINT ( 'NONE',  ( 32.65343452309119243, -287.6344093156233725, -238.2921932989166862 ) ) ;
#37445 = CARTESIAN_POINT ( 'NONE',  ( -102.2393619153125144, -285.1732299390026810, -236.9351774717262060 ) ) ;
#37446 = ORIENTED_EDGE ( 'NONE', *, *, #90775, .F. ) ;
#37447 = CARTESIAN_POINT ( 'NONE',  ( 220.4471435719830197, 34.91984470236808136, -7.000000000000000888 ) ) ;
#37448 = CARTESIAN_POINT ( 'NONE',  ( -70.38082524794387496, -293.4817050468574280, -202.1795831189753869 ) ) ;
#37449 = CARTESIAN_POINT ( 'NONE',  ( -27.82588600098905118, -293.6186922873910703, -346.3268312306767598 ) ) ;
#37450 = CARTESIAN_POINT ( 'NONE',  ( -8.657531191722618757, -275.7260967845510891, -337.7588768899171896 ) ) ;
#37451 = CARTESIAN_POINT ( 'NONE',  ( -80.56086804385851963, -296.8318437976121800, -206.6935125192828480 ) ) ;
#37452 = CARTESIAN_POINT ( 'NONE',  ( 23.16819565115745405, -291.4510493263329067, -228.2763003371824766 ) ) ;
#37453 = CARTESIAN_POINT ( 'NONE',  ( -109.8823183692600907, -294.6000381193005637, -285.1155726733708775 ) ) ;
#37454 = CARTESIAN_POINT ( 'NONE',  ( 2.442912765373550510, -293.8031455063644444, -208.6217891557181474 ) ) ;
#37455 = CARTESIAN_POINT ( 'NONE',  ( 31.11214059008991129, -294.2829109717696952, -244.1256884269543264 ) ) ;
#37456 = LINE ( 'NONE', #51658, #61137 ) ;
#37457 = CARTESIAN_POINT ( 'NONE',  ( -70.03408964624055955, -293.4815471591751930, -338.0601135973089413 ) ) ;
#37458 = CARTESIAN_POINT ( 'NONE',  ( -110.6383152259951714, -298.3474752891375488, -286.3140909482042957 ) ) ;
#37459 = CARTESIAN_POINT ( 'NONE',  ( -37.25574734936045473, -289.9923039856906826, -343.5963626472061492 ) ) ;
#37460 = CARTESIAN_POINT ( 'NONE',  ( 6.078919257242056062, -294.7781340909078835, -329.1330549387660653 ) ) ;
#37461 = CARTESIAN_POINT ( 'NONE',  ( -105.9326596929985698, -280.9410224564196028, -239.0314339285689584 ) ) ;
#37462 = CARTESIAN_POINT ( 'NONE',  ( -92.70524414728711804, -277.9642826135986979, -217.4822590635860422 ) ) ;
#37463 = VERTEX_POINT ( 'NONE', #71048 ) ;
#37464 = CARTESIAN_POINT ( 'NONE',  ( -34.09918009706371578, -273.4405203420124622, -193.5314436979977302 ) ) ;
#37465 = CARTESIAN_POINT ( 'NONE',  ( 21.30055889832789617, -280.2658364039197636, -316.2130498709144035 ) ) ;
#37466 = CARTESIAN_POINT ( 'NONE',  ( -53.57002169826647275, -278.2473137609144374, -195.8552417591963035 ) ) ;
#37467 = CARTESIAN_POINT ( 'NONE',  ( -105.7400412630732518, -276.9616102279749157, -239.0638665336492750 ) ) ;
#37468 = CARTESIAN_POINT ( 'NONE',  ( -109.1055128195557700, -271.3400360307750248, -254.0721613814322950 ) ) ;
#37469 = DIRECTION ( 'NONE',  ( 0.000000000000000000, 0.000000000000000000, -1.000000000000000000 ) ) ;
#37470 = CARTESIAN_POINT ( 'NONE',  ( 153.8059597141930510, 20.39660080186459723, 12.88664367905129104 ) ) ;
#37471 = CARTESIAN_POINT ( 'NONE',  ( -110.9638905495010874, -288.3669261625742024, -286.4290949801811621 ) ) ;
#37472 = CARTESIAN_POINT ( 'NONE',  ( -114.0068376344051018, -290.6487534309579246, -262.6369593465452681 ) ) ;
#37473 = CARTESIAN_POINT ( 'NONE',  ( -38.35877714513877379, -276.0395859228228232, -195.2013283002371793 ) ) ;
#37474 = CARTESIAN_POINT ( 'NONE',  ( -67.53628947469199773, -295.6549983629083727, -201.8758242723695844 ) ) ;
#37475 = CARTESIAN_POINT ( 'NONE',  ( -101.2904462688696725, -283.1863939766353155, -313.0560977462169490 ) ) ;
#37476 = DIRECTION ( 'NONE',  ( -1.000000000000000000, 0.000000000000000000, 0.000000000000000000 ) ) ;
#37477 = CARTESIAN_POINT ( 'NONE',  ( 34.95251751390191686, -279.8093045300353765, -290.3720257522728616 ) ) ;
#37478 = DIRECTION ( 'NONE',  ( -1.000000000000000000, -0.000000000000000000, -0.000000000000000000 ) ) ;
#37479 = CARTESIAN_POINT ( 'NONE',  ( 25.19418736623600097, -291.8191474391782094, -231.8407379668302326 ) ) ;
#37480 = CARTESIAN_POINT ( 'NONE',  ( -71.72971496733919139, -283.7322233382939203, -204.5710737661032965 ) ) ;
#37481 = CARTESIAN_POINT ( 'NONE',  ( 195.0811277904324754, 27.48493576247232895, 15.19607843137254477 ) ) ;
#37482 = CARTESIAN_POINT ( 'NONE',  ( 82.68040262957964615, -297.0801184085799491, -195.3611179825600175 ) ) ;
#37483 = CARTESIAN_POINT ( 'NONE',  ( 32.70516106426969571, -291.2035751602908817, -243.5574263739953551 ) ) ;
#37484 = CARTESIAN_POINT ( 'NONE',  ( -69.58271295524120603, -279.0838550669636220, -336.7600244727085510 ) ) ;
#37485 = CARTESIAN_POINT ( 'NONE',  ( -55.59263170166233436, -284.4870809741044013, -344.7581086082990396 ) ) ;
#37487 = CARTESIAN_POINT ( 'NONE',  ( -52.08893400525370510, -285.8580710583424320, -198.8662294032218369 ) ) ;
#37486 = CARTESIAN_POINT ( 'NONE',  ( -4.430786967408551824, -272.5622822969111212, -202.3308065067057271 ) ) ;
#37488 = CARTESIAN_POINT ( 'NONE',  ( 35.60219635229639579, -276.8501768434589962, -260.6367731040798503 ) ) ;
#37489 = CARTESIAN_POINT ( 'NONE',  ( -51.30170664368912981, -278.0380690717825019, -342.1783857148822108 ) ) ;
#37490 = CARTESIAN_POINT ( 'NONE',  ( -91.95719958110348102, -285.8317855447812121, -321.7817660464956475 ) ) ;
#37491 = TOROIDAL_SURFACE ( 'NONE', #38974, 160.1282194813176716, 1.000000000000000000 ) ;
#37492 = VERTEX_POINT ( 'NONE', #43094 ) ;
#37493 = FACE_OUTER_BOUND ( 'NONE', #39336, .T. ) ;
#37494 = CARTESIAN_POINT ( 'NONE',  ( -68.22812767807562295, -295.2800603224667384, -340.8950006044734096 ) ) ;
#37495 = CARTESIAN_POINT ( 'NONE',  ( -35.92701835163976654, -288.0498750724642036, -195.7297205570683616 ) ) ;
#37496 = DIRECTION ( 'NONE',  ( 0.000000000000000000, 0.000000000000000000, 1.000000000000000000 ) ) ;
#37497 = CARTESIAN_POINT ( 'NONE',  ( -88.52914483777347243, -293.1952119285919025, -334.4957818155094174 ) ) ;
#37498 = CARTESIAN_POINT ( 'NONE',  ( -79.72844130231119664, -278.4143771956909177, -206.3845385109265180 ) ) ;
#37499 = CARTESIAN_POINT ( 'NONE',  ( -97.70193146623168445, -289.5794152206813123, -223.8310577723109702 ) ) ;
#37500 = CARTESIAN_POINT ( 'NONE',  ( -108.7604235962452037, -285.8347357563053492, -288.5290483093402827 ) ) ;
#37501 = CARTESIAN_POINT ( 'NONE',  ( -94.74039640288346220, -280.9646091686304885, -223.6346406665721531 ) ) ;
#37502 = CARTESIAN_POINT ( 'NONE',  ( 36.57903236361585186, -289.2214678645232198, -289.7087690605700345 ) ) ;
#37503 = CARTESIAN_POINT ( 'NONE',  ( 4.527285024688798565, -284.4878019337590445, -332.6492585765331569 ) ) ;
#37504 = CARTESIAN_POINT ( 'NONE',  ( 1.048875562918027970, -276.7215340536763506, -337.1686097628556809 ) ) ;
#37505 = CARTESIAN_POINT ( 'NONE',  ( -97.74651051932343648, -271.1564459011171948, -226.1016842667979176 ) ) ;
#37506 = CARTESIAN_POINT ( 'NONE',  ( -112.4012560575572905, -278.6003003003949061, -253.1837180568203394 ) ) ;
#37507 = CARTESIAN_POINT ( 'NONE',  ( -55.67144113608279810, -299.7346915498959561, -198.1597643774171900 ) ) ;
#37508 = DIRECTION ( 'NONE',  ( 0.000000000000000000, 0.000000000000000000, -1.000000000000000000 ) ) ;
#37509 = CARTESIAN_POINT ( 'NONE',  ( 31.98288692825981272, -284.4805209788416960, -303.7098442033569654 ) ) ;
#37510 = CARTESIAN_POINT ( 'NONE',  ( 11.15640338229844275, -272.9526403292505847, -211.7956515749848165 ) ) ;
#37511 = CARTESIAN_POINT ( 'NONE',  ( 113.5000000000000568, -218.8335761803644743, -490.8867980474134356 ) ) ;
#37512 = CARTESIAN_POINT ( 'NONE',  ( -109.1914814245206173, -278.2344627587875721, -257.1098022196482020 ) ) ;
#37513 = CARTESIAN_POINT ( 'NONE',  ( 36.50694323011791198, -277.0141089910986807, -290.7665520423612406 ) ) ;
#37514 = CARTESIAN_POINT ( 'NONE',  ( -113.6711810870028359, -283.5085031039642445, -278.5238717547131841 ) ) ;
#37515 = CARTESIAN_POINT ( 'NONE',  ( -26.30190637799861264, -290.6700151387158257, -343.5982377934620331 ) ) ;
#37516 = CARTESIAN_POINT ( 'NONE',  ( -15.08150901362087204, -299.8461792891959590, -194.0488100198521693 ) ) ;
#37517 = CARTESIAN_POINT ( 'NONE',  ( -112.7509503946451872, -297.9265635157346424, -256.8906431035279638 ) ) ;
#37518 = CARTESIAN_POINT ( 'NONE',  ( -38.96218905668040122, -294.0319303719762729, -195.5453278999278268 ) ) ;
#37519 = CARTESIAN_POINT ( 'NONE',  ( 15.19405727760773495, -280.3087349704866256, -323.7259149928286774 ) ) ;
#37520 = CARTESIAN_POINT ( 'NONE',  ( 1.489159096981346408, -272.5939989760689741, -206.6115205403624770 ) ) ;
#37521 = CARTESIAN_POINT ( 'NONE',  ( -108.5480278508402705, -285.8035598545636162, -297.6391946151897514 ) ) ;
#37522 = CARTESIAN_POINT ( 'NONE',  ( -88.88814336202254651, -288.7177959898705240, -322.4877931423029054 ) ) ;
#37523 = CARTESIAN_POINT ( 'NONE',  ( -112.5291768906040630, -274.3922002906971898, -284.1740904352106440 ) ) ;
#37524 = ORIENTED_EDGE ( 'NONE', *, *, #67573, .F. ) ;
#37525 = CARTESIAN_POINT ( 'NONE',  ( 36.56981266951201803, -286.3713841404104414, -289.7439601455833440 ) ) ;
#37526 = CARTESIAN_POINT ( 'NONE',  ( -31.87400628591920082, -288.6481172002576727, -343.2279066006028643 ) ) ;
#37527 = EDGE_LOOP ( 'NONE', ( #7874, #51537, #75848, #15666 ) ) ;
#37528 = CARTESIAN_POINT ( 'NONE',  ( -113.5142202591188720, -285.7435972221371117, -261.4594503700303108 ) ) ;
#37529 = CARTESIAN_POINT ( 'NONE',  ( 32.11960236385683487, -276.1841455350033243, -292.8825509497615940 ) ) ;
#37530 = CARTESIAN_POINT ( 'NONE',  ( -8.614199152875432475, -291.3397673769372318, -199.2539931800049260 ) ) ;
#37531 = CARTESIAN_POINT ( 'NONE',  ( 34.49524211914257421, -282.5513700882429475, -297.7977087862402072 ) ) ;
#37532 = EDGE_CURVE ( 'NONE', #74793, #87260, #79554, .T. ) ;
#37533 = CARTESIAN_POINT ( 'NONE',  ( 35.50797613771576522, -282.7844060178347263, -247.6535769292032967 ) ) ;
#37534 = CARTESIAN_POINT ( 'NONE',  ( 13.66995374275020936, -282.6938633923983275, -328.0823601178042850 ) ) ;
#37535 = CARTESIAN_POINT ( 'NONE',  ( -3.142946668124080745, -280.8502914417632610, -205.8292431900194117 ) ) ;
#37536 = CARTESIAN_POINT ( 'NONE',  ( -82.08285599513421005, -294.9094976428775681, -214.2051214447836571 ) ) ;
#37537 = CARTESIAN_POINT ( 'NONE',  ( 200.3681379904781465, 289.3007429391860228, -97.55793450621084162 ) ) ;
#37538 = ORIENTED_EDGE ( 'NONE', *, *, #28382, .T. ) ;
#37539 = CARTESIAN_POINT ( 'NONE',  ( -110.8391933014092245, -280.3702994153910595, -284.5051734269482040 ) ) ;
#37540 = CARTESIAN_POINT ( 'NONE',  ( 83.59802325294344882, 83.57088953122406849, -301.7212683633755432 ) ) ;
#37541 = CARTESIAN_POINT ( 'NONE',  ( -89.82948962184238439, -228.9372499028087304, -344.6302353727376158 ) ) ;
#37542 = CARTESIAN_POINT ( 'NONE',  ( -110.4760564755729746, -295.9223227184746747, -268.7223453535407884 ) ) ;
#37543 = CARTESIAN_POINT ( 'NONE',  ( 36.22997111948400573, -292.7769263796104724, -247.8503185055625693 ) ) ;
#37544 = CARTESIAN_POINT ( 'NONE',  ( 161.3931422174006514, 217.5860020225172491, -202.5160790841660514 ) ) ;
#37546 = CARTESIAN_POINT ( 'NONE',  ( -40.00720749556981559, -287.4859398097393637, -344.1630921471895022 ) ) ;
#37545 = CARTESIAN_POINT ( 'NONE',  ( -20.65166408309490365, -296.8319791780506876, -193.9542942158973631 ) ) ;
#37547 = CARTESIAN_POINT ( 'NONE',  ( -102.5410590905519399, -297.9361215806902692, -305.8563158083793496 ) ) ;
#37548 = CARTESIAN_POINT ( 'NONE',  ( -57.54593055370612120, -287.1011297558742967, -199.6467516099031343 ) ) ;
#37549 = ORIENTED_EDGE ( 'NONE', *, *, #84148, .F. ) ;
#37550 = CARTESIAN_POINT ( 'NONE',  ( -13.84264205821067506, -295.6957170467346145, -343.4406259332304217 ) ) ;
#37551 = CARTESIAN_POINT ( 'NONE',  ( -77.08779614944982939, -285.9963523650653201, -208.9966326678652706 ) ) ;
#37552 = CARTESIAN_POINT ( 'NONE',  ( -37.59088967158061934, -296.8440274397970597, -193.7585943611897221 ) ) ;
#37553 = CARTESIAN_POINT ( 'NONE',  ( -7.262855828185701412, -293.2395587303224147, -199.6402367457031062 ) ) ;
#37554 = CARTESIAN_POINT ( 'NONE',  ( 23.98372463674631661, -294.6639772559295807, -316.8231366738565953 ) ) ;
#37555 = CARTESIAN_POINT ( 'NONE',  ( -67.80312578678240243, -291.8075635755508870, -204.0065849163114251 ) ) ;
#37556 = ORIENTED_EDGE ( 'NONE', *, *, #69734, .T. ) ;
#37557 = CARTESIAN_POINT ( 'NONE',  ( 157.2832821354283794, 16.68119283998523272, 9.201835683359835372 ) ) ;
#37558 = CARTESIAN_POINT ( 'NONE',  ( -78.08602790601095478, -275.4291078910717374, -206.7276837630186321 ) ) ;
#37559 = CARTESIAN_POINT ( 'NONE',  ( -2.723187585705332037, -273.2944696992763625, -202.0122574492627052 ) ) ;
#37560 = EDGE_CURVE ( 'NONE', #43675, #40890, #45948, .T. ) ;
#37561 = ORIENTED_EDGE ( 'NONE', *, *, #55070, .F. ) ;
#37562 = CARTESIAN_POINT ( 'NONE',  ( -89.17528491032298632, -277.2661824618260766, -327.2188913447552068 ) ) ;
#37563 = AXIS2_PLACEMENT_3D ( 'NONE', #6408, #72216, #15367 ) ;
#37564 = CARTESIAN_POINT ( 'NONE',  ( -36.45371137686723984, -296.5433422393704745, -196.6680143152582048 ) ) ;
#37565 = CARTESIAN_POINT ( 'NONE',  ( -21.41065430713900497, -274.9854101818856975, -342.9196221950773520 ) ) ;
#37566 = CARTESIAN_POINT ( 'NONE',  ( -94.86377687975156903, -274.2704227116444144, -224.9140414991398984 ) ) ;
#37567 = CARTESIAN_POINT ( 'NONE',  ( -104.6005375515376272, -273.8830666450586477, -241.2557143445264956 ) ) ;
#37568 = CARTESIAN_POINT ( 'NONE',  ( -111.4599002293362702, -274.5245255676214811, -253.6139859404296715 ) ) ;
#37569 = ADVANCED_FACE ( 'NONE', ( #93275 ), #76178, .T. ) ;
#37570 = CARTESIAN_POINT ( 'NONE',  ( 10.75566765627312726, -272.7329247175058526, -212.2842431649167168 ) ) ;
#37571 = CARTESIAN_POINT ( 'NONE',  ( -97.26218134082830602, -296.6204925839485895, -312.2350788598213285 ) ) ;
#37572 = CARTESIAN_POINT ( 'NONE',  ( 33.68064685724496599, -292.3799151794447084, -289.6755657358717144 ) ) ;
#37573 = CARTESIAN_POINT ( 'NONE',  ( 193.9646936176701786, 21.00000000000000000, -15.00000000000000000 ) ) ;
#37574 = CARTESIAN_POINT ( 'NONE',  ( -41.37494481440511152, -277.5939710936997926, -347.2069905948220025 ) ) ;
#37575 = CARTESIAN_POINT ( 'NONE',  ( 35.60205065226340793, -275.7709323924987075, -274.3105143076345485 ) ) ;
#37576 = CARTESIAN_POINT ( 'NONE',  ( -105.3534839891285060, -282.7811752266095482, -305.5152443238438877 ) ) ;
#37577 = CARTESIAN_POINT ( 'NONE',  ( -97.63743886441584152, -299.1640323921772051, -225.4569763027148781 ) ) ;
#37578 = DIRECTION ( 'NONE',  ( 0.000000000000000000, 0.000000000000000000, -1.000000000000000000 ) ) ;
#37579 = CARTESIAN_POINT ( 'NONE',  ( -8.181212030536782365, -285.6412765830118019, -203.2621786373384509 ) ) ;
#37580 = CARTESIAN_POINT ( 'NONE',  ( -83.65810834634042692, -275.9371548799731499, -328.1571939332554280 ) ) ;
#37581 = CARTESIAN_POINT ( 'NONE',  ( -99.68384909428412755, -276.5901503890083859, -309.5566113658804852 ) ) ;
#37582 = CARTESIAN_POINT ( 'NONE',  ( 26.96455796263020588, -283.0343519342358150, -231.6655152765091827 ) ) ;
#37583 = CARTESIAN_POINT ( 'NONE',  ( 28.20906473603430697, -276.3115109789105190, -237.3425212625459437 ) ) ;
#37584 = CARTESIAN_POINT ( 'NONE',  ( 164.2231345125756263, 296.7472757692770529, 7.499999999999996447 ) ) ;
#37585 = CARTESIAN_POINT ( 'NONE',  ( 37.43763592253894501, -273.7669438095991268, -255.7155958976435386 ) ) ;
#37586 = CARTESIAN_POINT ( 'NONE',  ( -98.76589622790213241, -281.1395390408788444, -227.0356455514520349 ) ) ;
#37587 = CARTESIAN_POINT ( 'NONE',  ( 165.2494399300530290, 8.542400036368780647, -9.000000000000001776 ) ) ;
#37588 = CARTESIAN_POINT ( 'NONE',  ( 8.909657572472564624, -288.6012342047308152, -210.6105857170054776 ) ) ;
#37589 = CARTESIAN_POINT ( 'NONE',  ( -98.34275362693919931, -287.9582406316378638, -314.0163152306072334 ) ) ;
#37590 = DIRECTION ( 'NONE',  ( -0.000000000000000000, -1.000000000000000000, -0.000000000000000000 ) ) ;
#37591 = CARTESIAN_POINT ( 'NONE',  ( -108.4126790972154453, -271.4847261399625609, -251.4535893715823534 ) ) ;
#37592 = CARTESIAN_POINT ( 'NONE',  ( -108.1371321504643959, -288.3985911579586627, -292.8667624560513900 ) ) ;
#37593 = CARTESIAN_POINT ( 'NONE',  ( 197.9738562182569694, 296.4636489450776367, -54.00000000000000711 ) ) ;
#37594 = CARTESIAN_POINT ( 'NONE',  ( 197.3133474189782248, 42.36571313990103960, 12.74999999999998757 ) ) ;
#37595 = CARTESIAN_POINT ( 'NONE',  ( 37.98733281522758887, -286.1897379819343996, -282.8574360961315506 ) ) ;
#37596 = CARTESIAN_POINT ( 'NONE',  ( -53.84900324873385813, -284.8675625642646310, -342.3439394815155197 ) ) ;
#37597 = CARTESIAN_POINT ( 'NONE',  ( -104.5255380858709344, -283.2577979975578160, -234.7477315733243870 ) ) ;
#37598 = CARTESIAN_POINT ( 'NONE',  ( -101.1236770562101981, -291.0389213455058552, -234.7487109493455932 ) ) ;
#37599 = CARTESIAN_POINT ( 'NONE',  ( 19.27792113855783285, -282.3158793617697597, -223.3352547110860655 ) ) ;
#37600 = CARTESIAN_POINT ( 'NONE',  ( 15.95048526883005557, -283.0756710360772672, -320.5595098475272948 ) ) ;
#37601 = CARTESIAN_POINT ( 'NONE',  ( -111.5098345817626040, -292.3608566650248690, -283.7565790884347052 ) ) ;
#37602 = CARTESIAN_POINT ( 'NONE',  ( -34.04909031562004884, -298.2589888633038413, -193.3610277050512707 ) ) ;
#37603 = CARTESIAN_POINT ( 'NONE',  ( 4.734782201528179968, -286.5685885933644954, -333.1216456320078123 ) ) ;
#37604 = CARTESIAN_POINT ( 'NONE',  ( 33.01976959949786306, -275.9513472451616849, -301.6383233848166583 ) ) ;
#37605 = CARTESIAN_POINT ( 'NONE',  ( -47.23691339035758574, -293.9057003455085919, -196.3750952792245528 ) ) ;
#37606 = DIRECTION ( 'NONE',  ( 1.000000000000000000, -0.000000000000000000, -0.000000000000000000 ) ) ;
#37607 = CARTESIAN_POINT ( 'NONE',  ( -106.6662871844225293, -287.4805209788416391, -237.0123917617630980 ) ) ;
#37608 = CARTESIAN_POINT ( 'NONE',  ( -32.12731403894525073, -281.6698216102062133, -343.6690551796345403 ) ) ;
#37609 = CARTESIAN_POINT ( 'NONE',  ( -105.9143137401185442, -276.1477636336859405, -301.2746351304886048 ) ) ;
#37610 = EDGE_LOOP ( 'NONE', ( #65047, #57827, #92251 ) ) ;
#37611 = DIRECTION ( 'NONE',  ( 1.000000000000000000, 0.000000000000000000, 0.000000000000000000 ) ) ;
#37612 = CARTESIAN_POINT ( 'NONE',  ( -105.7857231747956916, -295.3866671249630826, -236.8669972660001406 ) ) ;
#37613 = CARTESIAN_POINT ( 'NONE',  ( 35.68928468134305376, -274.8451466765188798, -266.1413440818419076 ) ) ;
#37614 = CARTESIAN_POINT ( 'NONE',  ( -104.1933360997721394, -292.4869027017095959, -239.3519819349652948 ) ) ;
#37615 = CARTESIAN_POINT ( 'NONE',  ( -69.13054301742045027, -292.5647597207795343, -204.3709258588713737 ) ) ;
#37616 = CARTESIAN_POINT ( 'NONE',  ( -109.0698126027523926, -286.0747161948644361, -288.6108274780153806 ) ) ;
#37617 = CARTESIAN_POINT ( 'NONE',  ( 37.78132488123052468, -295.1543623217763752, -284.4010640732971638 ) ) ;
#37618 = CARTESIAN_POINT ( 'NONE',  ( 22.71049668625461848, -294.2289691711235946, -222.9373213547489456 ) ) ;
#37619 = CARTESIAN_POINT ( 'NONE',  ( -109.3632621996024881, -296.2283329583613067, -282.2730700179022847 ) ) ;
#37620 = CARTESIAN_POINT ( 'NONE',  ( 9.241551642968731883, -290.4123875611823564, -329.1403770801458677 ) ) ;
#37621 = CARTESIAN_POINT ( 'NONE',  ( -90.43660223440669199, -283.9454276347947825, -326.2009835950146908 ) ) ;
#37622 = CARTESIAN_POINT ( 'NONE',  ( -45.94125219169887231, -296.0237547665257125, -195.2920704253969859 ) ) ;
#37623 = CARTESIAN_POINT ( 'NONE',  ( -101.4203214609275108, -283.8224439033913313, -313.1525799021392231 ) ) ;
#37624 = CARTESIAN_POINT ( 'NONE',  ( -51.57026404567798039, -279.2149392249379503, -343.6372721431823152 ) ) ;
#37625 = ADVANCED_FACE ( 'NONE', ( #71999 ), #7118, .T. ) ;
#37626 = CARTESIAN_POINT ( 'NONE',  ( -110.7878736959665105, -283.3400389017655812, -270.8969657661165229 ) ) ;
#37627 = AXIS2_PLACEMENT_3D ( 'NONE', #32376, #11042, #76401 ) ;
#37628 = CARTESIAN_POINT ( 'NONE',  ( 6.737930832372755141, -286.4529149418784186, -331.1045233509693162 ) ) ;
#37629 = CARTESIAN_POINT ( 'NONE',  ( -85.99312505032125387, -277.5262283533841128, -212.2122561871963171 ) ) ;
#37630 = CARTESIAN_POINT ( 'NONE',  ( -53.17117378510891967, -153.5335516589311737, -364.2630158522994179 ) ) ;
#37631 = CARTESIAN_POINT ( 'NONE',  ( -110.3805893628636881, -284.0166549049548053, -273.6346452700706777 ) ) ;
#37632 = CARTESIAN_POINT ( 'NONE',  ( 8.297596240448868343, -281.8659182009773190, -208.7723215107029091 ) ) ;
#37633 = CARTESIAN_POINT ( 'NONE',  ( -41.75903509417830861, -288.1652468606594084, -347.0118059888877724 ) ) ;
#37634 = CARTESIAN_POINT ( 'NONE',  ( -23.06855666265645510, -278.4727810662645311, -345.2660467195866545 ) ) ;
#37635 = CARTESIAN_POINT ( 'NONE',  ( -34.29386784849671699, -278.3297499137577802, -346.8072362108209745 ) ) ;
#37636 = CARTESIAN_POINT ( 'NONE',  ( -62.30695293087269704, -279.5516311147617898, -201.7093929148592224 ) ) ;
#37637 = CARTESIAN_POINT ( 'NONE',  ( -49.16017066696437610, -275.8808498938869889, -196.6055294434982272 ) ) ;
#37638 = CARTESIAN_POINT ( 'NONE',  ( 25.07699264894857905, -284.9922498286451287, -228.9885039889509812 ) ) ;
#37639 = CARTESIAN_POINT ( 'NONE',  ( -82.36340345759107606, -291.2555654027345895, -331.8386475591551630 ) ) ;
#37640 = CARTESIAN_POINT ( 'NONE',  ( -39.71275232492541107, -294.0029185774877192, -343.6443603086365783 ) ) ;
#37641 = VERTEX_POINT ( 'NONE', #28888 ) ;
#37642 = CARTESIAN_POINT ( 'NONE',  ( 34.08737187044444994, -293.4196534637811169, -285.5860100850539993 ) ) ;
#37643 = CARTESIAN_POINT ( 'NONE',  ( -56.12643432226993667, -292.8954854425140866, -195.9516550952625096 ) ) ;
#37644 = CARTESIAN_POINT ( 'NONE',  ( 34.43274187487774185, -282.0200121692074049, -256.4271846446987979 ) ) ;
#37645 = CARTESIAN_POINT ( 'NONE',  ( -30.50496736591661318, -297.0561975967531794, -193.6714471065133978 ) ) ;
#37646 = CARTESIAN_POINT ( 'NONE',  ( 18.27203574674027209, -287.4756648982031493, -217.1766575721160848 ) ) ;
#37647 = ADVANCED_FACE ( 'NONE', ( #6181 ), #3469, .F. ) ;
#37648 = CARTESIAN_POINT ( 'NONE',  ( -68.04154480222608470, -289.7776306228537919, -340.9533543019367130 ) ) ;
#37649 = CARTESIAN_POINT ( 'NONE',  ( 2.454985290050144986, -286.9352139954348218, -209.1376640089450518 ) ) ;
#37650 = LINE ( 'NONE', #81671, #73222 ) ;
#37651 = CARTESIAN_POINT ( 'NONE',  ( -84.92324064171599218, -218.1701808897174715, -350.4119417867636344 ) ) ;
#37652 = CARTESIAN_POINT ( 'NONE',  ( 192.6544724140480582, 276.0552902512551441, -124.0055601186182059 ) ) ;
#37653 = CARTESIAN_POINT ( 'NONE',  ( -76.45075835905313966, -276.7867205270100612, -332.2517913679837989 ) ) ;
#37654 = CARTESIAN_POINT ( 'NONE',  ( -97.91194419254118486, -276.9003649770493212, -311.6584739244761977 ) ) ;
#37655 = CARTESIAN_POINT ( 'NONE',  ( -97.79382389457855140, -272.8564731349133012, -222.7031173553139638 ) ) ;
#37656 = CARTESIAN_POINT ( 'NONE',  ( 186.2046704664805929, 260.4489007258302991, -151.5571721899337376 ) ) ;
#37657 = CARTESIAN_POINT ( 'NONE',  ( -68.82782541750671612, -276.1423109118917409, -340.1029172073166933 ) ) ;
#37658 = CARTESIAN_POINT ( 'NONE',  ( -76.54002866929528182, -297.3286924278899050, -335.5181367140972952 ) ) ;
#37659 = CARTESIAN_POINT ( 'NONE',  ( -38.90517695359586980, -292.5243609972285412, -197.3163099394028279 ) ) ;
#37660 = CARTESIAN_POINT ( 'NONE',  ( -106.3727411092069133, -297.7892413564482581, -236.6139077118289151 ) ) ;
#37661 = CARTESIAN_POINT ( 'NONE',  ( -21.03610659092324653, -287.5233325544106151, -342.0226215668388363 ) ) ;
#37662 = CARTESIAN_POINT ( 'NONE',  ( -97.73816644073109217, -273.8410081171123807, -222.7630125149007654 ) ) ;
#37663 = CARTESIAN_POINT ( 'NONE',  ( -106.8686205551998540, -296.4218318016476701, -292.7735055452791926 ) ) ;
#37664 = VERTEX_POINT ( 'NONE', #15142 ) ;
#37665 = FACE_OUTER_BOUND ( 'NONE', #42279, .T. ) ;
#37666 = CARTESIAN_POINT ( 'NONE',  ( -111.0737817670128038, -280.2617639320028502, -286.8806318921927527 ) ) ;
#37667 = EDGE_CURVE ( 'NONE', #58191, #57853, #26288, .T. ) ;
#37668 = CARTESIAN_POINT ( 'NONE',  ( -95.04264424169875269, -280.2668934386103388, -225.1211432287273908 ) ) ;
#37669 = CARTESIAN_POINT ( 'NONE',  ( -77.26319644249774399, -279.3393431236303286, -335.0770921082039990 ) ) ;
#37670 = CARTESIAN_POINT ( 'NONE',  ( -72.21893659852504754, -272.0622194876918343, -205.3867320333394275 ) ) ;
#37671 = DIRECTION ( 'NONE',  ( 0.000000000000000000, 0.000000000000000000, 1.000000000000000000 ) ) ;
#37672 = DIRECTION ( 'NONE',  ( 1.124465274301078034E-16, 1.000000000000000000, 0.000000000000000000 ) ) ;
#37673 = CARTESIAN_POINT ( 'NONE',  ( 21.32770764968728017, -281.1095361591715118, -226.9016110156684363 ) ) ;
#37674 = CARTESIAN_POINT ( 'NONE',  ( 5.789108410471958344, -277.2864156108663565, -333.9527225772035308 ) ) ;
#37675 = CARTESIAN_POINT ( 'NONE',  ( 35.30794059788363626, -277.7916533601141964, -288.9898687286022323 ) ) ;
#37676 = CARTESIAN_POINT ( 'NONE',  ( -90.92885079171797713, -276.3691525625011423, -324.9056232648151195 ) ) ;
#37677 = EDGE_LOOP ( 'NONE', ( #56184, #87929, #19257, #43737 ) ) ;
#37678 = CARTESIAN_POINT ( 'NONE',  ( 197.3133474189782248, 24.42324672360810212, 12.74999999999999112 ) ) ;
#37679 = CARTESIAN_POINT ( 'NONE',  ( 38.06438725825336178, -283.5263374061846662, -269.9143067520816999 ) ) ;
#37680 = CARTESIAN_POINT ( 'NONE',  ( -12.19512293733743213, -291.5849070708507043, -201.6030324167746244 ) ) ;
#37681 = ADVANCED_FACE ( 'NONE', ( #8025 ), #80770, .F. ) ;
#37682 = CARTESIAN_POINT ( 'NONE',  ( 27.05693341984959233, -286.3479168327781963, -228.3357829610680199 ) ) ;
#37683 = CARTESIAN_POINT ( 'NONE',  ( -64.44706033559685920, -281.6507206309740354, -339.2325450183386693 ) ) ;
#37685 = CARTESIAN_POINT ( 'NONE',  ( 5.575143043045670765, -284.7178221125593609, -209.4748501153949576 ) ) ;
#37684 = CARTESIAN_POINT ( 'NONE',  ( 1.396174800651887260, -281.0986647465979331, -332.9885912476374301 ) ) ;
#37686 = AXIS2_PLACEMENT_3D ( 'NONE', #48555, #48086, #62815 ) ;
#37687 = CARTESIAN_POINT ( 'NONE',  ( -32.95453044752736105, -281.3137330514537666, -197.0952784151002959 ) ) ;
#37688 = CARTESIAN_POINT ( 'NONE',  ( -111.5612411848370158, -270.6950922538807731, -259.2160366785121255 ) ) ;
#37689 = CARTESIAN_POINT ( 'NONE',  ( 21.88842702488935643, -280.6018506554717646, -318.3215814268220925 ) ) ;
#37690 = CARTESIAN_POINT ( 'NONE',  ( 33.60309272334027497, -295.8689257732274882, -294.8481270805441454 ) ) ;
#37691 = CARTESIAN_POINT ( 'NONE',  ( -96.16207195449918288, -287.1941086603724216, -223.5616277089561947 ) ) ;
#37692 = LINE ( 'NONE', #75100, #45859 ) ;
#37693 = CARTESIAN_POINT ( 'NONE',  ( -74.00205074352921031, -293.4891656483618476, -204.2904520863180267 ) ) ;
#37694 = CARTESIAN_POINT ( 'NONE',  ( 37.69952133095186753, -273.5684581228775301, -271.6439160306233589 ) ) ;
#37695 = CARTESIAN_POINT ( 'NONE',  ( -46.01771493812130132, -288.3565515813159550, -346.7612723019060468 ) ) ;
#37696 = CARTESIAN_POINT ( 'NONE',  ( 34.84588310033183234, -292.1530112701957478, -285.7641872428404781 ) ) ;
#37697 = CARTESIAN_POINT ( 'NONE',  ( -43.45424580659107505, -257.5073373634913878, -441.6910188950594147 ) ) ;
#37698 = CARTESIAN_POINT ( 'NONE',  ( -108.3007510680304080, -276.9859520510550510, -289.4937228425025637 ) ) ;
#37699 = CARTESIAN_POINT ( 'NONE',  ( -96.25511390437439729, -295.3168522175690782, -225.1732222194624740 ) ) ;
#37700 = CARTESIAN_POINT ( 'NONE',  ( -66.50944301466391551, -290.7573771064948573, -337.8727843772070969 ) ) ;
#37701 = DIRECTION ( 'NONE',  ( 0.000000000000000000, 0.000000000000000000, 1.000000000000000000 ) ) ;
#37702 = CARTESIAN_POINT ( 'NONE',  ( 164.7123623445222904, 2.999999999999999112, 9.000000000000001776 ) ) ;
#37703 = CARTESIAN_POINT ( 'NONE',  ( 28.88359954126167750, -291.5350766291451805, -232.4544241809067273 ) ) ;
#37704 = CARTESIAN_POINT ( 'NONE',  ( -14.33575256702261669, -287.9554799457537229, -200.1850115788404878 ) ) ;
#37705 = CARTESIAN_POINT ( 'NONE',  ( -113.2402406540008002, -288.7456447905061054, -274.0197458076002590 ) ) ;
#37706 = CARTESIAN_POINT ( 'NONE',  ( 36.26926440092935167, -288.9501699191234820, -268.2778148346371836 ) ) ;
#37707 = DIRECTION ( 'NONE',  ( 0.9693563597868444237, 0.2456588035076248677, 0.000000000000000000 ) ) ;
#37708 = CARTESIAN_POINT ( 'NONE',  ( 30.10667718276161864, -287.9739422950855214, -241.8870976369559571 ) ) ;
#37709 = CARTESIAN_POINT ( 'NONE',  ( -63.66743565242112624, -297.3735375276176001, -340.9682171409212401 ) ) ;
#37710 = CARTESIAN_POINT ( 'NONE',  ( 159.4851178187871312, 0.000000000000000000, 7.000000000000000000 ) ) ;
#37711 = CARTESIAN_POINT ( 'NONE',  ( -74.22260853141756343, -290.7362035837512622, -337.5162988473455812 ) ) ;
#37712 = CARTESIAN_POINT ( 'NONE',  ( -35.35360162160101538, -278.0970711081669151, -195.0192884189522147 ) ) ;
#37713 = CARTESIAN_POINT ( 'NONE',  ( -19.76517645851018301, -280.6053071016204967, -195.3609824881742441 ) ) ;
#37714 = CARTESIAN_POINT ( 'NONE',  ( -82.22308794841831059, -279.1248546121124150, -207.8198890310584375 ) ) ;
#37715 = CARTESIAN_POINT ( 'NONE',  ( -73.31142217984276499, -283.5750233019674624, -204.5348150507924174 ) ) ;
#37716 = CARTESIAN_POINT ( 'NONE',  ( -111.5352550897782749, -274.3943000018521730, -270.3845729371874427 ) ) ;
#37717 = CARTESIAN_POINT ( 'NONE',  ( -1.346756639984390436, -278.6745402880802658, -205.4363189856392182 ) ) ;
#37718 = CARTESIAN_POINT ( 'NONE',  ( -57.96198189079880336, -281.3182150669873636, -342.5248510673511078 ) ) ;
#37719 = DIRECTION ( 'NONE',  ( 0.000000000000000000, 0.000000000000000000, -1.000000000000000000 ) ) ;
#37720 = CARTESIAN_POINT ( 'NONE',  ( -79.85610541683962538, -276.0952751281701012, -333.7906028290099698 ) ) ;
#37721 = CARTESIAN_POINT ( 'NONE',  ( -82.38303917391709774, -298.9449961160740941, -211.9698892282532654 ) ) ;
#37722 = CARTESIAN_POINT ( 'NONE',  ( -99.08715357158504844, -284.0802417515357092, -224.7875916228985886 ) ) ;
#37723 = CARTESIAN_POINT ( 'NONE',  ( -110.5031764828875396, -273.3548555555994426, -270.3713160627550565 ) ) ;
#37724 = CARTESIAN_POINT ( 'NONE',  ( -89.77185585563556458, -274.7552957348602831, -214.7039098860404067 ) ) ;
#37725 = CARTESIAN_POINT ( 'NONE',  ( 30.19599232763608043, -274.8453020664975952, -242.4659859445256416 ) ) ;
#37726 = CARTESIAN_POINT ( 'NONE',  ( -94.59304442827847481, -297.8818750939501001, -318.8297842443670902 ) ) ;
#37727 = CARTESIAN_POINT ( 'NONE',  ( -95.45690778130091303, -290.0360474077004369, -320.8747066884077981 ) ) ;
#37728 = CARTESIAN_POINT ( 'NONE',  ( -76.72077358112996137, -277.6096693091433281, -205.8133274144104234 ) ) ;
#37729 = CARTESIAN_POINT ( 'NONE',  ( -95.45969724777727095, -289.7027411976405347, -320.8714972655885163 ) ) ;
#37730 = CARTESIAN_POINT ( 'NONE',  ( -26.45170130298138744, -287.9690568858730444, -342.8334356260376126 ) ) ;
#37731 = CARTESIAN_POINT ( 'NONE',  ( 37.71025294593471244, -291.5516736992122446, -270.3367095491944383 ) ) ;
#37732 = ORIENTED_EDGE ( 'NONE', *, *, #4248, .F. ) ;
#37733 = CARTESIAN_POINT ( 'NONE',  ( 197.8752062525135500, 68.08088840871901937, 11.26666408104508577 ) ) ;
#37734 = CARTESIAN_POINT ( 'NONE',  ( -109.7602561260798808, -290.1922231692020091, -260.3144446255313937 ) ) ;
#37735 = DIRECTION ( 'NONE',  ( 0.000000000000000000, 0.000000000000000000, 1.000000000000000000 ) ) ;
#37736 = CARTESIAN_POINT ( 'NONE',  ( -40.81785317066410101, -286.9508117773478375, -193.6231241796697020 ) ) ;
#37737 = CARTESIAN_POINT ( 'NONE',  ( -82.08285599513421005, -298.1948066931273615, -326.5171145203363494 ) ) ;
#37738 = CARTESIAN_POINT ( 'NONE',  ( 13.23177851729148458, -293.4242757055536686, -328.1822876491806369 ) ) ;
#37739 = CARTESIAN_POINT ( 'NONE',  ( -49.99534544201929975, -284.5254039480373649, -345.8678343240129607 ) ) ;
#37740 = CARTESIAN_POINT ( 'NONE',  ( -52.08686027762424686, -285.6914178420956318, -198.8658016559107296 ) ) ;
#37741 = CARTESIAN_POINT ( 'NONE',  ( 21.86862158560414571, -276.2614182090201211, -226.8251411176449608 ) ) ;
#37742 = CARTESIAN_POINT ( 'NONE',  ( 31.37967797716864027, -291.1880930204496281, -241.0874106872614391 ) ) ;
#37743 = CARTESIAN_POINT ( 'NONE',  ( -11.33524563461924828, -273.1934724416707923, -201.6715427892335413 ) ) ;
#37744 = ORIENTED_EDGE ( 'NONE', *, *, #66611, .T. ) ;
#37745 = CARTESIAN_POINT ( 'NONE',  ( 195.8198161289002712, 42.34889664205514492, 12.33687207710887357 ) ) ;
#37746 = CARTESIAN_POINT ( 'NONE',  ( -3.241968658763197730, -294.2809074460785155, -339.3898654669944221 ) ) ;
#37747 = CARTESIAN_POINT ( 'NONE',  ( -22.19016968178731020, -288.1677394615121557, -197.4264962426103693 ) ) ;
#37748 = CARTESIAN_POINT ( 'NONE',  ( -97.99798081555323392, -298.2610521273613813, -223.4111628241926439 ) ) ;
#37749 = CARTESIAN_POINT ( 'NONE',  ( 9.088851792067538682, -287.3608727325254222, -213.8978864400777411 ) ) ;
#37750 = CARTESIAN_POINT ( 'NONE',  ( -113.8083720090882451, -277.7029385908161316, -263.0244537588394564 ) ) ;
#37751 = CARTESIAN_POINT ( 'NONE',  ( 39.13661133486895949, -294.3101867204293285, -278.8753295318030041 ) ) ;
#37752 = CARTESIAN_POINT ( 'NONE',  ( 27.82900540908005382, -286.2033991057485878, -309.0015711177097160 ) ) ;
#37753 = AXIS2_PLACEMENT_3D ( 'NONE', #53934, #32635, #33546 ) ;
#37754 = CARTESIAN_POINT ( 'NONE',  ( 24.01469349679570797, -294.5049369647204003, -316.8491514209268871 ) ) ;
#37755 = CARTESIAN_POINT ( 'NONE',  ( -87.94830204885226976, -291.6542034651085373, -217.6503829621510420 ) ) ;
#37756 = DIRECTION ( 'NONE',  ( -0.000000000000000000, -0.000000000000000000, 1.000000000000000000 ) ) ;
#37757 = CARTESIAN_POINT ( 'NONE',  ( 144.7857639756989272, -297.1570670221753971, -195.3611179825600175 ) ) ;
#37758 = CARTESIAN_POINT ( 'NONE',  ( 85.24291059907943691, 81.26895831532213776, -298.9807373496020659 ) ) ;
#37759 = CONICAL_SURFACE ( 'NONE', #90657, 5.024999999999987921, 0.7853981633974482790 ) ;
#37760 = CARTESIAN_POINT ( 'NONE',  ( 35.18394553432579386, -288.7691767095375894, -246.4701583390247492 ) ) ;
#37761 = CARTESIAN_POINT ( 'NONE',  ( 13.79469577742117181, -279.9094976428775681, -334.5364918783848793 ) ) ;
#37762 = ORIENTED_EDGE ( 'NONE', *, *, #58566, .T. ) ;
#37763 = CARTESIAN_POINT ( 'NONE',  ( -85.07341159308739975, -282.6498349985838558, -326.0020183466536992 ) ) ;
#37764 = CARTESIAN_POINT ( 'NONE',  ( -112.7737633824739731, -278.0259807495030486, -285.7803694997610933 ) ) ;
#37765 = CARTESIAN_POINT ( 'NONE',  ( 35.43902827600663841, -283.7770093004746172, -287.8224330372684108 ) ) ;
#37766 = CARTESIAN_POINT ( 'NONE',  ( -111.0078494383391643, -273.9054044750961907, -284.0227232199477498 ) ) ;
#37767 = CARTESIAN_POINT ( 'NONE',  ( -66.94390476819259561, -284.2464329214698751, -199.9174115631348343 ) ) ;
#37768 = CARTESIAN_POINT ( 'NONE',  ( 26.36739446536032361, -285.0481796969785364, -231.4638421486721995 ) ) ;
#37769 = CARTESIAN_POINT ( 'NONE',  ( -60.51620943829987453, -275.6152834882319098, -198.1728337017907506 ) ) ;
#37770 = CARTESIAN_POINT ( 'NONE',  ( -101.2714380519233686, -297.5274888796026858, -234.9919640418008271 ) ) ;
#37771 = CARTESIAN_POINT ( 'NONE',  ( -28.85555215543839225, -293.6272811269888052, -343.4140422409176381 ) ) ;
#37772 = CARTESIAN_POINT ( 'NONE',  ( -112.0741474413762688, -278.9759411383659540, -288.5373421947147676 ) ) ;
#37773 = CARTESIAN_POINT ( 'NONE',  ( 17.43522920221995776, -276.2413857850881982, -318.6343852935881387 ) ) ;
#37774 = CARTESIAN_POINT ( 'NONE',  ( -23.42491818985267926, -299.1636407243324811, -193.5942472848419698 ) ) ;
#37775 = CARTESIAN_POINT ( 'NONE',  ( -64.99649303227438679, -276.3252933695447950, -341.9483295330051078 ) ) ;
#37776 = CARTESIAN_POINT ( 'NONE',  ( -100.2953508598967574, -247.7937573541214249, -334.1010632675480565 ) ) ;
#37777 = CARTESIAN_POINT ( 'NONE',  ( -93.91613561194917281, -275.8684529495638458, -319.6178235012662299 ) ) ;
#37778 = CARTESIAN_POINT ( 'NONE',  ( -113.7215832906442330, -298.0225411687098926, -266.7811269161292671 ) ) ;
#37779 = CARTESIAN_POINT ( 'NONE',  ( -20.25526795762937127, -276.7662352645559167, -195.3538533559490702 ) ) ;
#37780 = DIRECTION ( 'NONE',  ( -1.000000000000000000, -0.000000000000000000, -0.000000000000000000 ) ) ;
#37781 = CARTESIAN_POINT ( 'NONE',  ( -56.38601138994710027, -284.3830813834740638, -341.1533511814076292 ) ) ;
#37782 = CARTESIAN_POINT ( 'NONE',  ( -108.3479269349698342, -285.9635469242175532, -297.5647797368438319 ) ) ;
#37783 = CARTESIAN_POINT ( 'NONE',  ( 30.05896838192226639, -286.5199305538867520, -241.9272974550434583 ) ) ;
#37784 = CARTESIAN_POINT ( 'NONE',  ( -88.06584979592813056, -277.7283686652557435, -216.6854663963555083 ) ) ;
#37785 = CARTESIAN_POINT ( 'NONE',  ( -108.5705212828705157, -286.1399632973974008, -291.3186634987029038 ) ) ;
#37786 = CARTESIAN_POINT ( 'NONE',  ( -67.57318300133543687, -278.1280593844198279, -203.1405009579335967 ) ) ;
#37787 = CARTESIAN_POINT ( 'NONE',  ( -72.98029933047352813, -278.6158898784741496, -334.4389367112646596 ) ) ;
#37788 = CARTESIAN_POINT ( 'NONE',  ( 197.7953982265470927, 19.09807621135331246, 10.91506350946108839 ) ) ;
#37789 = CARTESIAN_POINT ( 'NONE',  ( -108.0012170349966567, -273.2919539880256821, -251.5869293900192076 ) ) ;
#37790 = CARTESIAN_POINT ( 'NONE',  ( 37.82456592097646109, -282.1543792110126674, -254.3548339861530962 ) ) ;
#37791 = CARTESIAN_POINT ( 'NONE',  ( 2.068005410463290339, -283.0316567554436915, -336.4398741192388798 ) ) ;
#37792 = ORIENTED_EDGE ( 'NONE', *, *, #17570, .T. ) ;
#37793 = VERTEX_POINT ( 'NONE', #88011 ) ;
#37794 = CYLINDRICAL_SURFACE ( 'NONE', #85147, 7.500000000000012434 ) ;
#37795 = CARTESIAN_POINT ( 'NONE',  ( 30.59059424230705915, -289.8520486929858748, -304.0281190475556059 ) ) ;
#37796 = CARTESIAN_POINT ( 'NONE',  ( -86.20055025551432948, -296.5505580921436604, -215.9054985227050167 ) ) ;
#37797 = EDGE_CURVE ( 'NONE', #87117, #58726, #6652, .T. ) ;
#37798 = CARTESIAN_POINT ( 'NONE',  ( -72.11873837068029047, -290.9530080029579153, -201.7617707338883974 ) ) ;
#37799 = CARTESIAN_POINT ( 'NONE',  ( 21.71764038975468836, -286.6449205678022167, -314.4583285992746369 ) ) ;
#37800 = CARTESIAN_POINT ( 'NONE',  ( 6.178595397995848337, -287.0234379615165494, -329.7656499623095669 ) ) ;
#37801 = CARTESIAN_POINT ( 'NONE',  ( -71.37589818712689294, -286.7972193673790002, -205.3318640405370843 ) ) ;
#37802 = CARTESIAN_POINT ( 'NONE',  ( -94.63821083568684855, -275.8824393043251462, -318.7763050927415520 ) ) ;
#37803 = CARTESIAN_POINT ( 'NONE',  ( -59.81102077776797898, -287.7383936417400037, -343.1729991793357044 ) ) ;
#37804 = CARTESIAN_POINT ( 'NONE',  ( -29.69290381712577087, -288.1491791821498509, -195.7521603230860308 ) ) ;
#37805 = CARTESIAN_POINT ( 'NONE',  ( -64.80158629606067677, -287.4096252032110783, -340.3874302961012859 ) ) ;
#37806 = CARTESIAN_POINT ( 'NONE',  ( -10.87959983794257823, -283.6398546170017880, -338.7022512533970371 ) ) ;
#37807 = CARTESIAN_POINT ( 'NONE',  ( -61.13304196143574387, -293.7442956288926439, -199.0041141731558128 ) ) ;
#37808 = FACE_OUTER_BOUND ( 'NONE', #39837, .T. ) ;
#37809 = DIRECTION ( 'NONE',  ( 0.8946341770721968345, 0.4467993836324679613, 0.000000000000000000 ) ) ;
#37810 = CARTESIAN_POINT ( 'NONE',  ( -65.03740017501561965, -299.6134254742047460, -200.0039601905290567 ) ) ;
#37811 = CARTESIAN_POINT ( 'NONE',  ( -41.04916566346640394, -279.2014650675163239, -197.2936393989929797 ) ) ;
#37812 = CARTESIAN_POINT ( 'NONE',  ( 16.71818628295263665, -278.8207651294118818, -218.3010416923969501 ) ) ;
#37813 = CARTESIAN_POINT ( 'NONE',  ( 19.40351041030578827, -293.4558892461126902, -322.2472912541077221 ) ) ;
#37814 = CARTESIAN_POINT ( 'NONE',  ( -52.78280127321203707, -296.2509912985147480, -198.1421037400120326 ) ) ;
#37815 = CARTESIAN_POINT ( 'NONE',  ( 32.60663964426203165, -273.9665152204736387, -295.9772954130647804 ) ) ;
#37816 = CARTESIAN_POINT ( 'NONE',  ( 4.108237434672163957, -295.7956527958423294, -331.0500473937844959 ) ) ;
#37817 = CARTESIAN_POINT ( 'NONE',  ( 175.2296996224750103, 250.0000000000000568, 0.000000000000000000 ) ) ;
#37818 = CARTESIAN_POINT ( 'NONE',  ( -40.39297037167825977, -296.4944671830851348, -194.0638207371761439 ) ) ;
#37819 = CARTESIAN_POINT ( 'NONE',  ( -112.9374056294798550, -294.6944509249191810, -278.0593854609253981 ) ) ;
#37820 = CARTESIAN_POINT ( 'NONE',  ( 36.01322465072367862, -295.0542162284260144, -276.2288199817065788 ) ) ;
#37821 = DIRECTION ( 'NONE',  ( 1.000000000000000000, 0.000000000000000000, 0.000000000000000000 ) ) ;
#37822 = CARTESIAN_POINT ( 'NONE',  ( -94.06125868345739605, -296.7020844567787208, -316.5922034578405828 ) ) ;
#37823 = AXIS2_PLACEMENT_3D ( 'NONE', #25971, #46806, #61525 ) ;
#37824 = DIRECTION ( 'NONE',  ( 1.000000000000000000, 0.000000000000000000, 0.000000000000000000 ) ) ;
#37826 = CARTESIAN_POINT ( 'NONE',  ( -110.3742624300891748, -296.5736311168014367, -268.7328962846926288 ) ) ;
#37825 = CARTESIAN_POINT ( 'NONE',  ( -30.99667147627619812, -284.1520367043187321, -195.2605087894166900 ) ) ;
#37827 = CARTESIAN_POINT ( 'NONE',  ( -101.4191420572007871, -283.9890970573874256, -313.1543460418805580 ) ) ;
#37828 = CARTESIAN_POINT ( 'NONE',  ( -9.416466136213701432, -282.3344519962977301, -200.1507519025080342 ) ) ;
#37829 = CIRCLE ( 'NONE', #40780, 1.000000000000000888 ) ;
#37830 = CARTESIAN_POINT ( 'NONE',  ( 5.171536239335461360, -286.2764926188042409, -206.1231063992670727 ) ) ;
#37831 = CARTESIAN_POINT ( 'NONE',  ( -82.82360416465972719, -289.4288574986434810, -210.8697706112226626 ) ) ;
#37832 = CARTESIAN_POINT ( 'NONE',  ( -85.28047601435908120, -276.9094976428775681, -210.1954327657594206 ) ) ;
#37833 = CARTESIAN_POINT ( 'NONE',  ( 29.26390660990996651, -285.8203483262448117, -239.2976888795785442 ) ) ;
#37834 = CARTESIAN_POINT ( 'NONE',  ( -111.9651210933101595, -289.2496862974836063, -288.1045637006901643 ) ) ;
#37835 = LINE ( 'NONE', #8502, #38521 ) ;
#37836 = CARTESIAN_POINT ( 'NONE',  ( -109.3682417825332465, -297.9424386252651971, -286.4427135188584543 ) ) ;
#37837 = CARTESIAN_POINT ( 'NONE',  ( -98.11880804010954193, -280.5997480120203136, -224.0283581363119083 ) ) ;
#37839 = CARTESIAN_POINT ( 'NONE',  ( 33.13510413581197867, -280.9659617420585960, -251.2054813130784510 ) ) ;
#37838 = CARTESIAN_POINT ( 'NONE',  ( 0.9122612509525566127, -292.5644924864690211, -335.2844669534731565 ) ) ;
#37840 = CARTESIAN_POINT ( 'NONE',  ( -44.79351154302201365, -295.3105474605857808, -347.0530951707714280 ) ) ;
#37841 = CARTESIAN_POINT ( 'NONE',  ( -108.6107682297680270, -282.9546897511216912, -245.2606373344350459 ) ) ;
#37842 = CARTESIAN_POINT ( 'NONE',  ( -105.6095004350705295, -280.9612874923071786, -239.1794537842767454 ) ) ;
#37843 = CARTESIAN_POINT ( 'NONE',  ( -94.13258990755861078, -294.9582825502211563, -316.6215412285289403 ) ) ;
#37844 = CARTESIAN_POINT ( 'NONE',  ( -92.77558565261395529, -271.2595425627999361, -219.5768502237933717 ) ) ;
#37845 = ORIENTED_EDGE ( 'NONE', *, *, #59688, .T. ) ;
#37846 = CARTESIAN_POINT ( 'NONE',  ( 165.4421947725420523, 250.0000000000000568, 22.46007009812166544 ) ) ;
#37847 = CARTESIAN_POINT ( 'NONE',  ( 34.55023997769868771, -283.7916519174600580, -290.4458323788167604 ) ) ;
#37848 = CARTESIAN_POINT ( 'NONE',  ( -109.7964231187581703, -296.1886927427498222, -260.5822927291129076 ) ) ;
#37849 = DIRECTION ( 'NONE',  ( -1.000000000000000000, 0.000000000000000000, 0.000000000000000000 ) ) ;
#37850 = CARTESIAN_POINT ( 'NONE',  ( -110.4683760289727132, -281.8380690714489560, -287.0191576251351080 ) ) ;
#37851 = CARTESIAN_POINT ( 'NONE',  ( 28.36977180997978465, -274.2272177127116493, -230.4327391209765779 ) ) ;
#37852 = EDGE_CURVE ( 'NONE', #33307, #34997, #79241, .T. ) ;
#37853 = EDGE_CURVE ( 'NONE', #16441, #90518, #67209, .T. ) ;
#37854 = CARTESIAN_POINT ( 'NONE',  ( 21.12306777744842989, -289.5363890634069435, -319.7085514306408527 ) ) ;
#37855 = CARTESIAN_POINT ( 'NONE',  ( -72.62508707559196353, -291.4048058399475281, -206.3974875332536953 ) ) ;
#37856 = CARTESIAN_POINT ( 'NONE',  ( -6.496721337991925971, -281.9848599690938613, -203.4198082974186832 ) ) ;
#37857 = CARTESIAN_POINT ( 'NONE',  ( -59.73760420987919417, -275.3574279845327055, -199.9878846632465752 ) ) ;
#37858 = CARTESIAN_POINT ( 'NONE',  ( -4.154371310788768312, -279.2947154676454602, -204.8816500456040899 ) ) ;
#37859 = CARTESIAN_POINT ( 'NONE',  ( -18.49029900600233134, -278.8094562979103443, -342.9533029717113664 ) ) ;
#37860 = ORIENTED_EDGE ( 'NONE', *, *, #28287, .T. ) ;
#37861 = CARTESIAN_POINT ( 'NONE',  ( -94.14382996827848160, -273.0927270366960329, -218.3559024421128072 ) ) ;
#37862 = CARTESIAN_POINT ( 'NONE',  ( -32.07942449665793561, -294.0391766735301644, -196.0944767445531340 ) ) ;
#37863 = CARTESIAN_POINT ( 'NONE',  ( 188.7149167944524493, -12.49482340714361506, 10.00000000000000000 ) ) ;
#37864 = DIRECTION ( 'NONE',  ( -0.000000000000000000, -0.000000000000000000, -1.000000000000000000 ) ) ;
#37865 = CARTESIAN_POINT ( 'NONE',  ( 37.63316176299144900, -291.5485579843812047, -259.0961815992994843 ) ) ;
#37866 = CARTESIAN_POINT ( 'NONE',  ( -96.32734431689104326, -272.6640155438018951, -227.1646356837109977 ) ) ;
#37867 = CARTESIAN_POINT ( 'NONE',  ( 73.43068321062709458, -134.2391364535880598, 0.000000000000000000 ) ) ;
#37868 = CARTESIAN_POINT ( 'NONE',  ( 28.86439211801948446, -294.5748309556944378, -232.4208873458419191 ) ) ;
#37869 = CARTESIAN_POINT ( 'NONE',  ( -54.49178911615187815, -282.3376638359844719, -195.3683826091709363 ) ) ;
#37870 = CARTESIAN_POINT ( 'NONE',  ( -14.01819356607601463, -288.3554475995405824, -199.2009212967978158 ) ) ;
#37871 = CARTESIAN_POINT ( 'NONE',  ( 4.129456990265810923, -274.4916737323193843, -332.6521410263596294 ) ) ;
#37872 = CARTESIAN_POINT ( 'NONE',  ( 30.38624796905902059, -277.0623981502474749, -239.3457495839268745 ) ) ;
#37873 = CARTESIAN_POINT ( 'NONE',  ( -11.74248024021450476, -290.4677657347916124, -200.4062835822410023 ) ) ;
#37874 = CARTESIAN_POINT ( 'NONE',  ( -25.61058765086342248, -282.0605198663932356, -195.5100226104716796 ) ) ;
#37875 = EDGE_LOOP ( 'NONE', ( #40306, #14205, #44535, #3978 ) ) ;
#37876 = CARTESIAN_POINT ( 'NONE',  ( -58.98621574447633975, -282.6881675588109033, -340.2384550567359156 ) ) ;
#37877 = CARTESIAN_POINT ( 'NONE',  ( -70.15622494353128502, -278.5540352753159254, -339.6914360324055906 ) ) ;
#37878 = CARTESIAN_POINT ( 'NONE',  ( -74.09901423582336122, -282.3239683497937449, -337.6282586243166861 ) ) ;
#37879 = CARTESIAN_POINT ( 'NONE',  ( -62.31807115371835692, -278.3103704656411423, -343.0051362575957228 ) ) ;
#37880 = CARTESIAN_POINT ( 'NONE',  ( 25.50693952603189274, -277.6497980191384158, -313.7279578725210172 ) ) ;
#37881 = CIRCLE ( 'NONE', #87766, 26.04691768583011680 ) ;
#37882 = CARTESIAN_POINT ( 'NONE',  ( -53.35057174420112602, -282.3376638359844151, -200.3683826091709648 ) ) ;
#37883 = ORIENTED_EDGE ( 'NONE', *, *, #30742, .F. ) ;
#37884 = CARTESIAN_POINT ( 'NONE',  ( -112.2102538266806420, -298.6093062984550102, -265.9226144867148491 ) ) ;
#37885 = CARTESIAN_POINT ( 'NONE',  ( -92.63585976976855818, -290.9477255737501764, -318.5699222785102052 ) ) ;
#37886 = CARTESIAN_POINT ( 'NONE',  ( -98.24192166784143865, -275.9826242696316285, -313.5459242475561155 ) ) ;
#37887 = CARTESIAN_POINT ( 'NONE',  ( -65.05626370705968498, -291.1693201541895064, -341.1689339508319563 ) ) ;
#37888 = CARTESIAN_POINT ( 'NONE',  ( -34.84550506760024291, -291.4329202995482433, -197.3018155038428461 ) ) ;
#37889 = CARTESIAN_POINT ( 'NONE',  ( 31.62947258698452302, -287.4996641502236230, -304.5767688223044161 ) ) ;
#37890 = CARTESIAN_POINT ( 'NONE',  ( 207.8064396648212551, 36.74001737686529623, 13.57731244650625690 ) ) ;
#37891 = CARTESIAN_POINT ( 'NONE',  ( -105.9652657463868479, -282.5911136779089929, -297.6526102722045835 ) ) ;
#37892 = CARTESIAN_POINT ( 'NONE',  ( -109.8644192410052653, -292.2062103438839245, -286.2732203357548428 ) ) ;
#37893 = CARTESIAN_POINT ( 'NONE',  ( -110.5639283553350367, -282.9175442280081256, -279.1217415197455125 ) ) ;
#37894 = CARTESIAN_POINT ( 'NONE',  ( 26.88172111737788228, -282.3820820374240270, -234.6316393914941898 ) ) ;
#37895 = CARTESIAN_POINT ( 'NONE',  ( -112.6348559637020799, -291.3049127527841620, -285.3863339856826542 ) ) ;
#37896 = CARTESIAN_POINT ( 'NONE',  ( -108.2302647728582770, -278.8106888934681820, -288.0988227970166236 ) ) ;
#37897 = CARTESIAN_POINT ( 'NONE',  ( 22.80589254233456842, -291.7091276413913761, -222.9030792161684076 ) ) ;
#37898 = CARTESIAN_POINT ( 'NONE',  ( -23.82438203873358873, -287.0233348401827698, -194.6668090308007493 ) ) ;
#37899 = CARTESIAN_POINT ( 'NONE',  ( 28.64253936591920890, -287.5269053398747019, -230.6906288048405145 ) ) ;
#37900 = CARTESIAN_POINT ( 'NONE',  ( -94.28367814786605550, -284.0730989365664527, -316.0604412714987461 ) ) ;
#37901 = ORIENTED_EDGE ( 'NONE', *, *, #35632, .F. ) ;
#37902 = DIRECTION ( 'NONE',  ( -0.7957555401921962979, -0.6056179655966504871, 0.000000000000000000 ) ) ;
#37903 = CARTESIAN_POINT ( 'NONE',  ( -50.37750192876276856, -293.7478386542660473, -195.7261841411425962 ) ) ;
#37904 = CARTESIAN_POINT ( 'NONE',  ( -105.5258539099958028, -294.7859214051467802, -305.1797347298445402 ) ) ;
#37905 = CARTESIAN_POINT ( 'NONE',  ( 21.01718239492835494, -275.2306949174555939, -314.6064485773082993 ) ) ;
#37906 = CARTESIAN_POINT ( 'NONE',  ( -78.14134631940559927, -296.8673582020284698, -205.1790525265601275 ) ) ;
#37907 = CARTESIAN_POINT ( 'NONE',  ( 17.58453420211446527, -292.7284540843510285, -319.5107442805134497 ) ) ;
#37908 = CARTESIAN_POINT ( 'NONE',  ( -99.59764393805663474, -294.2445650762564355, -310.4821818053980564 ) ) ;
#37909 = CARTESIAN_POINT ( 'NONE',  ( -108.4971888562050992, -291.9941278445810440, -252.3092113475963743 ) ) ;
#37910 = CARTESIAN_POINT ( 'NONE',  ( 33.05082817476538537, -294.9020240355306441, -290.8786394097517132 ) ) ;
#37911 = CARTESIAN_POINT ( 'NONE',  ( -23.68628624284178130, -43.55766379199612004, 22.50000000000000000 ) ) ;
#37912 = CARTESIAN_POINT ( 'NONE',  ( -32.16482345846244328, -292.9868597415327258, -345.3622451808073492 ) ) ;
#37913 = CARTESIAN_POINT ( 'NONE',  ( -88.67267991231055646, -299.3324894279874684, -215.6086549289517222 ) ) ;
#37914 = CARTESIAN_POINT ( 'NONE',  ( 3.756531542628308795, -289.4255022940145636, -331.0386396783659393 ) ) ;
#37915 = CARTESIAN_POINT ( 'NONE',  ( 9.523272992201938791, -278.3916522198820758, -329.4369280531495292 ) ) ;
#37916 = CARTESIAN_POINT ( 'NONE',  ( -104.3535256286225206, -277.7182137153757253, -233.4461682377362024 ) ) ;
#37917 = CARTESIAN_POINT ( 'NONE',  ( -31.25984375472080856, -273.4756288010908065, -193.6906704887533692 ) ) ;
#37918 = CARTESIAN_POINT ( 'NONE',  ( 19.95993369407761975, -278.9709942436958841, -222.8246241192646551 ) ) ;
#37919 = CARTESIAN_POINT ( 'NONE',  ( -111.7081662790270116, -276.7420514374772438, -286.9764461759999676 ) ) ;
#37920 = CARTESIAN_POINT ( 'NONE',  ( -90.77723647660442907, -294.5144331977039656, -320.8912095960502029 ) ) ;
#37921 = CARTESIAN_POINT ( 'NONE',  ( -99.71146802823204780, -275.1163471905415463, -228.6157160029798945 ) ) ;
#37922 = CARTESIAN_POINT ( 'NONE',  ( -29.98784991494091656, -274.7991011438192572, -197.6300135279857955 ) ) ;
#37923 = DIRECTION ( 'NONE',  ( 3.961265963009670520E-15, 7.202301750926674102E-15, -1.000000000000000000 ) ) ;
#37924 = CARTESIAN_POINT ( 'NONE',  ( -76.29691754400595016, -289.5546316110525709, -205.7959278483178025 ) ) ;
#37925 = CARTESIAN_POINT ( 'NONE',  ( -113.8135556978273115, -290.4340524855738863, -279.8042728030280273 ) ) ;
#37926 = CARTESIAN_POINT ( 'NONE',  ( 25.38624446038517135, -276.9943808511857242, -228.9457416828620637 ) ) ;
#37927 = CARTESIAN_POINT ( 'NONE',  ( -112.2078474041528153, -294.5737924853900154, -268.6665875318754502 ) ) ;
#37928 = CARTESIAN_POINT ( 'NONE',  ( -69.12900813159500046, -282.6568709926306724, -340.3306733251769174 ) ) ;
#37929 = CYLINDRICAL_SURFACE ( 'NONE', #15405, 6.000000000000005329 ) ;
#37930 = CARTESIAN_POINT ( 'NONE',  ( 18.51668205331070283, -280.2492099564546493, -320.4285477096707950 ) ) ;
#37931 = DIRECTION ( 'NONE',  ( 0.000000000000000000, 1.000000000000000000, 0.000000000000000000 ) ) ;
#37932 = CARTESIAN_POINT ( 'NONE',  ( -60.36906169767474495, -290.5418558152254036, -200.6165381951582845 ) ) ;
#37933 = CARTESIAN_POINT ( 'NONE',  ( -108.5328522624296141, -282.9675988319892781, -249.1429434439755539 ) ) ;
#37934 = DIRECTION ( 'NONE',  ( 1.000000000000000000, 0.000000000000000000, 1.224646799147353207E-16 ) ) ;
#37935 = FACE_OUTER_BOUND ( 'NONE', #55830, .T. ) ;
#37936 = CARTESIAN_POINT ( 'NONE',  ( 35.37921285071867317, -291.7876982231325087, -288.7096729066396392 ) ) ;
#37937 = CARTESIAN_POINT ( 'NONE',  ( -101.2657006484102027, -279.6508405594983628, -307.3440872695285861 ) ) ;
#37938 = CARTESIAN_POINT ( 'NONE',  ( -44.36743251959935463, -284.3440870560242502, -346.6942614041393540 ) ) ;
#37940 = CARTESIAN_POINT ( 'NONE',  ( -72.37401242321359973, -285.5748606903512155, -206.3020960892154676 ) ) ;
#37939 = CARTESIAN_POINT ( 'NONE',  ( -35.53327204678248563, -272.1544973493340080, -194.8098739069588134 ) ) ;
#37941 = CARTESIAN_POINT ( 'NONE',  ( 7.957272456310147568, -277.8448265606603513, -328.4206999836026739 ) ) ;
#37942 = CARTESIAN_POINT ( 'NONE',  ( 17.56316655420695128, -277.0440886599989199, -318.7334835776064779 ) ) ;
#37943 = CARTESIAN_POINT ( 'NONE',  ( -82.65407103244992015, -285.6710795554912465, -330.1907914476502697 ) ) ;
#37944 = ORIENTED_EDGE ( 'NONE', *, *, #11892, .F. ) ;
#37945 = CARTESIAN_POINT ( 'NONE',  ( 123.4306832106270946, -134.2391364535880882, 4.999999999999990230 ) ) ;
#37946 = CARTESIAN_POINT ( 'NONE',  ( -37.69110860217527659, -294.8896991948645336, -347.3734036179122313 ) ) ;
#37948 = CARTESIAN_POINT ( 'NONE',  ( -38.67910699160877641, -288.0152243189778005, -195.7155332092584672 ) ) ;
#37947 = VECTOR ( 'NONE', #34048, 1000.000000000000000 ) ;
#37949 = CYLINDRICAL_SURFACE ( 'NONE', #91098, 5.000000000000000888 ) ;
#37950 = CARTESIAN_POINT ( 'NONE',  ( 35.65787339142939771, -296.4086741954485547, -190.3901485728259217 ) ) ;
#37951 = CARTESIAN_POINT ( 'NONE',  ( -112.9964973706912872, -277.3147261177873588, -282.9247227295463745 ) ) ;
#37952 = ADVANCED_FACE ( 'NONE', ( #46328, #16997 ), #23164, .F. ) ;
#37953 = CARTESIAN_POINT ( 'NONE',  ( -6.195093308072523008, -290.8544599722134762, -200.8032537155962132 ) ) ;
#37954 = CARTESIAN_POINT ( 'NONE',  ( -77.44243007871132534, -287.0239615608816734, -208.4730675298639540 ) ) ;
#37955 = CARTESIAN_POINT ( 'NONE',  ( -110.9766454386635530, -280.4159613647066180, -262.3939060166317745 ) ) ;
#37956 = CARTESIAN_POINT ( 'NONE',  ( 28.18384245165263025, -288.4596801626459524, -230.9525018236989808 ) ) ;
#37957 = CARTESIAN_POINT ( 'NONE',  ( 35.03716794658999589, -283.2990262911592936, -250.6575272160768577 ) ) ;
#37958 = CARTESIAN_POINT ( 'NONE',  ( -2.723208958902804788, -276.7739047820277278, -339.1548632472157578 ) ) ;
#37959 = CARTESIAN_POINT ( 'NONE',  ( -93.97625537493581760, -295.2494424698325588, -221.7166372947169179 ) ) ;
#37960 = CARTESIAN_POINT ( 'NONE',  ( -91.05664768868534509, -279.1481685183265995, -215.1170099280971044 ) ) ;
#37961 = CARTESIAN_POINT ( 'NONE',  ( -95.59315608801429676, -299.1141109904908717, -224.0137115754118042 ) ) ;
#37962 = CARTESIAN_POINT ( 'NONE',  ( 159.0442047513580235, 16.65459343288188521, 10.27557066714185119 ) ) ;
#37963 = CARTESIAN_POINT ( 'NONE',  ( -69.91165696735023971, -282.1233781216988064, -202.8022627189028810 ) ) ;
#37964 = CARTESIAN_POINT ( 'NONE',  ( -70.93438238202305968, -271.8548706035268197, -202.2031711506399176 ) ) ;
#37965 = CARTESIAN_POINT ( 'NONE',  ( 157.4851178187871312, 15.00000000000000000, 7.000000000000000888 ) ) ;
#37966 = CARTESIAN_POINT ( 'NONE',  ( -108.8262838897055644, -277.8608066030098485, -285.4588902117479847 ) ) ;
#37967 = CARTESIAN_POINT ( 'NONE',  ( -52.48223583661943792, -275.0675880126790958, -195.2151923003513616 ) ) ;
#37968 = CARTESIAN_POINT ( 'NONE',  ( 37.45097726468010535, -280.3933772174981414, -253.0153047186524020 ) ) ;
#37969 = CARTESIAN_POINT ( 'NONE',  ( -78.72266164990936943, -291.3777989225558827, -331.7872096583340635 ) ) ;
#37970 = CARTESIAN_POINT ( 'NONE',  ( -31.98970937299928963, -299.6381229907490820, -194.0530915948497750 ) ) ;
#37971 = CARTESIAN_POINT ( 'NONE',  ( -93.38279730261572809, -298.4735073980250490, -218.0591730620326985 ) ) ;
#37972 = CARTESIAN_POINT ( 'NONE',  ( 26.39635497366114336, -295.0238672210218738, -231.0519721495477086 ) ) ;
#37973 = CARTESIAN_POINT ( 'NONE',  ( -2.797170243721856853, -280.5943139258583869, -336.7584817938143260 ) ) ;
#37974 = CARTESIAN_POINT ( 'NONE',  ( 32.41123328122457536, -283.1305321615582784, -244.2163960166066659 ) ) ;
#37975 = CARTESIAN_POINT ( 'NONE',  ( -33.94107478962236968, -272.1152532615171822, -195.7938158184799420 ) ) ;
#37976 = CARTESIAN_POINT ( 'NONE',  ( -98.71218438183289834, -286.7596084585323410, -225.1067590509952367 ) ) ;
#37977 = CARTESIAN_POINT ( 'NONE',  ( -84.89595159269639169, -288.6462206336403256, -326.2207769746805184 ) ) ;
#37978 = CARTESIAN_POINT ( 'NONE',  ( 169.3780306774251585, 231.6620261969012518, -192.5545122492718235 ) ) ;
#37979 = ORIENTED_EDGE ( 'NONE', *, *, #4151, .T. ) ;
#37980 = CARTESIAN_POINT ( 'NONE',  ( -41.74488444491926487, -287.6813047203755218, -346.6580397196959780 ) ) ;
#37981 = CARTESIAN_POINT ( 'NONE',  ( -0.9845994714391579361, -288.2223261237656970, -333.7458427672590915 ) ) ;
#37982 = VERTEX_POINT ( 'NONE', #8490 ) ;
#37983 = CARTESIAN_POINT ( 'NONE',  ( -21.06303720827952120, -287.3359878590978838, -195.4178218019410451 ) ) ;
#37984 = CARTESIAN_POINT ( 'NONE',  ( 35.66395734434348697, -275.8656034421017011, -268.8573016045793338 ) ) ;
#37985 = CARTESIAN_POINT ( 'NONE',  ( -84.06708826913678934, -290.3475395861378843, -209.4811169698811284 ) ) ;
#37986 = CARTESIAN_POINT ( 'NONE',  ( 39.08050112270579746, -282.0907634891744920, -261.3536578646687758 ) ) ;
#37987 = CARTESIAN_POINT ( 'NONE',  ( 19.59830107522506637, -282.3770738116945154, -219.5424215642073307 ) ) ;
#37988 = CARTESIAN_POINT ( 'NONE',  ( -55.69302733148930429, -283.6154267302645167, -345.1205527136312412 ) ) ;
#37989 = CARTESIAN_POINT ( 'NONE',  ( -1.966078159314026408, -280.5346557561970826, -206.5053009388257692 ) ) ;
#37990 = CARTESIAN_POINT ( 'NONE',  ( -67.68488546085839630, -295.1237833571632336, -207.2794874003663779 ) ) ;
#37991 = CARTESIAN_POINT ( 'NONE',  ( 202.4862527844790918, 293.5851137920426481, -83.23994149847183621 ) ) ;
#37992 = ORIENTED_EDGE ( 'NONE', *, *, #55196, .T. ) ;
#37993 = B_SPLINE_CURVE_WITH_KNOTS ( 'NONE', 3,
 ( #89995, #75341, #33651, #10457 ),
 .UNSPECIFIED., .F., .F.,
 ( 4, 4 ),
 ( 2.907926436840383405E-17, 9.632970524407232079E-05 ),
 .UNSPECIFIED. ) ;
#37994 = CARTESIAN_POINT ( 'NONE',  ( 34.27822788303749491, -277.8330348413301749, -292.0992371250971473 ) ) ;
#37995 = CARTESIAN_POINT ( 'NONE',  ( -78.78026294810004515, -207.9127932031447585, -356.5521822105918659 ) ) ;
#37996 = CARTESIAN_POINT ( 'NONE',  ( -63.10763767576398209, -297.0562292587401316, -201.8969743661794496 ) ) ;
#37997 = CARTESIAN_POINT ( 'NONE',  ( 39.38017149039897902, -292.9875991775623447, -264.5921216702219567 ) ) ;
#37998 = CARTESIAN_POINT ( 'NONE',  ( 185.4443931024105154, 260.3151622445499243, -151.1883627937757524 ) ) ;
#38000 = CARTESIAN_POINT ( 'NONE',  ( -111.1372252583517053, -288.9414081907249852, -271.1740655560380446 ) ) ;
#37999 = CARTESIAN_POINT ( 'NONE',  ( -51.67217270728417589, -296.4471537263942764, -195.2522580918571578 ) ) ;
#38001 = CARTESIAN_POINT ( 'NONE',  ( -107.1406086838903917, -298.0796573429769865, -295.7901449906062226 ) ) ;
#38002 = CARTESIAN_POINT ( 'NONE',  ( 32.73882718537697656, -288.5753709002102028, -248.1839057564806694 ) ) ;
#38003 = EDGE_LOOP ( 'NONE', ( #42815, #69715, #79264, #75142, #84567, #32330 ) ) ;
#38004 = CARTESIAN_POINT ( 'NONE',  ( -37.67588714652610093, -295.9974518625468818, -347.1381360191537055 ) ) ;
#38005 = CARTESIAN_POINT ( 'NONE',  ( -110.3710226115697708, -285.0730970311594774, -268.1916712630496704 ) ) ;
#38006 = CARTESIAN_POINT ( 'NONE',  ( -99.58988748450602202, -295.9417837305581997, -225.7161642925951810 ) ) ;
#38007 = CARTESIAN_POINT ( 'NONE',  ( -84.17603890807394862, -292.2297406332108949, -209.3785076887394894 ) ) ;
#38008 = CARTESIAN_POINT ( 'NONE',  ( 8.808999987652043728, -293.1580491083669244, -208.7345788021393957 ) ) ;
#38009 = CARTESIAN_POINT ( 'NONE',  ( -101.1247101860493416, -291.2055745553146835, -234.7505614426116551 ) ) ;
#38010 = ORIENTED_EDGE ( 'NONE', *, *, #22499, .F. ) ;
#38011 = CARTESIAN_POINT ( 'NONE',  ( 159.4851178187871312, 14.99999999999999467, 9.000000000000001776 ) ) ;
#38012 = CARTESIAN_POINT ( 'NONE',  ( -105.4140822479478317, -298.8466545130112308, -237.0976805429417311 ) ) ;
#38013 = CARTESIAN_POINT ( 'NONE',  ( -13.17314441254772284, -273.1542339601764411, -197.6707497586970419 ) ) ;
#38014 = EDGE_LOOP ( 'NONE', ( #63002, #21449, #51278, #67111 ) ) ;
#38015 = EDGE_LOOP ( 'NONE', ( #3085, #63888, #10385, #57156, #32848, #82813 ) ) ;
#38016 = CARTESIAN_POINT ( 'NONE',  ( 8.199586888363507242, -275.9557434701049488, -332.4393170127128769 ) ) ;
#38017 = CARTESIAN_POINT ( 'NONE',  ( -85.82050341148772077, -271.7678419455719450, -214.6491010855486934 ) ) ;
#38018 = CARTESIAN_POINT ( 'NONE',  ( -106.6763083332015327, -280.7625981916240221, -243.6919817331335025 ) ) ;
#38019 = CARTESIAN_POINT ( 'NONE',  ( -10.83475279343434217, -274.8423747250193969, -339.7026439493652674 ) ) ;
#38020 = CARTESIAN_POINT ( 'NONE',  ( -82.19885496673704495, -298.6300005771332735, -212.2022350942222033 ) ) ;
#38021 = CARTESIAN_POINT ( 'NONE',  ( -102.2445098675298283, -273.9549306473553543, -236.3243581427655045 ) ) ;
#38022 = CARTESIAN_POINT ( 'NONE',  ( -26.37381662821301376, -299.7874194203834008, -194.1581838898675301 ) ) ;
#38023 = AXIS2_PLACEMENT_3D ( 'NONE', #51796, #73600, #2094 ) ;
#38024 = CARTESIAN_POINT ( 'NONE',  ( 18.82708103143630751, -272.8754507414665227, -220.0502045523545860 ) ) ;
#38025 = CARTESIAN_POINT ( 'NONE',  ( -104.0262027689579583, -296.7991953022923894, -300.4359476478604165 ) ) ;
#38026 = CARTESIAN_POINT ( 'NONE',  ( -64.27046450102136532, -290.2684964245506194, -201.8623214280431455 ) ) ;
#38027 = CARTESIAN_POINT ( 'NONE',  ( 193.8285826777556906, 214.7033826592484900, 16.75079304138583325 ) ) ;
#38028 = CARTESIAN_POINT ( 'NONE',  ( -20.13376311645589212, -277.3292412974519721, -345.4052188263205494 ) ) ;
#38029 = CARTESIAN_POINT ( 'NONE',  ( 13.49513530746693846, -274.9551107504381093, -217.9720335527587451 ) ) ;
#38030 = CIRCLE ( 'NONE', #90927, 5.000000000000000888 ) ;
#38031 = CARTESIAN_POINT ( 'NONE',  ( -110.6403524020426801, -282.9595852846330217, -292.3293688976641533 ) ) ;
#38032 = CARTESIAN_POINT ( 'NONE',  ( -112.4014047878844167, -298.4897306950653615, -275.2462256535673077 ) ) ;
#38033 = CARTESIAN_POINT ( 'NONE',  ( 17.06571399127465583, -89.54582641780471874, 21.50000000000000000 ) ) ;
#38034 = EDGE_CURVE ( 'NONE', #74706, #29017, #17244, .T. ) ;
#38035 = CARTESIAN_POINT ( 'NONE',  ( -46.73549448923062499, -285.1271442305770165, -197.7543325333487871 ) ) ;
#38036 = CARTESIAN_POINT ( 'NONE',  ( -47.04552479385017705, -281.1749854343948982, -344.8987877324399847 ) ) ;
#38037 = CARTESIAN_POINT ( 'NONE',  ( -108.0918309486891928, -276.5060405219413155, -292.2675135468204530 ) ) ;
#38038 = CARTESIAN_POINT ( 'NONE',  ( -51.41117104690651729, -275.8103227967047815, -342.5928624138286409 ) ) ;
#38039 = CARTESIAN_POINT ( 'NONE',  ( 12.97923336959364171, -282.7545632186796638, -214.6792131050404748 ) ) ;
#38040 = CARTESIAN_POINT ( 'NONE',  ( -6.375337126376237507, -275.6733370884547298, -203.8162844600482231 ) ) ;
#38041 = CARTESIAN_POINT ( 'NONE',  ( 156.4851178187871312, 15.00000000000000000, -10.00000000000000000 ) ) ;
#38042 = CARTESIAN_POINT ( 'NONE',  ( -109.3392502214157815, -271.2699654632976944, -245.4052931082674718 ) ) ;
#38043 = CARTESIAN_POINT ( 'NONE',  ( -2.020010472000925983, -282.5189682774783364, -204.0104837070591657 ) ) ;
#38044 = DIRECTION ( 'NONE',  ( -1.110223024625156383E-14, 0.000000000000000000, 1.000000000000000000 ) ) ;
#38045 = CARTESIAN_POINT ( 'NONE',  ( 28.85793303929712295, -288.9902804529170339, -233.8256666176858118 ) ) ;
#38046 = SURFACE_STYLE_USAGE ( .BOTH. , #16297 ) ;
#38047 = CARTESIAN_POINT ( 'NONE',  ( -77.36554666504912348, -287.5883757774195715, -333.8490403940427882 ) ) ;
#38048 = CARTESIAN_POINT ( 'NONE',  ( 199.2296996224750103, 68.12454877777268791, 0.000000000000000000 ) ) ;
#38049 = CARTESIAN_POINT ( 'NONE',  ( 52.29403391987453631, -297.9936773689175311, -196.9829468324793709 ) ) ;
#38050 = CARTESIAN_POINT ( 'NONE',  ( -107.2028677025591747, -288.3629464893806471, -295.4665505462839974 ) ) ;
#38051 = CARTESIAN_POINT ( 'NONE',  ( 197.9737475143014365, 296.4634315385704895, -68.42128063630356394 ) ) ;
#38052 = CARTESIAN_POINT ( 'NONE',  ( -39.19284143790798680, -296.0287923942119050, -195.3712127120207356 ) ) ;
#38053 = CARTESIAN_POINT ( 'NONE',  ( 36.11169830780685430, -286.2939863111757859, -291.0803737606623258 ) ) ;
#38054 = CARTESIAN_POINT ( 'NONE',  ( -21.19353604100142974, -284.4418195411456054, -342.4253500997595552 ) ) ;
#38055 = CARTESIAN_POINT ( 'NONE',  ( -60.18366881432676507, -284.0000331656657977, -197.8340883321860701 ) ) ;
#38056 = CARTESIAN_POINT ( 'NONE',  ( -67.80119068360822610, -291.6409105054428892, -204.0056966741539384 ) ) ;
#38057 = CARTESIAN_POINT ( 'NONE',  ( 20.97180445537994942, -282.3504855144262820, -225.4528947625408648 ) ) ;
#38058 = CARTESIAN_POINT ( 'NONE',  ( 33.26674139174349421, -282.1018918807884006, -251.1546712788251909 ) ) ;
#38059 = ADVANCED_FACE ( 'NONE', ( #16077, #3250 ), #31221, .F. ) ;
#38060 = CARTESIAN_POINT ( 'NONE',  ( -110.6564373829958754, -292.3087541750309697, -287.8333740428198553 ) ) ;
#38061 = CARTESIAN_POINT ( 'NONE',  ( -33.33661474827648163, -298.2676784322164849, -193.3610081594396206 ) ) ;
#38062 = ORIENTED_EDGE ( 'NONE', *, *, #56630, .F. ) ;
#38063 = CARTESIAN_POINT ( 'NONE',  ( 26.21996961618841482, -286.1793335361921322, -311.3137351565780477 ) ) ;
#38064 = CARTESIAN_POINT ( 'NONE',  ( 19.87720214335996971, -276.2517535795547019, -321.9075151797589456 ) ) ;
#38065 = CARTESIAN_POINT ( 'NONE',  ( -73.44409134452433818, -293.5510314178607132, -204.9695415175167170 ) ) ;
#38066 = CARTESIAN_POINT ( 'NONE',  ( 198.1425780972542157, 15.00000000000000000, -10.00000000000000000 ) ) ;
#38067 = CARTESIAN_POINT ( 'NONE',  ( -85.28047601435908120, -280.1948066931273047, -330.5268031993605859 ) ) ;
#38068 = CARTESIAN_POINT ( 'NONE',  ( -72.01812765988987053, -275.5093619164914571, -337.0656063798820696 ) ) ;
#38069 = CARTESIAN_POINT ( 'NONE',  ( 208.3435665664548253, 37.37777598216731434, 12.00000000000000000 ) ) ;
#38070 = CARTESIAN_POINT ( 'NONE',  ( -43.20762621294778683, -296.3792661677754836, -194.3345750951777973 ) ) ;
#38071 = CARTESIAN_POINT ( 'NONE',  ( -94.68751698953826690, -272.5396184233964618, -225.0251503953136023 ) ) ;
#38072 = CARTESIAN_POINT ( 'NONE',  ( -103.0363452464017939, -292.5228295113558943, -236.8576611911791190 ) ) ;
#38073 = CARTESIAN_POINT ( 'NONE',  ( -104.9248197460980521, -291.8721990889911808, -242.0168600270522177 ) ) ;
#38074 = CARTESIAN_POINT ( 'NONE',  ( -109.4068923262737769, -286.0921486355181287, -287.2859794326822112 ) ) ;
#38075 = CARTESIAN_POINT ( 'NONE',  ( 1.385683880272469359, -293.9838099719196407, -204.4311199512791575 ) ) ;
#38076 = CARTESIAN_POINT ( 'NONE',  ( 15.08794424837540582, -294.0883033630243517, -214.5709747507284817 ) ) ;
#38077 = CARTESIAN_POINT ( 'NONE',  ( 35.42426483371428958, -293.4625202886259103, -276.2018668788093123 ) ) ;
#38078 = CARTESIAN_POINT ( 'NONE',  ( 25.93914211147642490, -290.0940410217154408, -310.6169952348456036 ) ) ;
#38079 = CARTESIAN_POINT ( 'NONE',  ( 36.59912542331345975, -281.4488246690619349, -248.8253842194818048 ) ) ;
#38080 = CARTESIAN_POINT ( 'NONE',  ( -54.24873108733295624, -295.9164900576541299, -196.7169294862655420 ) ) ;
#38081 = CARTESIAN_POINT ( 'NONE',  ( -78.52067087794172551, -285.3473135554751252, -205.2973617700632758 ) ) ;
#38082 = CARTESIAN_POINT ( 'NONE',  ( 22.79159058339396182, -276.9260289539328710, -226.1363042096109552 ) ) ;
#38083 = EDGE_CURVE ( 'NONE', #63583, #26188, #44930, .T. ) ;
#38084 = CARTESIAN_POINT ( 'NONE',  ( -108.4093102378187439, -283.5879308475414291, -252.0164920896237390 ) ) ;
#38085 = CARTESIAN_POINT ( 'NONE',  ( 28.59199460058563247, -286.0280141179491693, -306.2152749690803262 ) ) ;
#38086 = CARTESIAN_POINT ( 'NONE',  ( -113.1415284369289225, -276.7123818836934106, -268.7367008472911607 ) ) ;
#38088 = AXIS2_PLACEMENT_3D ( 'NONE', #54573, #83444, #62655 ) ;
#38087 = CARTESIAN_POINT ( 'NONE',  ( 175.2296996224750103, 161.0000000000000853, -9.550761578869391144 ) ) ;
#38089 = CARTESIAN_POINT ( 'NONE',  ( -68.79575240390201429, -285.1347820164560289, -204.4031666728032519 ) ) ;
#38090 = AXIS2_PLACEMENT_3D ( 'NONE', #15253, #22811, #9051 ) ;
#38091 = CARTESIAN_POINT ( 'NONE',  ( -11.65702282940276113, -281.5842657776760802, -198.1368346254730284 ) ) ;
#38092 = CARTESIAN_POINT ( 'NONE',  ( 19.44209849457770289, -287.3153057858571060, -322.0374496882692483 ) ) ;
#38093 = CARTESIAN_POINT ( 'NONE',  ( 4.406193145682850698, -296.2405483440600733, -331.4764795447555343 ) ) ;
#38094 = CARTESIAN_POINT ( 'NONE',  ( -71.19691223855207340, -279.0917383025974914, -338.6272518357770309 ) ) ;
#38095 = CARTESIAN_POINT ( 'NONE',  ( -56.78244293940348086, -278.6127705720674044, -344.4114615685963940 ) ) ;
#38096 = CARTESIAN_POINT ( 'NONE',  ( -61.79182492101748636, -277.2121412433758678, -339.1985157613461865 ) ) ;
#38097 = CARTESIAN_POINT ( 'NONE',  ( -94.15242387558603809, -299.2288517715467719, -221.6323644550944607 ) ) ;
#38098 = CARTESIAN_POINT ( 'NONE',  ( 36.81639763142910482, -285.4180333055808205, -259.9514766968874255 ) ) ;
#38099 = TOROIDAL_SURFACE ( 'NONE', #72932, 1.000000000000000000, 0.5000000000000000000 ) ;
#38100 = CARTESIAN_POINT ( 'NONE',  ( -110.8663202425512395, -292.4061405809321741, -250.2972950319428662 ) ) ;
#38101 = CARTESIAN_POINT ( 'NONE',  ( -34.30208204216661017, -293.9333656212720598, -343.6071881580551235 ) ) ;
#38102 = ORIENTED_EDGE ( 'NONE', *, *, #60850, .T. ) ;
#38103 = CARTESIAN_POINT ( 'NONE',  ( -20.84752390307642500, -294.5014145718042755, -341.5471223093775279 ) ) ;
#38104 = CARTESIAN_POINT ( 'NONE',  ( -66.90902328005806510, -292.7532913219158104, -199.5990807605870430 ) ) ;
#38105 = CARTESIAN_POINT ( 'NONE',  ( -89.55218366008271857, -279.9438174470339504, -219.1233851949293410 ) ) ;
#38106 = CARTESIAN_POINT ( 'NONE',  ( -34.75850841673518943, -297.0041160269089460, -193.6706883115846551 ) ) ;
#38107 = CARTESIAN_POINT ( 'NONE',  ( 37.72725014170847402, -288.4131013318003056, -287.0935583328578673 ) ) ;
#38108 = CARTESIAN_POINT ( 'NONE',  ( 22.39142333219114178, -288.5372376295240997, -318.9379997211000273 ) ) ;
#38109 = CARTESIAN_POINT ( 'NONE',  ( -5.793356887292062218, -286.8119764390199862, -204.4930250025599321 ) ) ;
#38110 = CARTESIAN_POINT ( 'NONE',  ( 202.9737692553709962, 295.9636489462768054, -68.65455572930012806 ) ) ;
#38111 = CARTESIAN_POINT ( 'NONE',  ( 166.2108551876890488, 232.3202090705826492, -191.5262553198002138 ) ) ;
#38112 = CARTESIAN_POINT ( 'NONE',  ( 167.1921940846895893, 229.9663351943898419, -189.8569236648036451 ) ) ;
#38113 = CARTESIAN_POINT ( 'NONE',  ( -91.09342159657846594, -277.0374043253031004, -320.0670094650786268 ) ) ;
#38114 = CARTESIAN_POINT ( 'NONE',  ( -51.35337332025960677, -276.1558680671116690, -342.3187380588741462 ) ) ;
#38115 = CARTESIAN_POINT ( 'NONE',  ( -92.15102994253193458, -272.9615447619819406, -216.3085356503619039 ) ) ;
#38116 = CARTESIAN_POINT ( 'NONE',  ( -20.35789830974468018, -109.6084772789823916, -359.8065553577603737 ) ) ;
#38117 = CARTESIAN_POINT ( 'NONE',  ( -110.9705065649931299, -276.9747855222266821, -291.1480642736794948 ) ) ;
#38118 = CARTESIAN_POINT ( 'NONE',  ( 12.74495500033551387, -296.1252341224343354, -327.5737134146771723 ) ) ;
#38119 = CARTESIAN_POINT ( 'NONE',  ( -109.6829969018154856, -290.9084358417952672, -280.6843532465209705 ) ) ;
#38120 = CARTESIAN_POINT ( 'NONE',  ( -112.4448545765557412, -297.5592081711904484, -254.0615937859901408 ) ) ;
#38121 = CARTESIAN_POINT ( 'NONE',  ( -101.1286437139368957, -273.7711920057724342, -227.3182133880806362 ) ) ;
#38122 = CARTESIAN_POINT ( 'NONE',  ( -88.12726814782543272, -297.4840736525333114, -217.8517575210165660 ) ) ;
#38123 = EDGE_LOOP ( 'NONE', ( #16201, #12681, #38915, #36614 ) ) ;
#38124 = CARTESIAN_POINT ( 'NONE',  ( 155.7140808774800007, 20.99999999999998934, -15.62500000000000711 ) ) ;
#38125 = CARTESIAN_POINT ( 'NONE',  ( -14.99185207823118304, -278.6851731866643718, -342.5948391728875890 ) ) ;
#38126 = CARTESIAN_POINT ( 'NONE',  ( 23.35050395498058862, -281.6922609910706683, -317.6685906046086529 ) ) ;
#38127 = CARTESIAN_POINT ( 'NONE',  ( -87.75312529491488078, -280.4077368875006186, -217.0658230868243095 ) ) ;
#38128 = CARTESIAN_POINT ( 'NONE',  ( -68.57805882759940630, -279.2171287941487208, -339.6448327876481699 ) ) ;
#38129 = CARTESIAN_POINT ( 'NONE',  ( -90.68525089149083840, -271.7585826991801810, -219.4980614582265730 ) ) ;
#38130 = CARTESIAN_POINT ( 'NONE',  ( 222.2216768131362130, 37.54180348216212337, -7.000000000000000888 ) ) ;
#38131 = CARTESIAN_POINT ( 'NONE',  ( -67.30822923370951116, -279.8145885708273113, -203.7817009153541221 ) ) ;
#38132 = CARTESIAN_POINT ( 'NONE',  ( 20.70499276958092238, -277.0369178684688904, -320.7272392672297769 ) ) ;
#38133 = CARTESIAN_POINT ( 'NONE',  ( 37.38987542344903403, -277.6337173131076952, -276.7008547578741968 ) ) ;
#38134 = CARTESIAN_POINT ( 'NONE',  ( 18.46040732272641449, -274.8443577663598489, -322.5600748390428407 ) ) ;
#38135 = ORIENTED_EDGE ( 'NONE', *, *, #85924, .T. ) ;
#38136 = CARTESIAN_POINT ( 'NONE',  ( 164.2231345125756263, 275.0000000000000568, 20.22542485937379908 ) ) ;
#38137 = CARTESIAN_POINT ( 'NONE',  ( 36.37035322322167019, -283.3312483454838571, -254.6489238649541278 ) ) ;
#38138 = CARTESIAN_POINT ( 'NONE',  ( -57.69006915872256513, -290.9798938200905241, -200.0333399804792123 ) ) ;
#38139 = CARTESIAN_POINT ( 'NONE',  ( -1.010383528823081134, -285.8701362197173808, -202.5868734572287337 ) ) ;
#38140 = CARTESIAN_POINT ( 'NONE',  ( -45.77691269678831532, -281.4002506599366598, -343.9439112152375060 ) ) ;
#38142 = CARTESIAN_POINT ( 'NONE',  ( 21.49353193450845723, -285.0021332209296361, -224.7570647683890286 ) ) ;
#38141 = CARTESIAN_POINT ( 'NONE',  ( -68.04663588475162328, -282.0381534561762464, -337.2384821573598970 ) ) ;
#38143 = CARTESIAN_POINT ( 'NONE',  ( 22.42797515750187642, -282.1653427034317474, -227.7616294682023863 ) ) ;
#38144 = CARTESIAN_POINT ( 'NONE',  ( 24.96937362042031694, -22.70870612819967249, -344.9910381422254773 ) ) ;
#38145 = AXIS2_PLACEMENT_3D ( 'NONE', #54683, #13042, #19644 ) ;
#38146 = CARTESIAN_POINT ( 'NONE',  ( -10.99793381436519546, -281.1143937487111089, -341.9185428627089891 ) ) ;
#38147 = CARTESIAN_POINT ( 'NONE',  ( -5.332377254942230138, -296.6311619307271030, -338.2014921125468732 ) ) ;
#38148 = CARTESIAN_POINT ( 'NONE',  ( -113.0712592572288884, -276.7051254908457167, -277.2170487885584294 ) ) ;
#38149 = AXIS2_PLACEMENT_3D ( 'NONE', #75129, #54267, #24936 ) ;
#38150 = CARTESIAN_POINT ( 'NONE',  ( -83.06406019369541127, -278.3483213075222693, -327.4644804750734579 ) ) ;
#38151 = CARTESIAN_POINT ( 'NONE',  ( -57.29440101855271905, -287.7955695959546460, -197.8369601348519495 ) ) ;
#38152 = CIRCLE ( 'NONE', #18499, 24.00000000000001066 ) ;
#38153 = CARTESIAN_POINT ( 'NONE',  ( 0.000000000000000000, 3.000000000000000000, 7.000000000000000000 ) ) ;
#38154 = CARTESIAN_POINT ( 'NONE',  ( -104.7311097971390979, -292.9219864565461648, -236.0699337834114147 ) ) ;
#38155 = AXIS2_PLACEMENT_3D ( 'NONE', #76371, #12432, #92419 ) ;
#38156 = CARTESIAN_POINT ( 'NONE',  ( 15.11238893981135689, -274.3122857521174751, -324.0391033689166420 ) ) ;
#38157 = CARTESIAN_POINT ( 'NONE',  ( -69.29948947087444822, -288.6591707814179131, -340.2529659736412668 ) ) ;
#38158 = CARTESIAN_POINT ( 'NONE',  ( 34.73549648865058970, -291.7443981673570761, -254.4495949386498808 ) ) ;
#38159 = CARTESIAN_POINT ( 'NONE',  ( -43.21050586802018501, -280.7973836945827770, -430.6442049081568939 ) ) ;
#38160 = CARTESIAN_POINT ( 'NONE',  ( -109.0845264429125621, -277.4465791657704585, -254.3595933732700303 ) ) ;
#38161 = CARTESIAN_POINT ( 'NONE',  ( -109.5052595901155854, -294.4651296394792439, -287.8299060026484995 ) ) ;
#38162 = CARTESIAN_POINT ( 'NONE',  ( -109.6612311643044961, -291.6959195703931869, -283.4427428661520594 ) ) ;
#38163 = DIRECTION ( 'NONE',  ( 0.000000000000000000, 0.000000000000000000, 1.000000000000000000 ) ) ;
#38164 = FACE_OUTER_BOUND ( 'NONE', #38003, .T. ) ;
#38165 = CARTESIAN_POINT ( 'NONE',  ( 33.79805615685317122, -292.3849048071350012, -297.9626184323128655 ) ) ;
#38166 = CARTESIAN_POINT ( 'NONE',  ( 17.47128430420026390, -288.4521454873818698, -220.9258929091162429 ) ) ;
#38167 = CARTESIAN_POINT ( 'NONE',  ( -107.4237895048374156, -289.1705503211960604, -240.9931973861614551 ) ) ;
#38168 = CARTESIAN_POINT ( 'NONE',  ( 19.10212196162155251, -288.3123591753166579, -223.1242302544103211 ) ) ;
#38169 = DIRECTION ( 'NONE',  ( 0.000000000000000000, 0.000000000000000000, 1.000000000000000000 ) ) ;
#38170 = CARTESIAN_POINT ( 'NONE',  ( 35.28574378847898174, -288.4711299979107366, -279.1847293194409758 ) ) ;
#38171 = EDGE_CURVE ( 'NONE', #3443, #77260, #38294, .T. ) ;
#38172 = CARTESIAN_POINT ( 'NONE',  ( -93.41051579411129069, -297.8338025801376148, -320.7260867572086909 ) ) ;
#38173 = CARTESIAN_POINT ( 'NONE',  ( 197.3748232817349049, 250.5000000000000568, -12.45182892472559821 ) ) ;
#38174 = CARTESIAN_POINT ( 'NONE',  ( 32.50912416915949876, -289.1609698821554275, -301.8074383155118312 ) ) ;
#38175 = CARTESIAN_POINT ( 'NONE',  ( -40.90484585850677490, -278.0276661291882192, -195.0772881908005729 ) ) ;
#38176 = CARTESIAN_POINT ( 'NONE',  ( -42.80043329190615964, -277.4525471246775510, -347.1461850449549615 ) ) ;
#38177 = CARTESIAN_POINT ( 'NONE',  ( -35.33232595634194695, -279.7434158215249340, -193.3953584454684744 ) ) ;
#38178 = CARTESIAN_POINT ( 'NONE',  ( -109.0462468928235324, -298.8003620417125035, -249.6173290969251468 ) ) ;
#38179 = CARTESIAN_POINT ( 'NONE',  ( -27.55091640495669481, -284.1763831366105251, -196.0029227304790993 ) ) ;
#38180 = CARTESIAN_POINT ( 'NONE',  ( -110.3351356391935383, -272.5060871493917602, -270.3605314645446924 ) ) ;
#38181 = CARTESIAN_POINT ( 'NONE',  ( -52.04928822564251334, -278.0016273279152301, -197.5448404869050876 ) ) ;
#38182 = CARTESIAN_POINT ( 'NONE',  ( -67.11153899471445072, -281.4422543931092946, -339.1997506313520603 ) ) ;
#38183 = CARTESIAN_POINT ( 'NONE',  ( -23.68628624284178130, -43.55766379199612004, -21.50000000000000000 ) ) ;
#38184 = CARTESIAN_POINT ( 'NONE',  ( -37.14833585774874081, -275.5296226693956214, -346.6804828658507063 ) ) ;
#38185 = CARTESIAN_POINT ( 'NONE',  ( -61.21968729243319984, -296.8878875091681948, -340.1328370557582161 ) ) ;
#38186 = AXIS2_PLACEMENT_3D ( 'NONE', #66405, #45998, #10474 ) ;
#38187 = CARTESIAN_POINT ( 'NONE',  ( -61.14882776215457483, -282.2743603966768546, -343.3186621254529314 ) ) ;
#38188 = CARTESIAN_POINT ( 'NONE',  ( -100.3628595697173864, -296.9812390932145263, -307.7670017612341553 ) ) ;
#38189 = CARTESIAN_POINT ( 'NONE',  ( -34.08997682767452631, -299.4072287231633709, -193.8535555751990387 ) ) ;
#38190 = CARTESIAN_POINT ( 'NONE',  ( -89.25422137235663911, -272.9630121942633423, -219.0076602137361022 ) ) ;
#38191 = CARTESIAN_POINT ( 'NONE',  ( -5.207191147485279004, -294.4751929007266540, -202.5799045153537463 ) ) ;
#38192 = CARTESIAN_POINT ( 'NONE',  ( 22.40648644523092159, -288.3706634549013188, -318.9529948112489137 ) ) ;
#38193 = CARTESIAN_POINT ( 'NONE',  ( -85.86098415119855076, -277.4664998374685752, -212.3689101532220604 ) ) ;
#38194 = CARTESIAN_POINT ( 'NONE',  ( -99.03040929027332595, -289.7721585397893591, -316.4644066337247068 ) ) ;
#38195 = ADVANCED_FACE ( 'NONE', ( #73831 ), #23641, .T. ) ;
#38196 = CARTESIAN_POINT ( 'NONE',  ( -109.8576196795451807, -289.4750679476808273, -280.6908118294176688 ) ) ;
#38197 = CARTESIAN_POINT ( 'NONE',  ( -7.949881231717635721, -290.4370185403515734, -201.3462844993334500 ) ) ;
#38198 = ORIENTED_EDGE ( 'NONE', *, *, #25604, .T. ) ;
#38199 = CARTESIAN_POINT ( 'NONE',  ( 200.1417227593101416, 66.37791233065237861, 9.866782148935371310 ) ) ;
#38200 = CARTESIAN_POINT ( 'NONE',  ( -82.58928494692568734, -289.1975188984123974, -327.7252575604900926 ) ) ;
#38201 = CARTESIAN_POINT ( 'NONE',  ( 175.2296996224750103, 214.5000000000000568, 0.000000000000000000 ) ) ;
#38202 = CARTESIAN_POINT ( 'NONE',  ( -78.40674263858510074, -286.4550670128155616, -205.5037167377598166 ) ) ;
#38203 = CARTESIAN_POINT ( 'NONE',  ( -67.68488546085839630, -291.9805209788416391, -333.4427485647536855 ) ) ;
#38204 = CARTESIAN_POINT ( 'NONE',  ( 36.86602852210865677, -292.8576334676833994, -290.0088461502414248 ) ) ;
#38205 = CARTESIAN_POINT ( 'NONE',  ( -61.06275791114273943, -284.6688200554312402, -343.1530184357202415 ) ) ;
#38206 = CARTESIAN_POINT ( 'NONE',  ( -106.1744418274619903, -284.0601348321706610, -294.8232535178393618 ) ) ;
#38207 = CARTESIAN_POINT ( 'NONE',  ( -101.2097353058410221, -273.2865370362063686, -227.2560281227328858 ) ) ;
#38208 = CARTESIAN_POINT ( 'NONE',  ( 30.62454061274588213, -276.4934919209092641, -242.2662758217954035 ) ) ;
#38209 = CARTESIAN_POINT ( 'NONE',  ( 20.63899226741434489, -290.9216286073296374, -223.3293401474844870 ) ) ;
#38210 = CARTESIAN_POINT ( 'NONE',  ( -36.71735929268815823, -272.8550897420360002, -196.9542163663845713 ) ) ;
#38211 = ORIENTED_EDGE ( 'NONE', *, *, #43955, .T. ) ;
#38212 = CARTESIAN_POINT ( 'NONE',  ( -49.37856652629597676, -155.6656457446864010, -366.7448178265262868 ) ) ;
#38213 = CARTESIAN_POINT ( 'NONE',  ( -63.08333844951189917, -287.6345917927048390, -200.4585746506386954 ) ) ;
#38214 = AXIS2_PLACEMENT_3D ( 'NONE', #89619, #24307, #46081 ) ;
#38215 = CARTESIAN_POINT ( 'NONE',  ( -98.02141753380104205, -297.0032661770089248, -317.2595657885099740 ) ) ;
#38216 = CARTESIAN_POINT ( 'NONE',  ( -68.82634408111194091, -286.2783572065064845, -204.3729961819459504 ) ) ;
#38217 = CARTESIAN_POINT ( 'NONE',  ( -82.41783001576253298, -276.7098571323332408, -332.4977635846553881 ) ) ;
#38218 = CARTESIAN_POINT ( 'NONE',  ( 37.97243851665219694, -294.3980082376273231, -285.8882976108286584 ) ) ;
#38219 = CARTESIAN_POINT ( 'NONE',  ( 21.15190270237869186, -285.0342599829427286, -222.2071574813568020 ) ) ;
#38220 = CARTESIAN_POINT ( 'NONE',  ( 15.46726557943651592, -294.6629259380151780, -326.3696658334123981 ) ) ;
#38222 = CARTESIAN_POINT ( 'NONE',  ( -85.94626496167029472, -291.6900750801716526, -215.7982516429003965 ) ) ;
#38221 = AXIS2_PLACEMENT_3D ( 'NONE', #2997, #16280, #30965 ) ;
#38223 = DIRECTION ( 'NONE',  ( 1.000000000000000000, 0.000000000000000000, 0.000000000000000000 ) ) ;
#38224 = CIRCLE ( 'NONE', #68456, 7.999999999999992895 ) ;
#38225 = CARTESIAN_POINT ( 'NONE',  ( 175.2296996224750103, 20.99999999999998934, 0.000000000000000000 ) ) ;
#38226 = CARTESIAN_POINT ( 'NONE',  ( 26.24832809208005813, -24.45034260818095007, -341.6199306127273303 ) ) ;
#38227 = CARTESIAN_POINT ( 'NONE',  ( -107.2983151197432079, -286.4658101120140827, -239.7530354811208326 ) ) ;
#38228 = CARTESIAN_POINT ( 'NONE',  ( -88.52914483777347243, -275.1952119285919025, -334.4957818155094174 ) ) ;
#38229 = EDGE_LOOP ( 'NONE', ( #14718, #76352, #68658 ) ) ;
#38231 = CARTESIAN_POINT ( 'NONE',  ( -73.96308360780625435, -282.4708357146256503, -333.9256661511798256 ) ) ;
#38230 = VECTOR ( 'NONE', #7683, 1000.000000000000000 ) ;
#38232 = CARTESIAN_POINT ( 'NONE',  ( 24.10433119332092744, -284.1330263689860089, -313.0742735949146436 ) ) ;
#38233 = CARTESIAN_POINT ( 'NONE',  ( -110.7722160373275386, -273.8307757778172800, -270.3773979239509231 ) ) ;
#38234 = CARTESIAN_POINT ( 'NONE',  ( -4.434163912197863766, -281.2017068078284296, -339.3370803435893777 ) ) ;
#38235 = CARTESIAN_POINT ( 'NONE',  ( -40.00797838916162164, -284.0385879478847642, -195.7639480264176655 ) ) ;
#38236 = CARTESIAN_POINT ( 'NONE',  ( -65.78583342212881746, -275.5444618774009200, -200.1244076857425682 ) ) ;
#38237 = CARTESIAN_POINT ( 'NONE',  ( -110.2740881995150630, -297.1017357810082444, -266.0188591581253945 ) ) ;
#38238 = CARTESIAN_POINT ( 'NONE',  ( 20.58185079837913989, -291.6034632902216117, -225.1068386577035199 ) ) ;
#38239 = CARTESIAN_POINT ( 'NONE',  ( -111.2415884289707293, -279.4705056754106067, -249.0980209400465810 ) ) ;
#38240 = CARTESIAN_POINT ( 'NONE',  ( 28.03050442123319286, -275.9940402596490685, -302.9631461159615355 ) ) ;
#38241 = CARTESIAN_POINT ( 'NONE',  ( -48.94629074504154431, -298.8491627244250708, -194.4251155180126318 ) ) ;
#38242 = CARTESIAN_POINT ( 'NONE',  ( -59.58852979488969481, -276.2540416485381911, -343.7543811530905487 ) ) ;
#38243 = CARTESIAN_POINT ( 'NONE',  ( -31.54385115900521086, -124.1296239073781607, -364.1778657101933732 ) ) ;
#38244 = CARTESIAN_POINT ( 'NONE',  ( -51.54890300056257502, -275.2335631807532081, -344.0553809397135296 ) ) ;
#38245 = CIRCLE ( 'NONE', #56468, 4.000000000000003553 ) ;
#38246 = CARTESIAN_POINT ( 'NONE',  ( 10.84093783140056111, -295.8263448672410618, -329.7339507977677044 ) ) ;
#38247 = LINE ( 'NONE', #60992, #1962 ) ;
#38248 = DIRECTION ( 'NONE',  ( 0.000000000000000000, -1.000000000000000000, 0.000000000000000000 ) ) ;
#38249 = VECTOR ( 'NONE', #16417, 1000.000000000000114 ) ;
#38250 = CARTESIAN_POINT ( 'NONE',  ( -106.8297032076564363, -285.9426923828335134, -246.8430626459063433 ) ) ;
#38251 = CARTESIAN_POINT ( 'NONE',  ( -41.49108591558039905, -284.8637311041416069, -346.2860497495687468 ) ) ;
#38252 = CARTESIAN_POINT ( 'NONE',  ( 13.21603316624100799, -286.1300616758726960, -217.4915730602340318 ) ) ;
#38253 = CARTESIAN_POINT ( 'NONE',  ( -90.03061317398214669, -277.6926388087219379, -218.6135886400298034 ) ) ;
#38254 = CARTESIAN_POINT ( 'NONE',  ( -101.4562166480833270, -285.9075286045120947, -307.7802875325949685 ) ) ;
#38255 = CARTESIAN_POINT ( 'NONE',  ( -65.05911048295058663, -278.1631735808554140, -202.0789613358016084 ) ) ;
#38256 = CARTESIAN_POINT ( 'NONE',  ( -71.78731679912783648, -278.5983219187128839, -335.0879145805561734 ) ) ;
#38257 = CARTESIAN_POINT ( 'NONE',  ( -81.11288322568364606, -273.9318433865227576, -211.7991527701329915 ) ) ;
#38258 = CARTESIAN_POINT ( 'NONE',  ( 34.44030703506230395, -282.7027650657638560, -297.7746596684362430 ) ) ;
#38259 = VECTOR ( 'NONE', #12971, 1000.000000000000000 ) ;
#38260 = CARTESIAN_POINT ( 'NONE',  ( 17.17507782287434637, -281.2965836629814476, -215.9960167168562748 ) ) ;
#38261 = VERTEX_POINT ( 'NONE', #30746 ) ;
#38262 = EDGE_LOOP ( 'NONE', ( #81295, #42747 ) ) ;
#38263 = CARTESIAN_POINT ( 'NONE',  ( 198.0894686820296897, 18.12099305396623450, -11.05388702472888163 ) ) ;
#38264 = CARTESIAN_POINT ( 'NONE',  ( 38.40462979923098175, -289.3913045430080047, -268.6881026303229874 ) ) ;
#38265 = EDGE_CURVE ( 'NONE', #72058, #29328, #9888, .T. ) ;
#38266 = CARTESIAN_POINT ( 'NONE',  ( -66.87516899125938608, -296.8521327021429670, -203.4117984635471430 ) ) ;
#38267 = CARTESIAN_POINT ( 'NONE',  ( -33.53610219977581153, -291.4474667964885839, -193.5572755580007822 ) ) ;
#38268 = CARTESIAN_POINT ( 'NONE',  ( 31.63029556596134384, -285.6872523792127367, -244.2637082733112095 ) ) ;
#38270 = CARTESIAN_POINT ( 'NONE',  ( -19.81070340442436972, -290.5203253875714040, -198.4009697251290731 ) ) ;
#38269 = CARTESIAN_POINT ( 'NONE',  ( -42.72499257243614323, -287.6959801609669398, -343.8041946979590193 ) ) ;
#38271 = CARTESIAN_POINT ( 'NONE',  ( -93.56912619919566509, -286.4235205853242405, -223.1847779027603735 ) ) ;
#38272 = CARTESIAN_POINT ( 'NONE',  ( -107.8650874191867501, -276.2192798750934344, -296.0367544315753321 ) ) ;
#38273 = CARTESIAN_POINT ( 'NONE',  ( 18.04914815115305515, -286.6742007915108275, -322.6898323005310658 ) ) ;
#38274 = CARTESIAN_POINT ( 'NONE',  ( -65.15985027491844050, -287.6888408981169505, -200.6971229825820160 ) ) ;
#38275 = CARTESIAN_POINT ( 'NONE',  ( -40.29290318095328161, -287.0889835324059618, -345.4826013574561898 ) ) ;
#38276 = CARTESIAN_POINT ( 'NONE',  ( 22.00964024975775857, -283.0919163535518237, -313.2874522787940350 ) ) ;
#38277 = CARTESIAN_POINT ( 'NONE',  ( -101.6606146046005392, -293.0735131239127895, -231.3620507675984754 ) ) ;
#38278 = CARTESIAN_POINT ( 'NONE',  ( 82.13810571491718804, -300.3989273480411271, -193.5455884681284999 ) ) ;
#38279 = CARTESIAN_POINT ( 'NONE',  ( 125.0516381006427338, 8.053287430127817004, -21.50000000000000000 ) ) ;
#38280 = CARTESIAN_POINT ( 'NONE',  ( -96.23956147004734873, -299.1186847680306187, -223.0287175365528753 ) ) ;
#38281 = CARTESIAN_POINT ( 'NONE',  ( 29.12364956286375417, -280.3362722114337657, -239.6625714786590606 ) ) ;
#38282 = CARTESIAN_POINT ( 'NONE',  ( 21.74119983320849414, -280.1858429236260690, -316.5586458956761362 ) ) ;
#38283 = CARTESIAN_POINT ( 'NONE',  ( -37.69851085673302293, -294.2536496412075167, -347.2118646812024849 ) ) ;
#38284 = CARTESIAN_POINT ( 'NONE',  ( -35.09704152150739276, -296.4805792807970306, -196.5617361290730969 ) ) ;
#38285 = CARTESIAN_POINT ( 'NONE',  ( -39.21809448493219463, -275.1557312364776067, -344.7774693109050190 ) ) ;
#38286 = CARTESIAN_POINT ( 'NONE',  ( -73.53075092266404056, -296.8583466739870005, -334.3267031128733606 ) ) ;
#38287 = CARTESIAN_POINT ( 'NONE',  ( 153.6987871352777404, 19.48326534539592458, 11.45812909364015297 ) ) ;
#38288 = CARTESIAN_POINT ( 'NONE',  ( -97.33904415044567315, -271.7646587999304870, -223.0438377799489444 ) ) ;
#38289 = CARTESIAN_POINT ( 'NONE',  ( -70.38771778888315112, -293.7215275353015613, -338.8001034058748928 ) ) ;
#38290 = AXIS2_PLACEMENT_3D ( 'NONE', #30731, #74753, #8477 ) ;
#38291 = CARTESIAN_POINT ( 'NONE',  ( -14.68206905329882872, -293.7769330262451604, -200.3474333505411664 ) ) ;
#38292 = CARTESIAN_POINT ( 'NONE',  ( -18.20453976106250948, -63.49190233628851132, -21.50000000000000000 ) ) ;
#38293 = CARTESIAN_POINT ( 'NONE',  ( -4.770355730253565518, -293.2952865419438808, -204.8360249310942720 ) ) ;
#38294 = LINE ( 'NONE', #66278, #35369 ) ;
#38295 = TOROIDAL_SURFACE ( 'NONE', #35274, 2.000000000000000000, 1.000000000000000000 ) ;
#38297 = CARTESIAN_POINT ( 'NONE',  ( 16.15913863187499899, -294.2659977360418679, -320.0266014895304920 ) ) ;
#38296 = CARTESIAN_POINT ( 'NONE',  ( -110.6256133797539007, -282.3473357903983469, -287.9621785684037150 ) ) ;
#38298 = CARTESIAN_POINT ( 'NONE',  ( -55.70218118981227917, -283.2821991931421621, -345.1400771567944616 ) ) ;
#38299 = CARTESIAN_POINT ( 'NONE',  ( 36.83627937149711329, -283.2889636592559555, -255.9756545566330601 ) ) ;
#38300 = CARTESIAN_POINT ( 'NONE',  ( 2.733626958387584960, -286.2410543535992247, -204.6365985822053801 ) ) ;
#38301 = CARTESIAN_POINT ( 'NONE',  ( -106.3849543886326074, -288.9312600485454823, -241.3636454860020422 ) ) ;
#38302 = CARTESIAN_POINT ( 'NONE',  ( -85.28047601435908120, -270.9094976428775681, -210.1954327657594206 ) ) ;
#38303 = CARTESIAN_POINT ( 'NONE',  ( -3.220396904966186025, -281.0896718150971196, -338.6284356751381779 ) ) ;
#38304 = AXIS2_PLACEMENT_3D ( 'NONE', #41430, #66505, #80694 ) ;
#38305 = CARTESIAN_POINT ( 'NONE',  ( -79.57910719044741654, -284.1532785482091299, -210.1551150911958814 ) ) ;
#38306 = CARTESIAN_POINT ( 'NONE',  ( -75.52177049016565036, -288.4694461545187778, -336.8725811825119649 ) ) ;
#38307 = LINE ( 'NONE', #83256, #11291 ) ;
#38308 = CARTESIAN_POINT ( 'NONE',  ( 18.59194129151673280, -295.8306440200837528, -318.5246364747315511 ) ) ;
#38309 = CARTESIAN_POINT ( 'NONE',  ( -107.9749472046090233, -280.3507179817029851, -241.2140649768817298 ) ) ;
#38311 = CARTESIAN_POINT ( 'NONE',  ( -46.45488995043136526, -279.6001736171690482, -197.8597614123047492 ) ) ;
#38310 = CARTESIAN_POINT ( 'NONE',  ( 23.54214447539355959, -292.1747373539700448, -314.7851444973658204 ) ) ;
#38312 = CARTESIAN_POINT ( 'NONE',  ( 35.48710783376738220, -294.0357408516879900, -295.5238188349825919 ) ) ;
#38313 = VECTOR ( 'NONE', #90435, 1000.000000000000000 ) ;
#38314 = CARTESIAN_POINT ( 'NONE',  ( -54.61129212475985639, -283.9117464541345726, -196.8011058332371306 ) ) ;
#38315 = CARTESIAN_POINT ( 'NONE',  ( -61.73089623349540034, -279.3691083292260942, -341.3396322565309333 ) ) ;
#38316 = CARTESIAN_POINT ( 'NONE',  ( 16.32342481155527381, -293.3248976544497282, -320.1954717306409179 ) ) ;
#38317 = CARTESIAN_POINT ( 'NONE',  ( 94.80756045878979421, -297.7061134510668694, -195.4061741161222585 ) ) ;
#38318 = ORIENTED_EDGE ( 'NONE', *, *, #51997, .F. ) ;
#38319 = CARTESIAN_POINT ( 'NONE',  ( -74.94434090351494149, -282.8906705383787994, 74.50000000000001421 ) ) ;
#38320 = VECTOR ( 'NONE', #45746, 1000.000000000000000 ) ;
#38321 = CARTESIAN_POINT ( 'NONE',  ( 1.228735692626827136, -282.5494119252215910, -206.3937974810505409 ) ) ;
#38322 = CARTESIAN_POINT ( 'NONE',  ( -55.82492791742164684, -294.8041295310868577, -341.0984725911246187 ) ) ;
#38323 = FACE_OUTER_BOUND ( 'NONE', #17517, .T. ) ;
#38324 = CARTESIAN_POINT ( 'NONE',  ( -37.30987171927208834, -277.5523547857346784, -195.3611179825600175 ) ) ;
#38325 = CARTESIAN_POINT ( 'NONE',  ( 25.20142870748443187, -274.1565618822819488, -225.7009995439237287 ) ) ;
#38326 = CARTESIAN_POINT ( 'NONE',  ( 37.02901749127890696, -289.0939504823149377, -288.3690796320923369 ) ) ;
#38327 = CARTESIAN_POINT ( 'NONE',  ( -96.76012430423257626, -290.9790014413030690, -227.8674726265915353 ) ) ;
#38328 = CARTESIAN_POINT ( 'NONE',  ( -38.38291887026635152, -281.5589946963260672, -196.6626192903837307 ) ) ;
#38329 = CARTESIAN_POINT ( 'NONE',  ( -62.31941323911313901, -275.3218859623015078, -200.9165050708860178 ) ) ;
#38330 = ADVANCED_FACE ( 'NONE', ( #52507 ), #81383, .T. ) ;
#38331 = CARTESIAN_POINT ( 'NONE',  ( -62.43033092924258654, -278.5134028308034431, -201.3314571112932185 ) ) ;
#38332 = CARTESIAN_POINT ( 'NONE',  ( -99.56579800509847189, -272.9884573393094342, -224.9167645849021824 ) ) ;
#38333 = CARTESIAN_POINT ( 'NONE',  ( -80.38285782364107490, -293.3845167254562512, -209.5626534471329023 ) ) ;
#38334 = DIRECTION ( 'NONE',  ( 0.000000000000000000, 0.000000000000000000, 1.000000000000000000 ) ) ;
#38335 = ADVANCED_FACE ( 'NONE', ( #9409 ), #88946, .T. ) ;
#38336 = DIRECTION ( 'NONE',  ( 0.000000000000000000, 1.000000000000000000, 0.000000000000000000 ) ) ;
#38337 = CARTESIAN_POINT ( 'NONE',  ( -25.19573484224367022, -290.3450152465179031, -195.5762197373435924 ) ) ;
#38338 = CARTESIAN_POINT ( 'NONE',  ( -108.5935202911870476, -272.2728100420393389, -254.2004693157816746 ) ) ;
#38339 = DIRECTION ( 'NONE',  ( 0.000000000000000000, 1.000000000000000000, 0.000000000000000000 ) ) ;
#38340 = CARTESIAN_POINT ( 'NONE',  ( -112.1841381722990150, -291.8836891193671477, -285.3039995540744371 ) ) ;
#38341 = CARTESIAN_POINT ( 'NONE',  ( -111.2869819898779866, -293.4805209788416391, -234.7871824221999191 ) ) ;
#38342 = CARTESIAN_POINT ( 'NONE',  ( -41.44838100212109566, -288.0005051074205085, -195.6277357957662559 ) ) ;
#38343 = CARTESIAN_POINT ( 'NONE',  ( 37.17738074211008126, -273.6401488022884223, -277.2120311342031300 ) ) ;
#38344 = CARTESIAN_POINT ( 'NONE',  ( 24.98609461861684977, -276.9191967559033856, -229.6602555895457272 ) ) ;
#38345 = CARTESIAN_POINT ( 'NONE',  ( 23.78408674541283219, -291.0510818093234207, -227.8539174325783847 ) ) ;
#38346 = CARTESIAN_POINT ( 'NONE',  ( -8.036980334142889149, -282.2923350966429439, -200.4790360668626192 ) ) ;
#38347 = VERTEX_POINT ( 'NONE', #60569 ) ;
#38348 = CARTESIAN_POINT ( 'NONE',  ( 5.645347047554210462, -281.8007761876296513, -329.4881544632503960 ) ) ;
#38349 = CARTESIAN_POINT ( 'NONE',  ( -99.39153700770440025, -279.0311643601683045, -315.4535023684555881 ) ) ;
#38350 = CARTESIAN_POINT ( 'NONE',  ( 24.77625827103772238, -280.9447965455061649, -315.2093527251433898 ) ) ;
#38351 = CARTESIAN_POINT ( 'NONE',  ( -70.18942206231223224, -278.4156382876280418, -339.7574056422278090 ) ) ;
#38352 = CARTESIAN_POINT ( 'NONE',  ( 0.000000000000000000, 0.000000000000000000, 0.000000000000000000 ) ) ;
#38353 = CARTESIAN_POINT ( 'NONE',  ( 38.62509353769181075, -276.9747198964386712, -262.6311570143912490 ) ) ;
#38354 = CARTESIAN_POINT ( 'NONE',  ( -102.0455923789670294, -293.4805209788416391, -239.2376011013261916 ) ) ;
#38355 = ORIENTED_EDGE ( 'NONE', *, *, #90249, .F. ) ;
#38356 = CARTESIAN_POINT ( 'NONE',  ( -110.4316933438511370, -298.7682539757504969, -253.5428676159656050 ) ) ;
#38357 = VECTOR ( 'NONE', #58106, 1000.000000000000000 ) ;
#38358 = CARTESIAN_POINT ( 'NONE',  ( -110.4296494165745202, -291.5489539411085502, -276.6701365953661593 ) ) ;
#38359 = CARTESIAN_POINT ( 'NONE',  ( -15.93270950355617543, -274.7941352625059608, -341.9240697206458890 ) ) ;
#38360 = CARTESIAN_POINT ( 'NONE',  ( 2.665923041233587476, -290.2839707296153620, -335.0244330072943058 ) ) ;
#38361 = CARTESIAN_POINT ( 'NONE',  ( -102.4966600036601960, -290.3516437447562453, -237.1020852761221249 ) ) ;
#38362 = CARTESIAN_POINT ( 'NONE',  ( 37.44311689830367129, -287.2867217584202990, -288.4932048968876188 ) ) ;
#38363 = CARTESIAN_POINT ( 'NONE',  ( 209.6160175266639669, 36.70030375927228761, 13.08022668053253668 ) ) ;
#38364 = CARTESIAN_POINT ( 'NONE',  ( -85.39797985797937940, -282.1294617860167477, -326.3703528610641911 ) ) ;
#38365 = CARTESIAN_POINT ( 'NONE',  ( -85.46809442110621546, -291.5858348596074734, -326.9507650845525859 ) ) ;
#38366 = CARTESIAN_POINT ( 'NONE',  ( -54.90297507577628267, -284.3022733159571658, -198.7380159556053059 ) ) ;
#38367 = CARTESIAN_POINT ( 'NONE',  ( 7.429577419464150623, -281.9921778690282395, -212.0148708629042460 ) ) ;
#38368 = CARTESIAN_POINT ( 'NONE',  ( 37.48756817190958657, -288.2778622312388279, -253.1738733812769055 ) ) ;
#38369 = AXIS2_PLACEMENT_3D ( 'NONE', #87095, #49259, #85239 ) ;
#38370 = CARTESIAN_POINT ( 'NONE',  ( -98.04823361276523030, -279.6097408603251324, -229.6177955603075134 ) ) ;
#38371 = CARTESIAN_POINT ( 'NONE',  ( -22.25688375772180194, -291.0360023838061920, -195.2040939807425843 ) ) ;
#38372 = CARTESIAN_POINT ( 'NONE',  ( 38.93157505034587018, -288.4769434130623154, -280.0925696633081543 ) ) ;
#38373 = CARTESIAN_POINT ( 'NONE',  ( 18.60437654828044174, -288.7663387799738075, -323.1774356101923331 ) ) ;
#38374 = CARTESIAN_POINT ( 'NONE',  ( -100.4000645825083211, -284.2140654984655725, -307.1394088186335694 ) ) ;
#38375 = ORIENTED_EDGE ( 'NONE', *, *, #9862, .F. ) ;
#38376 = CARTESIAN_POINT ( 'NONE',  ( 195.4471090089123777, 26.99502172241844633, 13.95936681960324854 ) ) ;
#38377 = CARTESIAN_POINT ( 'NONE',  ( -1.410869199410667685, -294.3838741617315122, -203.6581879796983401 ) ) ;
#38378 = AXIS2_PLACEMENT_3D ( 'NONE', #84644, #62433, #90338 ) ;
#38379 = CARTESIAN_POINT ( 'NONE',  ( 27.67792636295152775, -292.7688439279630188, -310.7811613359442049 ) ) ;
#38380 = AXIS2_PLACEMENT_3D ( 'NONE', #22524, #87377, #51396 ) ;
#38381 = CARTESIAN_POINT ( 'NONE',  ( 26.96765282657602825, -275.0889275876850775, -305.5058730060741254 ) ) ;
#38382 = CARTESIAN_POINT ( 'NONE',  ( -31.91013715723157418, -297.4670732795708545, -193.4636322180529646 ) ) ;
#38383 = CARTESIAN_POINT ( 'NONE',  ( 34.44647330940923524, -292.2502373729911369, -287.0649462891273060 ) ) ;
#38384 = CARTESIAN_POINT ( 'NONE',  ( -108.8083567849265023, -295.0433392946682716, -251.0641941214466613 ) ) ;
#38385 = CARTESIAN_POINT ( 'NONE',  ( -106.9527213638054093, -292.0645909574458301, -247.0923357363581090 ) ) ;
#38386 = CARTESIAN_POINT ( 'NONE',  ( 35.60144556126719095, -294.5292928190697808, -262.5553946875014617 ) ) ;
#38387 = CARTESIAN_POINT ( 'NONE',  ( 133.0872704186301405, -299.5541904835127980, -195.3611179825600175 ) ) ;
#38388 = AXIS2_PLACEMENT_3D ( 'NONE', #41654, #70571, #40235 ) ;
#38389 = CARTESIAN_POINT ( 'NONE',  ( -47.41178340180002948, -293.1796984736866420, -344.8501899837609699 ) ) ;
#38390 = CARTESIAN_POINT ( 'NONE',  ( -66.75749003150183114, -299.6669560479044208, -201.3566650642730167 ) ) ;
#38391 = CARTESIAN_POINT ( 'NONE',  ( -8.113602617729419819, -289.6010680811129987, -337.5653682545494689 ) ) ;
#38392 = EDGE_CURVE ( 'NONE', #69141, #84950, #79959, .T. ) ;
#38393 = EDGE_CURVE ( 'NONE', #135, #23299, #52042, .T. ) ;
#38394 = CARTESIAN_POINT ( 'NONE',  ( 7.287660961615398669, -278.4275849709833324, -331.1433368424354740 ) ) ;
#38395 = CARTESIAN_POINT ( 'NONE',  ( -39.96480596265028140, -275.8793195343735647, -346.9321209962316175 ) ) ;
#38396 = AXIS2_PLACEMENT_3D ( 'NONE', #40517, #76545, #46699 ) ;
#38397 = CARTESIAN_POINT ( 'NONE',  ( -49.69467705304472815, -273.2472898199230826, -194.4079987789754966 ) ) ;
#38398 = CARTESIAN_POINT ( 'NONE',  ( 16.85786742071456601, -280.3531236580254813, -321.4621273476014380 ) ) ;
#38399 = CARTESIAN_POINT ( 'NONE',  ( -53.97666152125205485, -275.6619971649533909, -344.7772703764786115 ) ) ;
#38400 = CARTESIAN_POINT ( 'NONE',  ( -108.3075101263664806, -295.4882345872784981, -251.2051467548723167 ) ) ;
#38401 = CARTESIAN_POINT ( 'NONE',  ( -95.59627442016343934, -275.2030350989207932, -223.1034399805188855 ) ) ;
#38402 = CARTESIAN_POINT ( 'NONE',  ( -48.89972073598492130, -274.5525847951537344, -198.1274311562501964 ) ) ;
#38403 = CARTESIAN_POINT ( 'NONE',  ( 196.2154913428680914, 25.52575416299670152, 11.66205930223015308 ) ) ;
#38405 = CARTESIAN_POINT ( 'NONE',  ( 22.28205928802048774, -274.7973126082226827, -228.2205122141655522 ) ) ;
#38404 = CARTESIAN_POINT ( 'NONE',  ( -109.6466878092473110, -288.8442713887507125, -249.1385931478510827 ) ) ;
#38406 = CARTESIAN_POINT ( 'NONE',  ( 25.85170750003431550, -288.1345815258399625, -314.4480433355608398 ) ) ;
#38407 = CARTESIAN_POINT ( 'NONE',  ( 51.15003443965340324, -301.1346102307301749, -194.9762188656702335 ) ) ;
#38408 = CARTESIAN_POINT ( 'NONE',  ( -95.01048168695832885, -295.2117324032735155, -222.6511494115316054 ) ) ;
#38409 = CARTESIAN_POINT ( 'NONE',  ( -74.20751820094648110, -282.7261465352300434, -337.8376250146515645 ) ) ;
#38410 = DIRECTION ( 'NONE',  ( 0.000000000000000000, 0.000000000000000000, -1.000000000000000000 ) ) ;
#38411 = CARTESIAN_POINT ( 'NONE',  ( 37.70396000512317869, -279.5638603164040319, -271.2858296272250982 ) ) ;
#38412 = DIRECTION ( 'NONE',  ( -1.000000000000000000, -0.000000000000000000, -0.000000000000000000 ) ) ;
#38413 = CARTESIAN_POINT ( 'NONE',  ( -77.45942791351100709, -290.2954812061835241, -208.8981338247106692 ) ) ;
#38414 = CARTESIAN_POINT ( 'NONE',  ( -29.33457778158224727, -281.0893635188935491, -344.2145858785827954 ) ) ;
#38415 = CARTESIAN_POINT ( 'NONE',  ( 200.5094052069776467, 41.41475569182169636, 9.999999999999998224 ) ) ;
#38416 = FACE_OUTER_BOUND ( 'NONE', #42687, .T. ) ;
#38417 = CARTESIAN_POINT ( 'NONE',  ( -63.47437060616803706, -289.7114337277214418, -200.0611593613644743 ) ) ;
#38418 = CARTESIAN_POINT ( 'NONE',  ( -36.74976385216874064, -275.5798458440512491, -196.6576269246798176 ) ) ;
#38419 = CARTESIAN_POINT ( 'NONE',  ( -97.72191922565930611, -285.1240637988797744, -317.5017359469233043 ) ) ;
#38421 = CARTESIAN_POINT ( 'NONE',  ( -42.67412919225751722, -285.9830368293920060, -197.5435117709969575 ) ) ;
#38420 = CARTESIAN_POINT ( 'NONE',  ( 0.4959079117829636729, -272.6320497298677878, -204.9425260007590452 ) ) ;
#38422 = CARTESIAN_POINT ( 'NONE',  ( 16.03768453958602436, -277.7017458304090383, -321.0169785486190790 ) ) ;
#38423 = CARTESIAN_POINT ( 'NONE',  ( -8.665984192381040785, -277.4698995446594836, -337.6822321636994388 ) ) ;
#38424 = CARTESIAN_POINT ( 'NONE',  ( -2.538993479511827189, -284.5919402284860666, -336.7973450088994127 ) ) ;
#38425 = ORIENTED_EDGE ( 'NONE', *, *, #54408, .T. ) ;
#38426 = CIRCLE ( 'NONE', #61107, 15.36528803885689420 ) ;
#38427 = CARTESIAN_POINT ( 'NONE',  ( 114.7448031289451222, -299.5541904835127980, -193.0244903219134756 ) ) ;
#38428 = CARTESIAN_POINT ( 'NONE',  ( -44.79773735905121157, -294.9772411305903574, -347.0526843203343219 ) ) ;
#38429 = CARTESIAN_POINT ( 'NONE',  ( -49.71853397641705641, -287.8735649070609384, -196.6969030181209632 ) ) ;
#38430 = CARTESIAN_POINT ( 'NONE',  ( 196.4890680266781828, 25.15197166163899922, 13.65125671900674753 ) ) ;
#38431 = CARTESIAN_POINT ( 'NONE',  ( 40.64545035920995986, -285.2666405000203440, -288.1938231032136741 ) ) ;
#38432 = CARTESIAN_POINT ( 'NONE',  ( -112.6898927689198757, -277.6527757842909523, -256.0031111151678260 ) ) ;
#38433 = CARTESIAN_POINT ( 'NONE',  ( -94.10165198749720616, -289.6489474031497480, -219.5206982253849333 ) ) ;
#38434 = VECTOR ( 'NONE', #52505, 1000.000000000000000 ) ;
#38435 = CARTESIAN_POINT ( 'NONE',  ( -101.6053319760717670, -286.5623667823225560, -234.1885920237355379 ) ) ;
#38436 = CARTESIAN_POINT ( 'NONE',  ( -71.42802845166538361, -281.3557639055264872, -204.6498298136843630 ) ) ;
#38437 = CARTESIAN_POINT ( 'NONE',  ( -64.35598605796496940, -287.1317016380446603, -198.8709448788910095 ) ) ;
#38438 = CARTESIAN_POINT ( 'NONE',  ( 15.34737533745692240, -284.3084113693651602, -323.8089971205864686 ) ) ;
#38439 = CARTESIAN_POINT ( 'NONE',  ( 33.02062984517930033, -276.1180004560837915, -301.6363881687481694 ) ) ;
#38440 = CARTESIAN_POINT ( 'NONE',  ( -112.1740853773269038, -270.5882458020582817, -267.5434424033534810 ) ) ;
#38441 = CARTESIAN_POINT ( 'NONE',  ( -50.93754487765809813, -279.7163340108675129, -194.5709272582197116 ) ) ;
#38442 = CIRCLE ( 'NONE', #47501, 20.00000000000000355 ) ;
#38443 = CARTESIAN_POINT ( 'NONE',  ( -92.93631029256951592, -299.1664390810638565, -220.8580522193773277 ) ) ;
#38444 = AXIS2_PLACEMENT_3D ( 'NONE', #7181, #19972, #57386 ) ;
#38445 = CARTESIAN_POINT ( 'NONE',  ( 165.7865175155837676, 3.000000000000000000, 9.000000000000001776 ) ) ;
#38446 = DIRECTION ( 'NONE',  ( 0.000000000000000000, 0.000000000000000000, 1.000000000000000000 ) ) ;
#38447 = CARTESIAN_POINT ( 'NONE',  ( -112.8531441054083047, -270.8995448367077756, -261.8760816757083489 ) ) ;
#38448 = CARTESIAN_POINT ( 'NONE',  ( 161.2494399300530290, 8.542400036368780647, 10.00000000000000000 ) ) ;
#38449 = CARTESIAN_POINT ( 'NONE',  ( -94.50510170511438446, -277.4175670830590548, -315.8820263994580273 ) ) ;
#38450 = CIRCLE ( 'NONE', #38388, 4.499999999999990230 ) ;
#38451 = CARTESIAN_POINT ( 'NONE',  ( -81.03655275476577913, -274.6785734826400471, -207.3780857020441601 ) ) ;
#38452 = CARTESIAN_POINT ( 'NONE',  ( 1.963337758915105979, -281.5982888175031462, -336.2999851971397334 ) ) ;
#38453 = CARTESIAN_POINT ( 'NONE',  ( -45.45152568235523205, -290.9164612216891896, -343.9288061492744077 ) ) ;
#38454 = CARTESIAN_POINT ( 'NONE',  ( -74.25384824107425175, -297.0533710928539222, -337.2050230729130931 ) ) ;
#38455 = CARTESIAN_POINT ( 'NONE',  ( -79.24685402941869938, -296.8093402388691402, -334.4857372358493990 ) ) ;
#38456 = CARTESIAN_POINT ( 'NONE',  ( 24.85108799284440195, -294.9884647037296759, -228.7427862960367122 ) ) ;
#38457 = CARTESIAN_POINT ( 'NONE',  ( 30.97806932586036055, -279.9546092500733607, -301.0240919962785142 ) ) ;
#38458 = CARTESIAN_POINT ( 'NONE',  ( -27.38959879430306188, -282.0996023331566676, -196.5371774006363239 ) ) ;
#38459 = CARTESIAN_POINT ( 'NONE',  ( -96.41722003954978959, -295.2571237522643059, -225.0480045448180704 ) ) ;
#38460 = CARTESIAN_POINT ( 'NONE',  ( -107.4826924242310753, -285.7677275432773740, -300.2732173316468334 ) ) ;
#38461 = AXIS2_PLACEMENT_3D ( 'NONE', #90474, #19473, #41707 ) ;
#38462 = EDGE_CURVE ( 'NONE', #33292, #55168, #70178, .T. ) ;
#38463 = CARTESIAN_POINT ( 'NONE',  ( 19.74557775531378923, -287.1200090360013633, -316.3531692368167114 ) ) ;
#38464 = CARTESIAN_POINT ( 'NONE',  ( 140.6514286645508207, 179.2331402481280236, -240.9484025443371706 ) ) ;
#38465 = VERTEX_POINT ( 'NONE', #17934 ) ;
#38466 = CARTESIAN_POINT ( 'NONE',  ( -5.885770650012288385, -287.2213916663812370, -339.9968185629729192 ) ) ;
#38467 = CARTESIAN_POINT ( 'NONE',  ( 35.65093069525761393, -287.2637592726157436, -273.7650458607844826 ) ) ;
#38468 = ORIENTED_EDGE ( 'NONE', *, *, #93160, .F. ) ;
#38469 = CARTESIAN_POINT ( 'NONE',  ( -102.6476277784160231, -285.1041721060128680, -310.5684347669297267 ) ) ;
#38470 = CARTESIAN_POINT ( 'NONE',  ( 35.12761081617328074, -276.0089223663409825, -279.7248369698144188 ) ) ;
#38471 = CARTESIAN_POINT ( 'NONE',  ( -92.57985671707740494, -290.2044330025888712, -217.0855957570606449 ) ) ;
#38472 = CARTESIAN_POINT ( 'NONE',  ( 17.75903708443733464, -282.9406334571459070, -324.0769510528670594 ) ) ;
#38473 = CARTESIAN_POINT ( 'NONE',  ( 1.008615363151603272, -282.0739696739936448, -204.3315720239004349 ) ) ;
#38474 = CARTESIAN_POINT ( 'NONE',  ( 36.45962783886409397, -282.1621962055115205, -292.4330717640871171 ) ) ;
#38475 = CARTESIAN_POINT ( 'NONE',  ( 11.30582025366161858, -280.7490792086498459, -215.9330116338370260 ) ) ;
#38476 = CARTESIAN_POINT ( 'NONE',  ( -21.39648532958014826, -292.3380690714489560, -340.3683826091709079 ) ) ;
#38477 = CARTESIAN_POINT ( 'NONE',  ( -77.50303971134606229, -208.8530697131320153, -357.3053013794460639 ) ) ;
#38478 = ORIENTED_EDGE ( 'NONE', *, *, #3777, .F. ) ;
#38479 = CARTESIAN_POINT ( 'NONE',  ( 31.86072791008295013, -277.1783681167906366, -241.7461843042033820 ) ) ;
#38480 = CARTESIAN_POINT ( 'NONE',  ( -108.3143740274736757, -261.7878351234190859, -317.3776606196656189 ) ) ;
#38481 = CARTESIAN_POINT ( 'NONE',  ( 36.32278028721702867, -279.7278161541131567, -282.4189423701175770 ) ) ;
#38482 = CARTESIAN_POINT ( 'NONE',  ( -107.5549654667471060, -296.1694816034614632, -250.0143728171061923 ) ) ;
#38483 = CARTESIAN_POINT ( 'NONE',  ( 21.31666403547346178, -293.7314648761540639, -320.1478955151795844 ) ) ;
#38484 = CARTESIAN_POINT ( 'NONE',  ( 154.1818069414172783, 204.3837156544556422, -214.5532738587077404 ) ) ;
#38486 = CARTESIAN_POINT ( 'NONE',  ( -91.19028885873797208, -288.2330510603243852, -320.9013010507957233 ) ) ;
#38485 = CARTESIAN_POINT ( 'NONE',  ( -34.06005215504181649, -296.6672129428951052, -193.9511196260665145 ) ) ;
#38487 = CARTESIAN_POINT ( 'NONE',  ( -0.1184100674215761706, -296.4121496192478276, -334.6482339227985108 ) ) ;
#38488 = CARTESIAN_POINT ( 'NONE',  ( 11.44902650208045181, -288.0604527573427163, -215.3317840669182317 ) ) ;
#38489 = ADVANCED_FACE ( 'NONE', ( #61506 ), #41408, .T. ) ;
#38490 = ORIENTED_EDGE ( 'NONE', *, *, #13625, .T. ) ;
#38491 = CARTESIAN_POINT ( 'NONE',  ( 38.61728129580925639, -294.3497738350770874, -258.9118917159863145 ) ) ;
#38492 = CARTESIAN_POINT ( 'NONE',  ( -69.03018709037934286, -283.9728641881617364, -336.2067496658171990 ) ) ;
#38493 = CARTESIAN_POINT ( 'NONE',  ( -57.27154210512010479, -296.5955917733255092, -196.3412025614190100 ) ) ;
#38494 = CARTESIAN_POINT ( 'NONE',  ( 4.045928813690177428, -293.3970060694782660, -205.5583997515548162 ) ) ;
#38495 = CARTESIAN_POINT ( 'NONE',  ( 38.26360101978755068, -293.8660056368633491, -256.1004959158440784 ) ) ;
#38496 = CARTESIAN_POINT ( 'NONE',  ( -69.97054427848298985, -289.6610254597630387, -335.6770329349184863 ) ) ;
#38497 = VERTEX_POINT ( 'NONE', #19795 ) ;
#38498 = CARTESIAN_POINT ( 'NONE',  ( 157.3811296300183642, 16.14910309754966278, 7.138650918358441899 ) ) ;
#38499 = CARTESIAN_POINT ( 'NONE',  ( -67.70457009757159028, -299.5185176082915746, -200.8905144143280097 ) ) ;
#38500 = CARTESIAN_POINT ( 'NONE',  ( -73.74257889085031081, -272.3752130129523152, -202.9004891753010895 ) ) ;
#38501 = CARTESIAN_POINT ( 'NONE',  ( 18.66658292093065796, -281.2792539473255147, -317.5661790417046859 ) ) ;
#38502 = ORIENTED_EDGE ( 'NONE', *, *, #18406, .F. ) ;
#38503 = ORIENTED_EDGE ( 'NONE', *, *, #28819, .T. ) ;
#38504 = CARTESIAN_POINT ( 'NONE',  ( -42.80805925910741649, -276.6270520138905340, -347.1051459007585436 ) ) ;
#38505 = CARTESIAN_POINT ( 'NONE',  ( -40.79216921455333278, -272.4080364295741674, -196.5915752667416427 ) ) ;
#38506 = CARTESIAN_POINT ( 'NONE',  ( -62.75367302011007808, -281.5784002811615210, -200.5566020078079248 ) ) ;
#38507 = CARTESIAN_POINT ( 'NONE',  ( -69.81273757450152573, -275.6238710964494771, -337.1321920999869803 ) ) ;
#38508 = CARTESIAN_POINT ( 'NONE',  ( -94.77155617724071135, -298.3991484513010732, -224.6561714183339689 ) ) ;
#38509 = CARTESIAN_POINT ( 'NONE',  ( -21.89605366827960964, -275.1962368745994354, -198.7731270007397484 ) ) ;
#38510 = CARTESIAN_POINT ( 'NONE',  ( -112.5447892850460505, -274.4547872134068029, -259.1171465317853517 ) ) ;
#38511 = CARTESIAN_POINT ( 'NONE',  ( -35.53734438785662775, -272.0947688877483870, -195.0146697697466038 ) ) ;
#38512 = CARTESIAN_POINT ( 'NONE',  ( 27.57325502563815789, -293.7470686021507049, -236.7465189929239386 ) ) ;
#38513 = CARTESIAN_POINT ( 'NONE',  ( 34.52917583849760774, -291.9192259512259966, -254.4929129107979975 ) ) ;
#38514 = CARTESIAN_POINT ( 'NONE',  ( -6.593530494673972342, -277.1514734525161998, -340.9024997457509585 ) ) ;
#38515 = EDGE_CURVE ( 'NONE', #9328, #83649, #36914, .T. ) ;
#38516 = CARTESIAN_POINT ( 'NONE',  ( 34.84133724452625103, -275.5740562193524852, -259.3862464096388862 ) ) ;
#38517 = CARTESIAN_POINT ( 'NONE',  ( -93.08378595305521230, -282.5169859453421282, -322.7837460224268966 ) ) ;
#38518 = CARTESIAN_POINT ( 'NONE',  ( 37.67440604498001022, -295.6230021717669274, -275.8785845459177040 ) ) ;
#38519 = CARTESIAN_POINT ( 'NONE',  ( 200.1126601882107252, 275.0000000000000568, -2.416251949619912853 ) ) ;
#38520 = CARTESIAN_POINT ( 'NONE',  ( -38.61749165448306087, -285.2329497985221565, -197.1982559707703899 ) ) ;
#38521 = VECTOR ( 'NONE', #37380, 1000.000000000000000 ) ;
#38522 = CARTESIAN_POINT ( 'NONE',  ( -98.31659834280573307, -281.9539909832136004, -314.4036871802330211 ) ) ;
#38523 = CARTESIAN_POINT ( 'NONE',  ( 31.80927144240720850, -274.4613172570902293, -295.6788772234957037 ) ) ;
#38524 = CARTESIAN_POINT ( 'NONE',  ( 26.04886463930497698, -284.0925361584082793, -310.5397254766070319 ) ) ;
#38525 = CARTESIAN_POINT ( 'NONE',  ( 33.23761890483539361, -276.4902060105467285, -250.0378959275174680 ) ) ;
#38526 = DIRECTION ( 'NONE',  ( 0.000000000000000000, 0.000000000000000000, -1.000000000000000000 ) ) ;
#38527 = CARTESIAN_POINT ( 'NONE',  ( 196.4265994039971304, 19.73582633127739427, 13.26925245973608547 ) ) ;
#38528 = CARTESIAN_POINT ( 'NONE',  ( -67.20316549286576446, -272.0669709513870771, -200.2559590933015841 ) ) ;
#38529 = AXIS2_PLACEMENT_3D ( 'NONE', #63322, #49548, #93100 ) ;
#38530 = CARTESIAN_POINT ( 'NONE',  ( -110.0474838609024602, -280.3071135841789214, -289.4877220180256359 ) ) ;
#38531 = CARTESIAN_POINT ( 'NONE',  ( 175.2296996224750103, 140.2072866198470251, 0.000000000000000000 ) ) ;
#38532 = CARTESIAN_POINT ( 'NONE',  ( -24.06344875422471219, -288.1404764920047796, -195.9237649757746738 ) ) ;
#38533 = CARTESIAN_POINT ( 'NONE',  ( -91.68632222370136731, -289.2779664695461861, -218.5995970954718359 ) ) ;
#38534 = AXIS2_PLACEMENT_3D ( 'NONE', #23678, #74809, #66767 ) ;
#38535 = DIRECTION ( 'NONE',  ( 1.000000000000000000, 0.000000000000000000, 0.000000000000000000 ) ) ;
#38536 = CARTESIAN_POINT ( 'NONE',  ( -110.7816523572172400, -295.3327331340378805, -271.4537965941055404 ) ) ;
#38537 = CARTESIAN_POINT ( 'NONE',  ( 14.93672385205651310, -286.4449433155193105, -323.0662587696817809 ) ) ;
#38538 = CARTESIAN_POINT ( 'NONE',  ( 81.08292338999881110, 82.25620239566015357, -296.3357184930298445 ) ) ;
#38539 = CARTESIAN_POINT ( 'NONE',  ( -53.02922665931427559, -295.8510235811711482, -196.9668153148425915 ) ) ;
#38540 = CARTESIAN_POINT ( 'NONE',  ( 36.82590184792485388, -286.2591133026817829, -288.3571208871751992 ) ) ;
#38541 = CARTESIAN_POINT ( 'NONE',  ( -0.8387789176852811224, -284.1588570990017502, -334.5014107697758732 ) ) ;
#38542 = CARTESIAN_POINT ( 'NONE',  ( -24.72420871733400105, -281.1332925138557357, -345.3463077315985288 ) ) ;
#38543 = CARTESIAN_POINT ( 'NONE',  ( -110.2456556156483174, -290.6131701911235723, -265.7356183765746209 ) ) ;
#38544 = CARTESIAN_POINT ( 'NONE',  ( 28.68772571341341404, -283.4155053428108317, -302.9651208116308112 ) ) ;
#38545 = CARTESIAN_POINT ( 'NONE',  ( 22.72317268907492505, -282.9358917705762906, -312.1320741675502859 ) ) ;
#38546 = CARTESIAN_POINT ( 'NONE',  ( -96.84496032399584919, -291.9010471635554040, -316.5971302783976284 ) ) ;
#38547 = CARTESIAN_POINT ( 'NONE',  ( 76.38462255090273345, -299.6058777463841807, -193.3579203087136023 ) ) ;
#38548 = CARTESIAN_POINT ( 'NONE',  ( -0.01378055072520428456, -286.6397010727742440, -336.1160537688457453 ) ) ;
#38549 = CARTESIAN_POINT ( 'NONE',  ( 1.195421383891718481, -274.5518939205146012, -203.6833226859605759 ) ) ;
#38550 = CARTESIAN_POINT ( 'NONE',  ( -14.36349944652816113, -294.3314635687355576, -199.3410567722573887 ) ) ;
#38551 = CYLINDRICAL_SURFACE ( 'NONE', #56038, 4.025000000000000355 ) ;
#38552 = CARTESIAN_POINT ( 'NONE',  ( -110.4542110544635705, -286.8376638359844719, -287.0812184334320705 ) ) ;
#38553 = CARTESIAN_POINT ( 'NONE',  ( -35.77586197230581178, -275.0324271114433259, -345.5242892143131712 ) ) ;
#38554 = CARTESIAN_POINT ( 'NONE',  ( 189.9243309297870610, 250.0000000000000568, 20.22542485937349355 ) ) ;
#38555 = CARTESIAN_POINT ( 'NONE',  ( -94.95274135883745714, -295.6335435708235195, -220.4084700009051403 ) ) ;
#38556 = CARTESIAN_POINT ( 'NONE',  ( -111.1686156865934691, -292.1770787729165022, -268.4612761058797332 ) ) ;
#38557 = CARTESIAN_POINT ( 'NONE',  ( -56.88089049190765678, -273.1421516632114503, -199.8660645403049898 ) ) ;
#38558 = CARTESIAN_POINT ( 'NONE',  ( -109.1070615161358006, -292.2918290585453747, -253.5596638670428149 ) ) ;
#38559 = CARTESIAN_POINT ( 'NONE',  ( -12.19062214125767696, -293.3287104482897689, -201.5260284210976920 ) ) ;
#38560 = CARTESIAN_POINT ( 'NONE',  ( -94.18614826009915930, -285.6488851040086274, -317.7603029178505949 ) ) ;
#38561 = CARTESIAN_POINT ( 'NONE',  ( -68.10829382968361756, -293.0812967459226002, -200.4038609825165054 ) ) ;
#38562 = CARTESIAN_POINT ( 'NONE',  ( -92.46844943382534154, -292.5988922430018988, -217.2353785349184818 ) ) ;
#38563 = CARTESIAN_POINT ( 'NONE',  ( -36.99768062687767411, -294.8810132462169804, -343.3727315176086563 ) ) ;
#38564 = CARTESIAN_POINT ( 'NONE',  ( 22.79190936736363682, -290.1646338507283076, -315.2039335150693660 ) ) ;
#38565 = CARTESIAN_POINT ( 'NONE',  ( 37.19234088328034460, -281.9607734364608973, -289.6918379650740007 ) ) ;
#38566 = CARTESIAN_POINT ( 'NONE',  ( -88.61290497509071429, -295.4198626974820172, -214.7873107050126862 ) ) ;
#38567 = CARTESIAN_POINT ( 'NONE',  ( -112.9978370375786199, -284.5680260334411855, -255.7607145945312084 ) ) ;
#38568 = CARTESIAN_POINT ( 'NONE',  ( 22.16304058319692061, -278.1513666033033019, -315.4280974550524093 ) ) ;
#38569 = CARTESIAN_POINT ( 'NONE',  ( -110.2690933549070849, -283.2325396760733724, -279.0904278785691304 ) ) ;
#38570 = CARTESIAN_POINT ( 'NONE',  ( 16.92253023958250679, -284.8245188364819569, -218.5136701463097211 ) ) ;
#38571 = CARTESIAN_POINT ( 'NONE',  ( -111.2841899529980481, -276.4818060341775094, -286.8781904642541463 ) ) ;
#38572 = CARTESIAN_POINT ( 'NONE',  ( -7.233842321018532751, -282.1539144287816043, -336.9443951218236748 ) ) ;
#38573 = CARTESIAN_POINT ( 'NONE',  ( -107.0641171735762782, -280.1663306701457259, -238.5033434644013255 ) ) ;
#38574 = CARTESIAN_POINT ( 'NONE',  ( 23.94709541931997521, -287.2283074292884635, -316.5834475868662139 ) ) ;
#38575 = CARTESIAN_POINT ( 'NONE',  ( 29.31681280234223408, -295.7430141291494010, -302.6448433069928683 ) ) ;
#38576 = CARTESIAN_POINT ( 'NONE',  ( -45.54304751212969649, -278.7544228478503214, -346.1709895120840201 ) ) ;
#38577 = CARTESIAN_POINT ( 'NONE',  ( -2.795305985376551838, -275.8143117622976206, -202.0834538698937877 ) ) ;
#38578 = CARTESIAN_POINT ( 'NONE',  ( -110.3511100643348186, -278.4178561801667229, -267.9061455862392336 ) ) ;
#38579 = CARTESIAN_POINT ( 'NONE',  ( -100.6893832978647367, -275.0649569870145683, -230.8779843866845738 ) ) ;
#38580 = CARTESIAN_POINT ( 'NONE',  ( 36.32199364678888998, -285.7215866698029458, -283.5402168862246981 ) ) ;
#38581 = CARTESIAN_POINT ( 'NONE',  ( -112.1435947867584275, -292.3367591503438234, -255.7631879635000587 ) ) ;
#38582 = CARTESIAN_POINT ( 'NONE',  ( 26.05310986494746572, -292.9754349837666609, -307.1758451841873807 ) ) ;
#38583 = ORIENTED_EDGE ( 'NONE', *, *, #3450, .F. ) ;
#38584 = CARTESIAN_POINT ( 'NONE',  ( 34.23805766763726410, -293.0284775758734099, -255.9241598278603078 ) ) ;
#38585 = ORIENTED_EDGE ( 'NONE', *, *, #3741, .F. ) ;
#38586 = CARTESIAN_POINT ( 'NONE',  ( -51.61424574545161903, -290.3102894950367272, -345.7122092189596856 ) ) ;
#38587 = CARTESIAN_POINT ( 'NONE',  ( -43.76830648553805503, -280.6203495924389699, -197.4919193750880595 ) ) ;
#38588 = CARTESIAN_POINT ( 'NONE',  ( -82.77634124440942287, -296.3678004105220225, -208.5117659198416220 ) ) ;
#38589 = CARTESIAN_POINT ( 'NONE',  ( 38.45497851479283469, -288.0401919739044843, -257.3154214071294064 ) ) ;
#38590 = CARTESIAN_POINT ( 'NONE',  ( -57.28132837293846080, -289.6357799515886313, -344.7677740555731134 ) ) ;
#38591 = CARTESIAN_POINT ( 'NONE',  ( -66.56413762178077320, -283.7790208351960928, -337.2935735189538491 ) ) ;
#38592 = CARTESIAN_POINT ( 'NONE',  ( -40.04897441875193209, -139.4172891677515622, -364.6093070308701272 ) ) ;
#38593 = CARTESIAN_POINT ( 'NONE',  ( -104.9560684206034011, -254.4573753784908376, -325.6091621043333362 ) ) ;
#38594 = CARTESIAN_POINT ( 'NONE',  ( -83.13117446773537722, -218.5196643677905968, -348.8949988116463032 ) ) ;
#38595 = CARTESIAN_POINT ( 'NONE',  ( -35.12295939574989490, -276.2207464307940654, -343.4889438559031873 ) ) ;
#38596 = CARTESIAN_POINT ( 'NONE',  ( -107.9121576436898380, -277.7343136329654953, -250.4642683499850193 ) ) ;
#38597 = CARTESIAN_POINT ( 'NONE',  ( -20.52033662665390423, -297.7651257057431735, -193.4240162007132824 ) ) ;
#38598 = CARTESIAN_POINT ( 'NONE',  ( 190.4953182115862376, 268.1230253924587146, -138.0059063792686516 ) ) ;
#38599 = CARTESIAN_POINT ( 'NONE',  ( -31.50471103718881949, -275.6648754719511203, -346.6972678698147661 ) ) ;
#38600 = VECTOR ( 'NONE', #88428, 1000.000000000000000 ) ;
#38601 = CARTESIAN_POINT ( 'NONE',  ( -107.7834588917727956, -290.7863070775582059, -289.9368497607976565 ) ) ;
#38602 = CARTESIAN_POINT ( 'NONE',  ( -35.84235262091186769, -298.8733041410477540, -193.5223946047195227 ) ) ;
#38603 = CARTESIAN_POINT ( 'NONE',  ( 35.44647769315002250, -286.3712344419290616, -280.6076267911944342 ) ) ;
#38604 = CARTESIAN_POINT ( 'NONE',  ( -110.9419918742206761, -273.4856394004074787, -247.9010192517368978 ) ) ;
#38605 = CARTESIAN_POINT ( 'NONE',  ( -63.56701120472439470, -295.5702629216104356, -338.5412712193190714 ) ) ;
#38606 = ORIENTED_EDGE ( 'NONE', *, *, #38392, .F. ) ;
#38607 = CARTESIAN_POINT ( 'NONE',  ( 197.9736226834741615, 68.21442376052006296, -9.114149584028082174 ) ) ;
#38608 = CARTESIAN_POINT ( 'NONE',  ( -68.40068826831367232, -279.3771157487001915, -339.2566956689610720 ) ) ;
#38609 = EDGE_CURVE ( 'NONE', #11817, #17165, #62610, .T. ) ;
#38610 = CARTESIAN_POINT ( 'NONE',  ( -27.38628060855530322, -282.4366715455404915, -346.7060905660006824 ) ) ;
#38611 = CARTESIAN_POINT ( 'NONE',  ( -105.5503977577082253, -279.2740471069772639, -297.2274471070107893 ) ) ;
#38612 = CARTESIAN_POINT ( 'NONE',  ( -111.7302058166181524, -280.5095439326133260, -254.7958839262545325 ) ) ;
#38613 = CARTESIAN_POINT ( 'NONE',  ( -110.5726122726317584, -271.1397352805959144, -262.1184692380630850 ) ) ;
#38614 = CARTESIAN_POINT ( 'NONE',  ( 18.83474343374798821, -281.0574907321378078, -223.7240476879092910 ) ) ;
#38615 = CARTESIAN_POINT ( 'NONE',  ( -60.83150259239849333, -274.5578704625709179, -197.1455853156062688 ) ) ;
#38616 = CARTESIAN_POINT ( 'NONE',  ( 1.363475323011903217, -276.5694342071035976, -206.1200871556967513 ) ) ;
#38617 = CARTESIAN_POINT ( 'NONE',  ( 36.31276330658904072, -274.3841859489003241, -290.7476668553790091 ) ) ;
#38618 = CARTESIAN_POINT ( 'NONE',  ( 175.2296996224750103, 160.0000000000000568, 10.55076157886938937 ) ) ;
#38619 = CARTESIAN_POINT ( 'NONE',  ( -107.9049296566723370, -290.0040694346157579, -251.0367197821137779 ) ) ;
#38620 = EDGE_CURVE ( 'NONE', #70265, #69489, #55792, .T. ) ;
#38621 = CARTESIAN_POINT ( 'NONE',  ( -85.44268468821064744, -284.7553845316572279, -210.3643841496721905 ) ) ;
#38622 = CARTESIAN_POINT ( 'NONE',  ( 32.02780294839854491, -279.4508296564083594, -244.4099689832119680 ) ) ;
#38624 = CARTESIAN_POINT ( 'NONE',  ( -92.57354282915400745, -283.3336680961187994, -220.3779152993751040 ) ) ;
#38623 = CARTESIAN_POINT ( 'NONE',  ( 0.7201297632527839943, -279.1447965278727565, -207.3206021567679613 ) ) ;
#38625 = CARTESIAN_POINT ( 'NONE',  ( 32.81139473946547724, -289.8985705205326440, -297.0293547073904392 ) ) ;
#38626 = CARTESIAN_POINT ( 'NONE',  ( -14.19814532920398698, -281.5640459856916209, -200.6546363802687836 ) ) ;
#38627 = CARTESIAN_POINT ( 'NONE',  ( 190.2832783574276903, 8.542400036368780647, -9.000000000000001776 ) ) ;
#38628 = CARTESIAN_POINT ( 'NONE',  ( 1.666915929396587615, -280.9395187050885170, -335.8192594806904481 ) ) ;
#38629 = CARTESIAN_POINT ( 'NONE',  ( -0.4212548499765729759, -296.5615698023182745, -335.6589921517457356 ) ) ;
#38630 = CARTESIAN_POINT ( 'NONE',  ( -101.0294958830999121, -277.3447172651430037, -228.8191301985502548 ) ) ;
#38631 = CARTESIAN_POINT ( 'NONE',  ( -106.3576983774112961, -278.8816436057744568, -294.6119849276227569 ) ) ;
#38632 = CARTESIAN_POINT ( 'NONE',  ( -111.6783332568231515, -286.6994352809491602, -258.8774037793710363 ) ) ;
#38633 = CARTESIAN_POINT ( 'NONE',  ( 165.0427047786672290, 250.5000000000000568, 23.37680765314704701 ) ) ;
#38634 = CARTESIAN_POINT ( 'NONE',  ( -44.78008781273001659, -293.8789889077572752, -195.1162027618132981 ) ) ;
#38635 = CARTESIAN_POINT ( 'NONE',  ( 13.07378181987813370, -274.3481182185060447, -325.9588569955002981 ) ) ;
#38636 = CARTESIAN_POINT ( 'NONE',  ( -70.57849786070354980, -288.6763976030566710, -339.6538109728577979 ) ) ;
#38637 = CARTESIAN_POINT ( 'NONE',  ( 0.3348002583417372113, -290.9629698883056790, -206.9030867035255312 ) ) ;
#38638 = CARTESIAN_POINT ( 'NONE',  ( -48.18343439339133027, -266.7963633758117794, -440.4292507800087719 ) ) ;
#38639 = CARTESIAN_POINT ( 'NONE',  ( -9.819120768379779207, -275.3698294393476544, -338.5198477838853819 ) ) ;
#38640 = CARTESIAN_POINT ( 'NONE',  ( -109.1706596917610312, -294.4477471526549834, -289.1588678978764619 ) ) ;
#38641 = CARTESIAN_POINT ( 'NONE',  ( -110.6128789897929323, -291.7844186261513073, -276.6889256733211937 ) ) ;
#38642 = CARTESIAN_POINT ( 'NONE',  ( 85.55100297371609486, -296.0521521680024080, -521.1711561948568487 ) ) ;
#38643 = DIRECTION ( 'NONE',  ( -1.000000000000000000, 0.000000000000000000, 0.000000000000000000 ) ) ;
#38644 = CARTESIAN_POINT ( 'NONE',  ( 24.26622432538682972, -291.4288702456225906, -225.3369977970235993 ) ) ;
#38645 = CARTESIAN_POINT ( 'NONE',  ( 30.16500051966891860, -289.5507427126352695, -300.3088815223756001 ) ) ;
#38646 = CARTESIAN_POINT ( 'NONE',  ( -70.22116375973402569, -287.7192440014742942, -338.8802677910119883 ) ) ;
#38647 = CARTESIAN_POINT ( 'NONE',  ( -4.346509843980319587, -287.9211802676148864, -204.5835204515061037 ) ) ;
#38648 = CARTESIAN_POINT ( 'NONE',  ( 22.88863428956209489, -288.9323752687214437, -311.9152228436436758 ) ) ;
#38649 = CARTESIAN_POINT ( 'NONE',  ( -44.61130307516486937, -297.1234672522799656, -345.4171139492346470 ) ) ;
#38650 = DIRECTION ( 'NONE',  ( -1.000000000000000000, 0.000000000000000000, 0.000000000000000000 ) ) ;
#38651 = CARTESIAN_POINT ( 'NONE',  ( 37.12207665703658677, -288.9838700175615145, -288.3930817483354190 ) ) ;
#38652 = CARTESIAN_POINT ( 'NONE',  ( -106.2726687366604637, -276.2277571832603940, -301.4374477890178241 ) ) ;
#38653 = CARTESIAN_POINT ( 'NONE',  ( -113.2776127247878435, -278.7274505345936859, -282.9897152781234126 ) ) ;
#38654 = CARTESIAN_POINT ( 'NONE',  ( -11.51245073006420583, -280.0461568319328762, -197.7889850670143517 ) ) ;
#38655 = CARTESIAN_POINT ( 'NONE',  ( -80.70355945091367289, -299.4405467869611357, -209.6026127663645582 ) ) ;
#38656 = CARTESIAN_POINT ( 'NONE',  ( -30.31933086257789611, -284.1406878904389828, -195.6384040962100244 ) ) ;
#38657 = CARTESIAN_POINT ( 'NONE',  ( -110.3467704370464162, -272.3479781978851975, -270.3585183588572818 ) ) ;
#38658 = CARTESIAN_POINT ( 'NONE',  ( -90.33908292914283322, -277.4323932189788025, -218.3061529871104369 ) ) ;
#38659 = CARTESIAN_POINT ( 'NONE',  ( -44.26075426774872312, -281.1393677263657196, -345.0932572550127020 ) ) ;
#38660 = LINE ( 'NONE', #45749, #69949 ) ;
#38661 = CARTESIAN_POINT ( 'NONE',  ( 36.21208490114274525, -274.2893516052154723, -290.7210815904421679 ) ) ;
#38662 = CARTESIAN_POINT ( 'NONE',  ( -107.3716679629555273, -298.3758536211280443, -247.2533725726121361 ) ) ;
#38663 = CARTESIAN_POINT ( 'NONE',  ( 30.79618817293042454, -280.9280018609353533, -305.5565819910685263 ) ) ;
#38664 = CARTESIAN_POINT ( 'NONE',  ( -65.67477836797526436, -298.6135027230203605, -202.8285693414526065 ) ) ;
#38665 = CARTESIAN_POINT ( 'NONE',  ( -111.1120349551615476, -297.6116580182963389, -290.6400719286995127 ) ) ;
#38666 = CARTESIAN_POINT ( 'NONE',  ( -76.57201217955358175, -273.1779267779495513, -208.7732124890071930 ) ) ;
#38667 = CARTESIAN_POINT ( 'NONE',  ( 35.05375967640134149, -295.8047943575637078, -290.0033275576636242 ) ) ;
#38668 = CARTESIAN_POINT ( 'NONE',  ( 7.542208665356192832, -286.8121861495543499, -207.7300053287800097 ) ) ;
#38669 = CARTESIAN_POINT ( 'NONE',  ( -87.94853297784503354, -277.4307384113761827, -214.2517367298578108 ) ) ;
#38670 = CARTESIAN_POINT ( 'NONE',  ( -87.38604648872859570, -289.5607974249431891, -328.9509221560660990 ) ) ;
#38671 = CARTESIAN_POINT ( 'NONE',  ( -72.48226097449756367, -288.5882362391677134, -334.6149072242307057 ) ) ;
#38672 = CARTESIAN_POINT ( 'NONE',  ( 16.08330946055215449, -290.8091783401737871, -217.6498664896715241 ) ) ;
#38673 = VERTEX_POINT ( 'NONE', #53914 ) ;
#38674 = CARTESIAN_POINT ( 'NONE',  ( -110.5532707284312579, -275.4615312476335589, -297.1751512281608143 ) ) ;
#38675 = CARTESIAN_POINT ( 'NONE',  ( -8.199706663469738643, -288.1677005902176916, -337.4132053195290837 ) ) ;
#38676 = CARTESIAN_POINT ( 'NONE',  ( 209.6287663260176259, 29.00782453271233408, 12.09245862095555601 ) ) ;
#38677 = CARTESIAN_POINT ( 'NONE',  ( -103.8426355183811864, -285.9946138933723319, -231.9089900136957567 ) ) ;
#38678 = CARTESIAN_POINT ( 'NONE',  ( -7.271291010711933289, -291.4957559357231389, -199.7168827661001274 ) ) ;
#38679 = CARTESIAN_POINT ( 'NONE',  ( 38.38554519050750002, -283.0044473123373336, -281.2552718805810059 ) ) ;
#38680 = CARTESIAN_POINT ( 'NONE',  ( -95.92301247436604683, -283.7745094956986804, -313.9183200083140832 ) ) ;
#38681 = CARTESIAN_POINT ( 'NONE',  ( -113.7747802549455542, -296.6687933634794945, -261.0345825958070236 ) ) ;
#38682 = CARTESIAN_POINT ( 'NONE',  ( 24.19734696805935315, -276.3143142766277833, -230.1841449704854767 ) ) ;
#38683 = CARTESIAN_POINT ( 'NONE',  ( 35.83380259722154193, -291.3821328833099074, -255.6236620708110081 ) ) ;
#38684 = CARTESIAN_POINT ( 'NONE',  ( 23.38946471719789955, -273.7767295388932780, -229.1213853654839738 ) ) ;
#38685 = VERTEX_POINT ( 'NONE', #91274 ) ;
#38686 = LINE ( 'NONE', #54757, #22905 ) ;
#38687 = CARTESIAN_POINT ( 'NONE',  ( -86.69887201954509237, -287.2802636248009662, -214.5680261316118447 ) ) ;
#38688 = CARTESIAN_POINT ( 'NONE',  ( -74.44471193628359629, -296.6129916539582041, -337.5388327397262174 ) ) ;
#38689 = CARTESIAN_POINT ( 'NONE',  ( -106.2670671519107373, -284.8780962609328640, -294.8672251754564968 ) ) ;
#38690 = CARTESIAN_POINT ( 'NONE',  ( 37.94924438709335845, -274.7986959810210692, -285.3308837687211508 ) ) ;
#38691 = CARTESIAN_POINT ( 'NONE',  ( -7.237762732274443778, -293.0881638256530550, -199.5861932270677528 ) ) ;
#38692 = CARTESIAN_POINT ( 'NONE',  ( 23.72202852916559124, -285.0863190528654627, -225.5110731105860111 ) ) ;
#38693 = CARTESIAN_POINT ( 'NONE',  ( 38.33724818304983017, -294.0625476862454661, -284.5192739322165494 ) ) ;
#38694 = CARTESIAN_POINT ( 'NONE',  ( -106.0510309508754290, -290.5562900909282575, -295.0818652329948009 ) ) ;
#38695 = DIRECTION ( 'NONE',  ( -0.000000000000000000, -1.000000000000000000, -0.000000000000000000 ) ) ;
#38696 = DIRECTION ( 'NONE',  ( -0.000000000000000000, -1.000000000000000000, -0.000000000000000000 ) ) ;
#38697 = CARTESIAN_POINT ( 'NONE',  ( -47.07807668347071939, -155.4490103796987626, -361.3962506754892843 ) ) ;
#38698 = CARTESIAN_POINT ( 'NONE',  ( -111.5403815227015087, -285.8467827904743785, -288.2282632799791600 ) ) ;
#38699 = CARTESIAN_POINT ( 'NONE',  ( -2.602324593224659921, -271.9809262143061233, -198.2974183793908196 ) ) ;
#38700 = VERTEX_POINT ( 'NONE', #34482 ) ;
#38701 = CARTESIAN_POINT ( 'NONE',  ( -97.79501939187794335, -282.8966276932354162, -311.9179422820130867 ) ) ;
#38702 = CARTESIAN_POINT ( 'NONE',  ( -114.0584231396461945, -278.1317557054591134, -277.3249408792123063 ) ) ;
#38703 = CARTESIAN_POINT ( 'NONE',  ( 17.17859992772618583, -284.2728057876785215, -321.6956901318080781 ) ) ;
#38704 = CARTESIAN_POINT ( 'NONE',  ( -45.94015373935981472, -156.1293870317898893, -363.6621071055034804 ) ) ;
#38705 = CARTESIAN_POINT ( 'NONE',  ( -50.01380106442190510, -281.7853987947431733, -345.7672475420787919 ) ) ;
#38706 = CARTESIAN_POINT ( 'NONE',  ( 36.75393891632501209, -285.6888538904835286, -279.3989870114871223 ) ) ;
#38707 = CARTESIAN_POINT ( 'NONE',  ( -85.04911771501511453, -275.2620658605604831, -211.5027474227059372 ) ) ;
#38708 = CARTESIAN_POINT ( 'NONE',  ( -70.95353362183402623, -296.0005070196287988, -335.2460091929279997 ) ) ;
#38709 = CARTESIAN_POINT ( 'NONE',  ( -37.53454268933070637, -290.7345485004443617, -196.8556903180865163 ) ) ;
#38710 = CARTESIAN_POINT ( 'NONE',  ( -103.3283961143731489, -279.7202660643321224, -230.7725192632215681 ) ) ;
#38711 = CARTESIAN_POINT ( 'NONE',  ( -8.738677133535908581, -276.6671966870574693, -337.5376493299509093 ) ) ;
#38712 = CARTESIAN_POINT ( 'NONE',  ( 38.82888932785649416, -274.5900494434139318, -279.7238603916275679 ) ) ;
#38713 = DIRECTION ( 'NONE',  ( 1.000000000000000000, 0.000000000000000000, -0.000000000000000000 ) ) ;
#38714 = CARTESIAN_POINT ( 'NONE',  ( 35.97090622290477313, -273.7558361698543195, -286.2401664282711522 ) ) ;
#38715 = CARTESIAN_POINT ( 'NONE',  ( 31.70542278211600262, -295.4014500383208315, -303.2122022881757744 ) ) ;
#38716 = ADVANCED_FACE ( 'NONE', ( #3732 ), #86777, .T. ) ;
#38717 = DIRECTION ( 'NONE',  ( 1.110223024625155531E-13, 0.000000000000000000, 1.000000000000000000 ) ) ;
#38718 = FACE_OUTER_BOUND ( 'NONE', #83972, .T. ) ;
#38719 = CARTESIAN_POINT ( 'NONE',  ( -78.53903684522647666, -284.7011510993472712, -330.9994352447401411 ) ) ;
#38720 = CARTESIAN_POINT ( 'NONE',  ( -38.69176861510950971, -284.8290019289717065, -346.3357935782334494 ) ) ;
#38721 = CARTESIAN_POINT ( 'NONE',  ( -19.78335102989808902, -285.6325094345863818, -199.3991771637086003 ) ) ;
#38722 = CARTESIAN_POINT ( 'NONE',  ( 29.87460138361937823, -274.3582520091341621, -300.8309263861464160 ) ) ;
#38723 = CARTESIAN_POINT ( 'NONE',  ( 35.70506315066613467, -283.5851191530240953, -283.6625824098250632 ) ) ;
#38724 = CARTESIAN_POINT ( 'NONE',  ( -24.22503359630115582, -275.3616467007357755, -342.9296799161996319 ) ) ;
#38725 = CARTESIAN_POINT ( 'NONE',  ( -13.67264448623344641, -277.8173867107839214, -339.7974934417040913 ) ) ;
#38726 = CARTESIAN_POINT ( 'NONE',  ( 121.3395553409046528, -299.5541904835127980, -198.8526868767648352 ) ) ;
#38727 = VECTOR ( 'NONE', #83179, 1000.000000000000227 ) ;
#38728 = CARTESIAN_POINT ( 'NONE',  ( -11.57315864699415542, -281.1820874616586252, -197.9164376734674704 ) ) ;
#38729 = CARTESIAN_POINT ( 'NONE',  ( -39.59174666557483846, -280.5169852378463133, -193.4425240798844072 ) ) ;
#38730 = ORIENTED_EDGE ( 'NONE', *, *, #69429, .F. ) ;
#38731 = ORIENTED_EDGE ( 'NONE', *, *, #30742, .T. ) ;
#38732 = CARTESIAN_POINT ( 'NONE',  ( 195.4937503561064887, 41.24039232090726870, 14.64184794398896194 ) ) ;
#38733 = CARTESIAN_POINT ( 'NONE',  ( 35.49703938673690828, -289.1447596469518544, -249.3226175423496898 ) ) ;
#38734 = CARTESIAN_POINT ( 'NONE',  ( -84.17036566300784273, -296.5863989790245228, -214.0839696217804828 ) ) ;
#38735 = EDGE_CURVE ( 'NONE', #70988, #54449, #25493, .T. ) ;
#38736 = CARTESIAN_POINT ( 'NONE',  ( -97.37877477793637127, -290.5452482676105888, -222.3104941083730637 ) ) ;
#38737 = CARTESIAN_POINT ( 'NONE',  ( 36.37445050113649359, -286.0052496041078598, -268.3123165637961733 ) ) ;
#38739 = CARTESIAN_POINT ( 'NONE',  ( -95.90260588986973289, -289.4205672298264744, -225.0997179538059640 ) ) ;
#38738 = CARTESIAN_POINT ( 'NONE',  ( -39.99741367048822127, -287.6607675278536931, -343.9523932668482757 ) ) ;
#38740 = CARTESIAN_POINT ( 'NONE',  ( -87.97948325793061031, -286.5295761286000698, -217.2297202608392865 ) ) ;
#38741 = CARTESIAN_POINT ( 'NONE',  ( -89.94493109208984549, -275.7943569993038864, -323.8932079826837480 ) ) ;
#38742 = CARTESIAN_POINT ( 'NONE',  ( 23.49111873604502776, -286.5695375880597453, -316.2502078246037627 ) ) ;
#38743 = CARTESIAN_POINT ( 'NONE',  ( 32.00032400169781255, -289.1778863366087080, -241.6478666014458270 ) ) ;
#38744 = CARTESIAN_POINT ( 'NONE',  ( -6.404888942851536093, -286.6465964779599744, -338.8661699398362543 ) ) ;
#38745 = EDGE_CURVE ( 'NONE', #30715, #26935, #53535, .T. ) ;
#38746 = CARTESIAN_POINT ( 'NONE',  ( 34.71911799381504693, -282.6661037326872474, -283.4946402849566311 ) ) ;
#38747 = CARTESIAN_POINT ( 'NONE',  ( -109.7684818101180610, -292.2942188605396723, -290.4705616292967534 ) ) ;
#38748 = CARTESIAN_POINT ( 'NONE',  ( 197.1098461824585968, 214.8820409514499090, -12.42446933126073816 ) ) ;
#38749 = CARTESIAN_POINT ( 'NONE',  ( 155.8658175007533657, 19.96629232096022122, -14.32310887264409160 ) ) ;
#38750 = CARTESIAN_POINT ( 'NONE',  ( -54.29627683302920360, -299.7561801430052810, -196.7278610676924302 ) ) ;
#38751 = CARTESIAN_POINT ( 'NONE',  ( 5.024963202835075471, -279.8386635464007099, -210.7149314764068890 ) ) ;
#38752 = CARTESIAN_POINT ( 'NONE',  ( 35.88783707607991147, -279.7599993690577094, -286.5609801482431180 ) ) ;
#38753 = CARTESIAN_POINT ( 'NONE',  ( 24.74974782781754001, -293.3516067526378492, -315.6470700573532895 ) ) ;
#38754 = CARTESIAN_POINT ( 'NONE',  ( -44.62801135734449787, -296.3584260429999517, -196.8707527219877704 ) ) ;
#38755 = CARTESIAN_POINT ( 'NONE',  ( -8.196989202679366926, -274.7473528729238978, -338.8723705916961535 ) ) ;
#38756 = CARTESIAN_POINT ( 'NONE',  ( -58.53454759373760652, -296.6471662342117952, -340.7323244043890895 ) ) ;
#38757 = CARTESIAN_POINT ( 'NONE',  ( 208.4306832106270804, -124.2391364535881024, -6.500000000000024869 ) ) ;
#38758 = CARTESIAN_POINT ( 'NONE',  ( -71.12582338760221035, -272.1896853246867636, -201.8247093305806743 ) ) ;
#38759 = CARTESIAN_POINT ( 'NONE',  ( -112.3852040423190175, -294.9443124747785419, -258.3437437178201890 ) ) ;
#38760 = CARTESIAN_POINT ( 'NONE',  ( 11.30684363273117299, -294.1669617081450951, -215.0781558697165963 ) ) ;
#38761 = CARTESIAN_POINT ( 'NONE',  ( 29.33919985515026596, -212.1443419142231051, 25.50000000000000000 ) ) ;
#38762 = CARTESIAN_POINT ( 'NONE',  ( -7.213068811878641462, -293.2606274030360964, -203.6912799562599616 ) ) ;
#38763 = DIRECTION ( 'NONE',  ( -0.6056179655966478226, 0.7957555401921982963, -0.000000000000000000 ) ) ;
#38765 = CARTESIAN_POINT ( 'NONE',  ( -20.84817480361739683, -294.8346421280153322, -341.5255537009674072 ) ) ;
#38764 = CARTESIAN_POINT ( 'NONE',  ( -95.02781199097549347, -281.9050084632482367, -318.8653086749613408 ) ) ;
#38766 = CARTESIAN_POINT ( 'NONE',  ( -18.91839532270654090, -282.8214490829483339, -345.1795817661326851 ) ) ;
#38767 = CARTESIAN_POINT ( 'NONE',  ( 12.03239917661917069, -282.6526394970497904, -213.1639807011012238 ) ) ;
#38768 = CARTESIAN_POINT ( 'NONE',  ( -36.56138241309975001, -285.7284152807337136, -193.3731814531014379 ) ) ;
#38769 = CARTESIAN_POINT ( 'NONE',  ( -104.0321345044617658, -289.0031135123950889, -236.2992576045764679 ) ) ;
#38770 = CARTESIAN_POINT ( 'NONE',  ( 30.45221852812324315, -280.4876221868914286, -305.3852859837128904 ) ) ;
#38771 = CARTESIAN_POINT ( 'NONE',  ( 9.356661063313353566, -285.3946019829459146, -213.6116110365334748 ) ) ;
#38772 = CARTESIAN_POINT ( 'NONE',  ( -15.05526900853502070, -287.6905604449424914, -343.7978897630304118 ) ) ;
#38773 = LINE ( 'NONE', #74782, #49145 ) ;
#38774 = CARTESIAN_POINT ( 'NONE',  ( -82.83714306084179668, -297.2859992475754325, -328.5348221971021871 ) ) ;
#38775 = CARTESIAN_POINT ( 'NONE',  ( -82.18570005214883167, -279.0760004505090137, -332.2288960437002174 ) ) ;
#38777 = CARTESIAN_POINT ( 'NONE',  ( -43.74871671564858389, -279.6358140187750223, -197.5713504666764209 ) ) ;
#38776 = CARTESIAN_POINT ( 'NONE',  ( -11.64237395522665963, -292.7393832104152693, -341.2539716593892649 ) ) ;
#38778 = CARTESIAN_POINT ( 'NONE',  ( 33.32355502936599123, -293.3290886519993137, -239.7764532301270890 ) ) ;
#38779 = CARTESIAN_POINT ( 'NONE',  ( -110.9512616473154907, -282.8493949467728044, -253.3039594950243725 ) ) ;
#38780 = CARTESIAN_POINT ( 'NONE',  ( -41.25396738523028262, -279.1015408230006187, -345.2718797789061682 ) ) ;
#38781 = CARTESIAN_POINT ( 'NONE',  ( -18.17041146242248928, -293.8576538703090932, -341.0425875367765798 ) ) ;
#38782 = CARTESIAN_POINT ( 'NONE',  ( -69.83879782982727136, -295.6240379137856280, -202.7671885601548638 ) ) ;
#38783 = ORIENTED_EDGE ( 'NONE', *, *, #15328, .T. ) ;
#38784 = FACE_OUTER_BOUND ( 'NONE', #80838, .T. ) ;
#38785 = CARTESIAN_POINT ( 'NONE',  ( 36.33091610447689135, -283.6869611531528790, -282.3691328587689213 ) ) ;
#38786 = CARTESIAN_POINT ( 'NONE',  ( -109.4246530689027566, -295.9027183941707335, -282.2790178427223964 ) ) ;
#38787 = DIRECTION ( 'NONE',  ( 0.000000000000000000, -0.000000000000000000, 1.000000000000000000 ) ) ;
#38788 = CARTESIAN_POINT ( 'NONE',  ( -95.95921662488163406, -270.6952119285918457, -223.5744983911110353 ) ) ;
#38789 = CARTESIAN_POINT ( 'NONE',  ( 98.67988849359637982, -298.7747639397677517, -193.6174340023339369 ) ) ;
#38790 = CARTESIAN_POINT ( 'NONE',  ( 36.21242324690683034, -288.5996057745439884, -249.1234694261997049 ) ) ;
#38791 = CARTESIAN_POINT ( 'NONE',  ( -72.36072668084190695, -289.3626830585199627, -334.4131888609855991 ) ) ;
#38792 = CARTESIAN_POINT ( 'NONE',  ( -105.0869751600894659, -280.4582392001921107, -241.3561966493277282 ) ) ;
#38793 = CARTESIAN_POINT ( 'NONE',  ( -47.43278820255034844, -299.6824456453469452, -196.9870020056213207 ) ) ;
#38794 = CARTESIAN_POINT ( 'NONE',  ( -51.89114037787017963, -278.6568620729844952, -198.3685471001835765 ) ) ;
#38795 = ORIENTED_EDGE ( 'NONE', *, *, #92638, .F. ) ;
#38796 = CARTESIAN_POINT ( 'NONE',  ( -14.81354312561614783, -297.9937060428184168, -193.3834923250184090 ) ) ;
#38797 = CARTESIAN_POINT ( 'NONE',  ( -47.20907965767397485, -293.8459718442173312, -196.5779964881937190 ) ) ;
#38798 = CARTESIAN_POINT ( 'NONE',  ( 175.2296996224750103, 250.0000000000000568, 0.000000000000000000 ) ) ;
#38799 = ADVANCED_FACE ( 'NONE', ( #48191 ), #41556, .T. ) ;
#38800 = CARTESIAN_POINT ( 'NONE',  ( -75.91549562676297569, -290.2336861823890786, -332.4574541783235304 ) ) ;
#38801 = FACE_OUTER_BOUND ( 'NONE', #24373, .T. ) ;
#38802 = CARTESIAN_POINT ( 'NONE',  ( 23.83137965190389096, -291.0886312732263264, -225.6603373111316273 ) ) ;
#38803 = CARTESIAN_POINT ( 'NONE',  ( -98.46294381318374178, -296.7735133423636853, -230.3161378687463809 ) ) ;
#38804 = DIRECTION ( 'NONE',  ( -0.000000000000000000, -1.000000000000000000, 0.000000000000000000 ) ) ;
#38805 = CARTESIAN_POINT ( 'NONE',  ( -111.5835760717182694, -291.8490584600560283, -288.0479520807988365 ) ) ;
#38806 = CARTESIAN_POINT ( 'NONE',  ( -99.90806341382572953, -287.6948066931273047, -220.5068182859052968 ) ) ;
#38807 = CARTESIAN_POINT ( 'NONE',  ( 36.94720901235586297, -289.6682648504477129, -279.3714678376840084 ) ) ;
#38808 = CARTESIAN_POINT ( 'NONE',  ( 32.97593397404876470, -273.8865216925588584, -296.1134837117195957 ) ) ;
#38809 = CARTESIAN_POINT ( 'NONE',  ( 36.81036916302631568, -277.3804418757688381, -263.2595170955654567 ) ) ;
#38810 = CARTESIAN_POINT ( 'NONE',  ( -4.169845387424268246, -290.5727406007346190, -203.7065217159041310 ) ) ;
#38811 = CARTESIAN_POINT ( 'NONE',  ( -94.05320953328877920, -281.1042910461220572, -220.1205946689422603 ) ) ;
#38812 = ORIENTED_EDGE ( 'NONE', *, *, #64104, .F. ) ;
#38813 = CARTESIAN_POINT ( 'NONE',  ( -56.35339028472269263, -282.6522753933383001, -340.9475777694492535 ) ) ;
#38814 = CARTESIAN_POINT ( 'NONE',  ( -84.66479131761597898, -278.7662605811159438, -330.7777176819421356 ) ) ;
#38815 = CARTESIAN_POINT ( 'NONE',  ( 13.40619459087050203, -281.1557541020961253, -327.8134145612160637 ) ) ;
#38816 = CARTESIAN_POINT ( 'NONE',  ( 31.03526160566912040, -276.0426467268437705, -235.4696961664207322 ) ) ;
#38817 = PRODUCT_CONTEXT ( 'NONE', #83158, 'mechanical' ) ;
#38818 = CARTESIAN_POINT ( 'NONE',  ( -38.36768189626314296, -275.5596251077748775, -194.0613465760981740 ) ) ;
#38819 = CARTESIAN_POINT ( 'NONE',  ( -67.68488546085839630, -279.9805209788415823, -333.4427485647536855 ) ) ;
#38820 = ORIENTED_EDGE ( 'NONE', *, *, #9944, .F. ) ;
#38821 = CARTESIAN_POINT ( 'NONE',  ( -106.8049319824969956, -298.1835524501046280, -298.6429154254506102 ) ) ;
#38822 = CARTESIAN_POINT ( 'NONE',  ( -108.0201540150592905, -291.3735363975515611, -290.0103841145019601 ) ) ;
#38823 = CARTESIAN_POINT ( 'NONE',  ( -57.00675063579810598, -291.0624103628849753, -343.8134480378828357 ) ) ;
#38824 = CARTESIAN_POINT ( 'NONE',  ( -55.02900067885569513, -291.1672101448540388, -199.4312084446210633 ) ) ;
#38825 = CARTESIAN_POINT ( 'NONE',  ( -91.85496449419646581, -284.8071997122972903, -216.0671872784213576 ) ) ;
#38826 = CYLINDRICAL_SURFACE ( 'NONE', #91430, 9.103929867429224387 ) ;
#38827 = CARTESIAN_POINT ( 'NONE',  ( 8.272607584459853669, -280.8163346047826963, -328.4416725878276679 ) ) ;
#38828 = CARTESIAN_POINT ( 'NONE',  ( 1.985699335745167327, -290.3800937224756922, -333.3231790262706227 ) ) ;
#38829 = CARTESIAN_POINT ( 'NONE',  ( -64.32711367824913395, -281.8907011518411423, -338.9358597490014517 ) ) ;
#38830 = CARTESIAN_POINT ( 'NONE',  ( 35.84177963000056621, -282.7720054275216626, -263.0859850048537396 ) ) ;
#38831 = CARTESIAN_POINT ( 'NONE',  ( 33.82870509269117321, -288.8613445592978906, -299.2706865993270071 ) ) ;
#38832 = CARTESIAN_POINT ( 'NONE',  ( -76.86041000289702652, -279.9999044749450832, -208.8495236173278329 ) ) ;
#38833 = CARTESIAN_POINT ( 'NONE',  ( 21.91192499489778100, -291.6917885894774258, -221.8120023364671169 ) ) ;
#38834 = CARTESIAN_POINT ( 'NONE',  ( 29.98513318908628023, -287.8731388192978784, -233.2202653767533320 ) ) ;
#38835 = CARTESIAN_POINT ( 'NONE',  ( -49.34132053080093527, -286.3955993419867241, -194.3104772342489355 ) ) ;
#38836 = CARTESIAN_POINT ( 'NONE',  ( -95.11513802396738981, -284.0903345210262501, -315.0047211613770628 ) ) ;
#38837 = ORIENTED_EDGE ( 'NONE', *, *, #58308, .T. ) ;
#38838 = VECTOR ( 'NONE', #84692, 1000.000000000000000 ) ;
#38839 = CARTESIAN_POINT ( 'NONE',  ( 20.35418469003431952, -294.7394456007099848, -221.2343779958318351 ) ) ;
#38840 = CARTESIAN_POINT ( 'NONE',  ( 37.58239763731098293, -292.0413089025782938, -254.8153091839437252 ) ) ;
#38841 = CARTESIAN_POINT ( 'NONE',  ( -56.67378824133316328, -276.3661706069784714, -341.0514464796813172 ) ) ;
#38842 = CARTESIAN_POINT ( 'NONE',  ( -23.37448629464264016, -297.5713107977072696, -193.4645463883891523 ) ) ;
#38843 = CARTESIAN_POINT ( 'NONE',  ( 21.55952134324993708, -291.4160008093153920, -226.0739430527690104 ) ) ;
#38844 = CARTESIAN_POINT ( 'NONE',  ( -99.28351402288689087, -295.3468833874654820, -229.7568633292858635 ) ) ;
#38845 = CARTESIAN_POINT ( 'NONE',  ( -12.13819365048166432, -293.5924916550139869, -201.3728256543343775 ) ) ;
#38846 = CARTESIAN_POINT ( 'NONE',  ( 6.851689802359501869, -293.7495103260690712, -211.8703464102424618 ) ) ;
#38847 = CARTESIAN_POINT ( 'NONE',  ( -6.572041688988396579, -292.6488985891979837, -338.9414107010813382 ) ) ;
#38848 = CARTESIAN_POINT ( 'NONE',  ( 219.7099725226080977, -147.7221692137691775, -1.978481845683818907 ) ) ;
#38849 = CARTESIAN_POINT ( 'NONE',  ( 1.446330167486975293, -289.4610779507010534, -332.4811401472002785 ) ) ;
#38850 = CARTESIAN_POINT ( 'NONE',  ( -68.31574903800111542, -279.4368442109777675, -339.0703002293935810 ) ) ;
#38851 = CARTESIAN_POINT ( 'NONE',  ( -35.73530157983303468, -275.8273832322307157, -346.9602576719697140 ) ) ;
#38852 = EDGE_CURVE ( 'NONE', #30831, #783, #18722, .T. ) ;
#38853 = CARTESIAN_POINT ( 'NONE',  ( -90.08690079926110172, -272.6789446726293704, -214.3307775404495032 ) ) ;
#38854 = CARTESIAN_POINT ( 'NONE',  ( 35.34123567665463383, -279.8399928478545462, -286.4392100515612469 ) ) ;
#38855 = CARTESIAN_POINT ( 'NONE',  ( -64.82574785959964458, -275.8049203512368308, -341.4876891502080412 ) ) ;
#38856 = EDGE_CURVE ( 'NONE', #64501, #55580, #42927, .T. ) ;
#38857 = CARTESIAN_POINT ( 'NONE',  ( -88.85940884276104157, -294.4788143193874816, -322.8460981224324087 ) ) ;
#38858 = CARTESIAN_POINT ( 'NONE',  ( 159.4851178187871312, 17.02694846567612075, 9.999999999999998224 ) ) ;
#38859 = CARTESIAN_POINT ( 'NONE',  ( -105.5143021396919352, -273.5573520494992295, -243.8322591845377758 ) ) ;
#38860 = CARTESIAN_POINT ( 'NONE',  ( 194.2870706637141325, 27.48493576247232184, 14.58823529411763431 ) ) ;
#38862 = CARTESIAN_POINT ( 'NONE',  ( -4.102791441679141116, -274.3364638657860155, -205.3534317641578753 ) ) ;
#38861 = CARTESIAN_POINT ( 'NONE',  ( -105.0470168024887982, -288.1368325642215495, -303.5614767484809704 ) ) ;
#38863 = CARTESIAN_POINT ( 'NONE',  ( -8.233132333283057491, -288.6813746547723554, -341.6613665754782687 ) ) ;
#38864 = CARTESIAN_POINT ( 'NONE',  ( -111.2699889068196057, -274.7299603236163534, -256.4946206855208857 ) ) ;
#38865 = CARTESIAN_POINT ( 'NONE',  ( -98.36330645575226583, -295.1420787051656589, -227.0437774687291324 ) ) ;
#38866 = CARTESIAN_POINT ( 'NONE',  ( -37.32457320118455613, -282.2490785764852603, -347.2126780741660923 ) ) ;
#38867 = DIRECTION ( 'NONE',  ( 0.000000000000000000, 0.000000000000000000, -1.000000000000000000 ) ) ;
#38868 = CARTESIAN_POINT ( 'NONE',  ( -78.41963187038422234, -281.6043709599552471, -333.1727363578929157 ) ) ;
#38869 = CARTESIAN_POINT ( 'NONE',  ( 208.4306832106270804, -125.2391364535880882, 0.000000000000000000 ) ) ;
#38870 = CARTESIAN_POINT ( 'NONE',  ( -91.95842277358480032, -290.0452186496872287, -221.3102519504354575 ) ) ;
#38871 = CARTESIAN_POINT ( 'NONE',  ( -34.82805275105177145, -281.1598582553121446, -344.5664000865866115 ) ) ;
#38872 = CARTESIAN_POINT ( 'NONE',  ( 221.8344101925596306, 1.000000000000000222, -7.000000000000000888 ) ) ;
#38873 = CARTESIAN_POINT ( 'NONE',  ( -101.4071529614679150, -289.0747590817246078, -231.3660105916091254 ) ) ;
#38874 = CARTESIAN_POINT ( 'NONE',  ( -83.64107105132380582, -274.9235214554420850, -213.0280908289012416 ) ) ;
#38875 = CARTESIAN_POINT ( 'NONE',  ( -34.47836883863266166, -284.2219802332732002, -346.9105141488691402 ) ) ;
#38877 = CARTESIAN_POINT ( 'NONE',  ( -71.40888074852966838, -283.5153415121228022, -334.9244760471290761 ) ) ;
#38876 = CARTESIAN_POINT ( 'NONE',  ( -70.74381144164148338, -271.6948836715877746, -202.5849189003282333 ) ) ;
#38878 = CARTESIAN_POINT ( 'NONE',  ( 34.94896151333151835, -276.7973176353905274, -256.5975734602923808 ) ) ;
#38879 = CARTESIAN_POINT ( 'NONE',  ( -4.985487101250802411, -277.4177748106638433, -335.9926991493922515 ) ) ;
#38880 = CARTESIAN_POINT ( 'NONE',  ( -69.58654837798279402, -285.4766549964556361, -338.0898269894869941 ) ) ;
#38881 = ORIENTED_EDGE ( 'NONE', *, *, #34457, .T. ) ;
#38882 = CARTESIAN_POINT ( 'NONE',  ( -111.5368827832384255, -270.7108482962777316, -270.3376737736280120 ) ) ;
#38883 = CARTESIAN_POINT ( 'NONE',  ( 11.19666648565100786, -294.2346486981763860, -330.2046296897908633 ) ) ;
#38884 = CARTESIAN_POINT ( 'NONE',  ( -8.889260789513871330, -288.4060450473700143, -201.3378485982815675 ) ) ;
#38885 = DIRECTION ( 'NONE',  ( -0.000000000000000000, 1.000000000000000000, -0.000000000000000000 ) ) ;
#38886 = CARTESIAN_POINT ( 'NONE',  ( -99.90806341382575795, -287.4094976428775112, -320.2154176792147382 ) ) ;
#38887 = CARTESIAN_POINT ( 'NONE',  ( -48.06191697002892482, -278.8392922549081732, -194.3695591657247803 ) ) ;
#38888 = CARTESIAN_POINT ( 'NONE',  ( -96.82614518502526835, -289.5966867193443477, -222.7371616665716374 ) ) ;
#38889 = CARTESIAN_POINT ( 'NONE',  ( -49.55532178199268856, -287.4138687008414195, -197.6349567661305002 ) ) ;
#38890 = CARTESIAN_POINT ( 'NONE',  ( -4.597880586798756219, -278.3749284970634790, -336.7515262305816464 ) ) ;
#38891 = CARTESIAN_POINT ( 'NONE',  ( -98.88057810649675616, -286.5847806301068204, -224.9797424687994862 ) ) ;
#38892 = CARTESIAN_POINT ( 'NONE',  ( 37.42496333949119247, -283.6362855124600628, -276.9008602133670820 ) ) ;
#38893 = CARTESIAN_POINT ( 'NONE',  ( 39.13784383678476075, -275.8361999596876331, -279.7457900415583936 ) ) ;
#38894 = CARTESIAN_POINT ( 'NONE',  ( -112.1750334612222417, -270.5523135732584024, -270.3357091355649118 ) ) ;
#38895 = CARTESIAN_POINT ( 'NONE',  ( -114.2321197488982563, -278.3341150095947114, -274.4676219728029309 ) ) ;
#38896 = CARTESIAN_POINT ( 'NONE',  ( -69.90918191436207962, -299.5399602978421285, -203.4232861379292672 ) ) ;
#38897 = CARTESIAN_POINT ( 'NONE',  ( 155.5427215445328386, 17.93151222991971139, 8.507834038804169552 ) ) ;
#38898 = DIRECTION ( 'NONE',  ( 0.9849620900324523864, 0.000000000000000000, -0.1727706028203384037 ) ) ;
#38899 = CARTESIAN_POINT ( 'NONE',  ( -96.36887887570836142, -295.3387268779783881, -222.8627216518738123 ) ) ;
#38900 = FACE_OUTER_BOUND ( 'NONE', #19360, .T. ) ;
#38901 = CARTESIAN_POINT ( 'NONE',  ( -109.9659129573688716, -277.9486957903625353, -278.7906956079009433 ) ) ;
#38902 = CARTESIAN_POINT ( 'NONE',  ( 26.59067294840640017, -276.1994243524819694, -228.1632461027326428 ) ) ;
#38903 = CARTESIAN_POINT ( 'NONE',  ( -0.4989284012178738514, -281.6335584687190021, -337.7216144051529341 ) ) ;
#38904 = CARTESIAN_POINT ( 'NONE',  ( 10.79103590186578288, -290.1364750279996088, -326.6535731360902446 ) ) ;
#38905 = CARTESIAN_POINT ( 'NONE',  ( -101.0387348915883479, -297.5136553189619804, -312.4732526350452986 ) ) ;
#38906 = CARTESIAN_POINT ( 'NONE',  ( -74.40074275643280544, -296.7383757356394653, -337.4625644740273742 ) ) ;
#38907 = CARTESIAN_POINT ( 'NONE',  ( 29.10296112272665425, -295.0955987878288056, -235.9353222072598726 ) ) ;
#38908 = CARTESIAN_POINT ( 'NONE',  ( 25.22910672298099044, -278.9957808248648803, -229.2198148158289541 ) ) ;
#38909 = CARTESIAN_POINT ( 'NONE',  ( 34.84613560998990067, -283.2365130819293313, -252.1371520393899175 ) ) ;
#38910 = CARTESIAN_POINT ( 'NONE',  ( -98.04308173675568128, -295.2220722057135731, -227.2721812352086772 ) ) ;
#38911 = CARTESIAN_POINT ( 'NONE',  ( -107.2009437233996891, -286.5458036563655924, -239.7967779330370774 ) ) ;
#38912 = CARTESIAN_POINT ( 'NONE',  ( 32.60441912591705460, -286.7641590877215663, -292.4791470319245832 ) ) ;
#38913 = CARTESIAN_POINT ( 'NONE',  ( 27.76947042884798122, -280.3632157620247085, -229.3486196732935127 ) ) ;
#38914 = CARTESIAN_POINT ( 'NONE',  ( -46.31138446648969165, -155.9421665903751659, -364.5751334320801789 ) ) ;
#38915 = ORIENTED_EDGE ( 'NONE', *, *, #54472, .T. ) ;
#38916 = CARTESIAN_POINT ( 'NONE',  ( 20.11773611681064011, -286.8138030240005492, -320.7496581208525299 ) ) ;
#38917 = CARTESIAN_POINT ( 'NONE',  ( -41.31983851173026778, -285.6674403338118395, -197.4359154329331716 ) ) ;
#38918 = ORIENTED_EDGE ( 'NONE', *, *, #74417, .T. ) ;
#38919 = CARTESIAN_POINT ( 'NONE',  ( -47.20294258024109979, -284.2543210959161684, -346.4153644551080902 ) ) ;
#38920 = CARTESIAN_POINT ( 'NONE',  ( 33.60808501386378566, -276.1138442194991285, -287.6827196816861374 ) ) ;
#38921 = CARTESIAN_POINT ( 'NONE',  ( -79.41330786547507614, -290.4190967844235729, -206.1768812656930834 ) ) ;
#38922 = CARTESIAN_POINT ( 'NONE',  ( 34.22650671086350371, -281.8448330589279180, -242.0856870232992151 ) ) ;
#38923 = CARTESIAN_POINT ( 'NONE',  ( 195.4197218357614361, 19.73101387165973364, -13.32484321907415747 ) ) ;
#38924 = CARTESIAN_POINT ( 'NONE',  ( -98.03675291034157624, -280.6945823384134542, -224.0924663166605910 ) ) ;
#38925 = CARTESIAN_POINT ( 'NONE',  ( 31.06029978177634732, -282.3407270155029778, -305.6727407117599569 ) ) ;
#38926 = CARTESIAN_POINT ( 'NONE',  ( -53.35057174420112602, -286.7666405000204577, -340.3538533559490702 ) ) ;
#38927 = CARTESIAN_POINT ( 'NONE',  ( 154.5379790899321222, 206.7802150222307205, -217.4094443645867614 ) ) ;
#38928 = ORIENTED_EDGE ( 'NONE', *, *, #63047, .T. ) ;
#38929 = CARTESIAN_POINT ( 'NONE',  ( 26.83531001496087143, -277.0346737873732650, -231.7726260706255630 ) ) ;
#38930 = CARTESIAN_POINT ( 'NONE',  ( -110.6672959571649102, -266.1490546199543701, -306.8034369765820202 ) ) ;
#38931 = CARTESIAN_POINT ( 'NONE',  ( 36.19165312914957155, -279.4066972170023178, -257.5278501546050052 ) ) ;
#38932 = CARTESIAN_POINT ( 'NONE',  ( -103.8078168060792308, -296.3120501644810361, -239.8066296507456912 ) ) ;
#38933 = CARTESIAN_POINT ( 'NONE',  ( 22.23499882974141073, -293.7140350553862049, -319.0659211555440606 ) ) ;
#38934 = CARTESIAN_POINT ( 'NONE',  ( -101.6167628974845485, -254.6067659492810549, -324.2419241925626920 ) ) ;
#38936 = CARTESIAN_POINT ( 'NONE',  ( -80.89588987942693166, -288.0539845580580618, -330.0021757292981874 ) ) ;
#38935 = CARTESIAN_POINT ( 'NONE',  ( 97.90671567993493341, -298.2887776826660797, -193.9822965058080513 ) ) ;
#38937 = CARTESIAN_POINT ( 'NONE',  ( -39.70502066771997107, -296.9425305464727671, -344.5713344866962871 ) ) ;
#38938 = CARTESIAN_POINT ( 'NONE',  ( 20.72002864524939980, -288.2369376787176520, -225.3047185328026103 ) ) ;
#38939 = ORIENTED_EDGE ( 'NONE', *, *, #19590, .T. ) ;
#38940 = CARTESIAN_POINT ( 'NONE',  ( 6.352435600664771975, -293.5711424186819158, -207.2450129433816812 ) ) ;
#38941 = CARTESIAN_POINT ( 'NONE',  ( -95.81896027629571222, -285.6587821465279262, -226.5615918734511069 ) ) ;
#38942 = CARTESIAN_POINT ( 'NONE',  ( -113.8715407284473997, -271.5443771474579648, -264.6355703682659168 ) ) ;
#38943 = CARTESIAN_POINT ( 'NONE',  ( -70.83657853913591396, -292.4242929471875527, -201.2072898770309450 ) ) ;
#38944 = CARTESIAN_POINT ( 'NONE',  ( -40.63606544407501531, -292.5041375600537776, -193.4800462869531543 ) ) ;
#38945 = CARTESIAN_POINT ( 'NONE',  ( -102.8444971011521716, -290.2821861333493985, -302.5850779066218479 ) ) ;
#38946 = ORIENTED_EDGE ( 'NONE', *, *, #14513, .F. ) ;
#38947 = DIRECTION ( 'NONE',  ( 0.000000000000000000, 0.000000000000000000, 1.000000000000000000 ) ) ;
#38948 = CARTESIAN_POINT ( 'NONE',  ( -15.28277488989663091, -300.1859184509785905, -194.5894067391707836 ) ) ;
#38949 = CARTESIAN_POINT ( 'NONE',  ( -99.23710006424150265, -271.9502294218637530, -225.1403997163347697 ) ) ;
#38950 = CARTESIAN_POINT ( 'NONE',  ( -8.412290636039669423, -281.7226062797830082, -337.6403697251629410 ) ) ;
#38951 = ORIENTED_EDGE ( 'NONE', *, *, #83939, .T. ) ;
#38952 = CARTESIAN_POINT ( 'NONE',  ( 10.48289776478432067, -275.9198106377223780, -330.6979981948464342 ) ) ;
#38953 = CARTESIAN_POINT ( 'NONE',  ( -57.05592824709768252, -272.1935891791212043, -199.1896894604461465 ) ) ;
#38954 = CARTESIAN_POINT ( 'NONE',  ( -96.61202424024402546, -281.0301961139024343, -225.6422002244793532 ) ) ;
#38955 = CARTESIAN_POINT ( 'NONE',  ( 16.47733404406061908, -274.4165876544465164, -321.4920972521829299 ) ) ;
#38956 = CARTESIAN_POINT ( 'NONE',  ( -93.92948339625232279, -298.4164489833885909, -223.5980776592406869 ) ) ;
#38957 = CARTESIAN_POINT ( 'NONE',  ( 52.12983541473749227, -300.2777557423787016, -197.0351508630318449 ) ) ;
#38958 = CARTESIAN_POINT ( 'NONE',  ( -111.5005418464798623, -298.3736825558245869, -252.8423676410268115 ) ) ;
#38959 = CARTESIAN_POINT ( 'NONE',  ( -38.31042497412869352, -272.0601773622864243, -195.0121406894418215 ) ) ;
#38960 = CARTESIAN_POINT ( 'NONE',  ( 33.40476224272852335, -293.9608878124998910, -251.9537626458941304 ) ) ;
#38961 = CARTESIAN_POINT ( 'NONE',  ( 9.235706666057446057, -291.2808837788294340, -213.3220331965499952 ) ) ;
#38962 = FACE_OUTER_BOUND ( 'NONE', #14336, .T. ) ;
#38963 = CARTESIAN_POINT ( 'NONE',  ( -42.79554508842491600, -277.6115874670767312, -347.1060362404298303 ) ) ;
#38964 = CARTESIAN_POINT ( 'NONE',  ( -40.52313901784983585, -298.3443636269313970, -197.3967600650562133 ) ) ;
#38965 = CARTESIAN_POINT ( 'NONE',  ( -47.20945034132956408, -281.8598615415051540, -346.2289357820915825 ) ) ;
#38966 = CARTESIAN_POINT ( 'NONE',  ( 29.28925649795061048, -296.0120784328213404, -305.1511171591659490 ) ) ;
#38967 = CARTESIAN_POINT ( 'NONE',  ( 150.8012326218627948, 131.0000000000000568, 11.50000000000000000 ) ) ;
#38968 = CARTESIAN_POINT ( 'NONE',  ( -48.36307516380174576, -282.3931924909401232, -342.6876761677719401 ) ) ;
#38969 = CARTESIAN_POINT ( 'NONE',  ( -112.4925948611060278, -282.5929181930020491, -267.1663043245724793 ) ) ;
#38970 = ADVANCED_FACE ( 'NONE', ( #55331 ), #55014, .T. ) ;
#38971 = CARTESIAN_POINT ( 'NONE',  ( -1.196520178436188742, -275.1376827105027019, -334.5194833867844295 ) ) ;
#38972 = CARTESIAN_POINT ( 'NONE',  ( 16.94890696751424741, -282.8253361369538652, -218.5421941955870011 ) ) ;
#38973 = DIRECTION ( 'NONE',  ( -0.000000000000000000, -0.000000000000000000, 1.000000000000000000 ) ) ;
#38974 = AXIS2_PLACEMENT_3D ( 'NONE', #23321, #81524, #9558 ) ;
#38975 = CARTESIAN_POINT ( 'NONE',  ( -95.40473791851191265, -271.6244640803246853, -220.9940584642222348 ) ) ;
#38976 = CARTESIAN_POINT ( 'NONE',  ( -109.5825018052297963, -280.8190351038822996, -249.5934748548683331 ) ) ;
#38977 = DIRECTION ( 'NONE',  ( -0.000000000000000000, 1.000000000000000000, -0.000000000000000000 ) ) ;
#38978 = CARTESIAN_POINT ( 'NONE',  ( -5.405234742231955103, -288.3891990309886069, -201.8820965183122382 ) ) ;
#38979 = CARTESIAN_POINT ( 'NONE',  ( -105.9330854110499445, -288.1531488174302353, -300.8227834273016015 ) ) ;
#38980 = DIRECTION ( 'NONE',  ( -1.000000000000000000, -0.000000000000000000, -0.000000000000000000 ) ) ;
#38981 = CARTESIAN_POINT ( 'NONE',  ( -73.51137206751494091, -294.3385038110995424, -334.2272697142782363 ) ) ;
#38982 = CARTESIAN_POINT ( 'NONE',  ( -42.77762028594852950, -287.2609067412499257, -344.4484903202602482 ) ) ;
#38983 = CARTESIAN_POINT ( 'NONE',  ( -96.00709874043252512, -235.9016261432062720, -336.2420922186948928 ) ) ;
#38984 = CARTESIAN_POINT ( 'NONE',  ( -109.7603545548370931, -294.8033588189083503, -250.8042810271120402 ) ) ;
#38985 = CARTESIAN_POINT ( 'NONE',  ( 38.94730303222441847, -286.0113107290040375, -268.7192447469402623 ) ) ;
#38986 = CARTESIAN_POINT ( 'NONE',  ( 5.369751610799484709, -282.2412376619672045, -210.1766324091266824 ) ) ;
#38987 = CARTESIAN_POINT ( 'NONE',  ( -35.94065552927719409, -281.2747063901879301, -346.3478152406299841 ) ) ;
#38988 = CARTESIAN_POINT ( 'NONE',  ( -5.792432161130517621, -288.6253538558429454, -336.1915341345905972 ) ) ;
#38989 = CARTESIAN_POINT ( 'NONE',  ( 15.67135945481114234, -282.2456455428496156, -219.2492358807538153 ) ) ;
#38990 = CARTESIAN_POINT ( 'NONE',  ( -5.954411318788324969, -283.4315928472718156, -336.4615079754016733 ) ) ;
#38991 = CARTESIAN_POINT ( 'NONE',  ( 37.46108697011733568, -289.6538132388272970, -279.8896436220896931 ) ) ;
#38992 = CARTESIAN_POINT ( 'NONE',  ( -14.81224999962049438, -298.4936074059563680, -193.3604978767456544 ) ) ;
#38993 = ORIENTED_EDGE ( 'NONE', *, *, #58451, .F. ) ;
#38994 = CARTESIAN_POINT ( 'NONE',  ( -36.93973224474150641, -274.0570866927869815, -193.3491151106246946 ) ) ;
#38995 = CARTESIAN_POINT ( 'NONE',  ( -36.20583416707631130, -294.0463177621254545, -195.7121984873012366 ) ) ;
#38996 = DIRECTION ( 'NONE',  ( -0.000000000000000000, 1.000000000000000000, -0.000000000000000000 ) ) ;
#38997 = CARTESIAN_POINT ( 'NONE',  ( -69.85430415644619018, -285.9805209788416391, -337.9475929042657754 ) ) ;
#38998 = CARTESIAN_POINT ( 'NONE',  ( 35.45666904871060154, -273.7919793432992606, -289.0807834443223214 ) ) ;
#38999 = CARTESIAN_POINT ( 'NONE',  ( 189.9243309297870610, 250.0000000000000568, 20.22542485937349355 ) ) ;
#39000 = CARTESIAN_POINT ( 'NONE',  ( -93.06368063729337337, -295.6687558741710973, -218.3082071701354607 ) ) ;
#39001 = CARTESIAN_POINT ( 'NONE',  ( -106.7784570364784003, -291.8229331462158598, -295.3606620649267143 ) ) ;
#39002 = CARTESIAN_POINT ( 'NONE',  ( -35.37928727901739734, -273.4259806303805931, -197.2730070036878658 ) ) ;
#39003 = CARTESIAN_POINT ( 'NONE',  ( -105.7495009215837740, -291.7072954930050059, -297.9038311947999205 ) ) ;
#39004 = CARTESIAN_POINT ( 'NONE',  ( -20.02812421946426724, -293.2212839492751755, -199.1493641275005757 ) ) ;
#39005 = CARTESIAN_POINT ( 'NONE',  ( -106.1478100833931251, -285.9508422871128914, -297.7712611095400348 ) ) ;
#39006 = CARTESIAN_POINT ( 'NONE',  ( -98.74203055571608445, -292.5869287079769947, -224.8572653843821456 ) ) ;
#39007 = CARTESIAN_POINT ( 'NONE',  ( -19.51802461569899450, -293.5917902759066465, -195.9049372163300688 ) ) ;
#39008 = CARTESIAN_POINT ( 'NONE',  ( -31.60447300687928163, -294.8111695704215549, -343.1854315091241006 ) ) ;
#39009 = CARTESIAN_POINT ( 'NONE',  ( 17.49009224085631686, -290.2692810093295179, -321.6081756120736372 ) ) ;
#39010 = CARTESIAN_POINT ( 'NONE',  ( 36.98445436032886136, -281.4663581058367754, -250.1958847455222781 ) ) ;
#39011 = CARTESIAN_POINT ( 'NONE',  ( -106.9334094854790465, -271.0810729753886221, -240.2735777226524192 ) ) ;
#39012 = CARTESIAN_POINT ( 'NONE',  ( -89.88469337680724891, -285.1683257312641331, -214.0015345207497717 ) ) ;
#39013 = CARTESIAN_POINT ( 'NONE',  ( 33.67054222880698688, -277.8304909373571832, -293.3634708625016287 ) ) ;
#39014 = CARTESIAN_POINT ( 'NONE',  ( -65.48205049319672355, -282.2233603389707355, -338.1630739897074704 ) ) ;
#39015 = CARTESIAN_POINT ( 'NONE',  ( -4.345659689830434047, -284.4868507100807733, -202.9951867596554678 ) ) ;
#39016 = CARTESIAN_POINT ( 'NONE',  ( -92.45207484672172882, -275.9696250686766348, -322.4282745601493048 ) ) ;
#39017 = DIRECTION ( 'NONE',  ( -0.000000000000000000, -0.000000000000000000, -1.000000000000000000 ) ) ;
#39018 = CARTESIAN_POINT ( 'NONE',  ( -97.58664566831039622, -283.4838571114924548, -311.7837312621551860 ) ) ;
#39019 = CARTESIAN_POINT ( 'NONE',  ( -59.20357792795423535, -280.9803744199904258, -196.9440421983110525 ) ) ;
#39020 = CARTESIAN_POINT ( 'NONE',  ( 38.06132436901835092, -286.4303283800328472, -255.9665318392303561 ) ) ;
#39021 = CARTESIAN_POINT ( 'NONE',  ( -3.858454154786618684, -296.3644074586063653, -336.3817229864486080 ) ) ;
#39022 = CARTESIAN_POINT ( 'NONE',  ( 9.007433788079975301, -276.2765173383014030, -209.8780773956021619 ) ) ;
#39023 = ADVANCED_FACE ( 'NONE', ( #4193 ), #61128, .T. ) ;
#39024 = CARTESIAN_POINT ( 'NONE',  ( 34.25432723298111171, -276.5239218767931675, -243.3924855000753382 ) ) ;
#39026 = ADVANCED_FACE ( 'NONE', ( #61958 ), #50499, .T. ) ;
#39025 = CARTESIAN_POINT ( 'NONE',  ( -56.60221595240335546, -277.1406179054495738, -340.8269144054496564 ) ) ;
#39027 = CARTESIAN_POINT ( 'NONE',  ( -55.76915472440706623, -299.8146850906341001, -197.7784781163661876 ) ) ;
#39028 = CARTESIAN_POINT ( 'NONE',  ( 35.17122925017660862, -285.3133092446726664, -251.8186930608801219 ) ) ;
#39029 = CARTESIAN_POINT ( 'NONE',  ( -113.0165467630394431, -292.0339229065062909, -279.7263851790283411 ) ) ;
#39030 = CARTESIAN_POINT ( 'NONE',  ( 23.60584574728441964, -291.9091297105313174, -229.6226505903001396 ) ) ;
#39031 = ORIENTED_EDGE ( 'NONE', *, *, #57561, .T. ) ;
#39032 = CARTESIAN_POINT ( 'NONE',  ( -55.01336574191913797, -291.4852909817102500, -199.5105730226777325 ) ) ;
#39033 = ORIENTED_EDGE ( 'NONE', *, *, #71157, .F. ) ;
#39034 = CARTESIAN_POINT ( 'NONE',  ( -100.4185050601238061, -291.0534040245203187, -313.9823191292185811 ) ) ;
#39035 = CARTESIAN_POINT ( 'NONE',  ( -108.7080772574181822, -279.4128477741582515, -254.4692374015736220 ) ) ;
#39036 = CARTESIAN_POINT ( 'NONE',  ( -51.72908787756697535, -296.7926990029499166, -194.9777508197268787 ) ) ;
#39037 = CARTESIAN_POINT ( 'NONE',  ( 7.477779198380253511, -287.2968412953714505, -207.8093246656045210 ) ) ;
#39038 = CARTESIAN_POINT ( 'NONE',  ( 0.2697523895151422435, -286.8721642800231280, -203.1811812881146295 ) ) ;
#39040 = CARTESIAN_POINT ( 'NONE',  ( -104.6186879773106995, -285.2678979832265895, -241.8428550806414137 ) ) ;
#39039 = VECTOR ( 'NONE', #24132, 1000.000000000000000 ) ;
#39041 = CARTESIAN_POINT ( 'NONE',  ( 199.5529246190115202, 289.5492434123001999, -97.49731541809454427 ) ) ;
#39042 = CARTESIAN_POINT ( 'NONE',  ( 178.2299433891311367, 253.8212103647281594, -165.6831904525195682 ) ) ;
#39043 = CARTESIAN_POINT ( 'NONE',  ( 201.5605228849236994, 292.5236489450776389, -53.99999999998448175 ) ) ;
#39044 = CARTESIAN_POINT ( 'NONE',  ( -43.23025606418143241, -276.3255762324919829, -343.2852335824551346 ) ) ;
#39045 = CARTESIAN_POINT ( 'NONE',  ( -105.5604524385525878, -277.1150520375541646, -297.2019060886451030 ) ) ;
#39046 = CARTESIAN_POINT ( 'NONE',  ( -88.01925875771564733, -273.0328617545135330, -212.3460600736322874 ) ) ;
#39047 = CARTESIAN_POINT ( 'NONE',  ( -106.8307097481477967, -265.7384667639375380, -305.7804014683771925 ) ) ;
#39048 = CARTESIAN_POINT ( 'NONE',  ( -103.1899387383158029, -276.7251046416644726, -309.4176808801952347 ) ) ;
#39049 = CARTESIAN_POINT ( 'NONE',  ( -108.4888339475103862, -291.2642207992174122, -253.6910708394728999 ) ) ;
#39050 = CARTESIAN_POINT ( 'NONE',  ( -82.88311288681744315, -298.2500014121351342, -208.4068894757872670 ) ) ;
#39051 = CARTESIAN_POINT ( 'NONE',  ( -112.5436807083961099, -296.8410566850397458, -286.6150104496201152 ) ) ;
#39052 = CARTESIAN_POINT ( 'NONE',  ( -41.03709630743936287, -295.2665969390627083, -343.2800913917124603 ) ) ;
#39053 = ORIENTED_EDGE ( 'NONE', *, *, #27120, .F. ) ;
#39054 = CARTESIAN_POINT ( 'NONE',  ( -8.412901268750733408, -278.5965707293539708, -340.1779943506299446 ) ) ;
#39055 = CARTESIAN_POINT ( 'NONE',  ( 38.80946278849148712, -281.1972177424339634, -281.3396101231168700 ) ) ;
#39056 = CARTESIAN_POINT ( 'NONE',  ( -83.64357314639039487, -280.4794828301169787, -213.4591250477863582 ) ) ;
#39057 = CARTESIAN_POINT ( 'NONE',  ( -39.90600557863260889, -278.8440571491466358, -346.3174016105907072 ) ) ;
#39058 = CARTESIAN_POINT ( 'NONE',  ( -67.04062821060830402, -296.2297936189843313, -203.0171833125274645 ) ) ;
#39059 = DIRECTION ( 'NONE',  ( -0.3428573139466628561, 0.000000000000000000, 0.9393874931428880526 ) ) ;
#39060 = CARTESIAN_POINT ( 'NONE',  ( -101.8559310399065794, -278.2535160764398370, -304.5212411430550787 ) ) ;
#39061 = CARTESIAN_POINT ( 'NONE',  ( -66.17613040871646035, -274.4870492672792466, -199.1238451561870590 ) ) ;
#39062 = CARTESIAN_POINT ( 'NONE',  ( 37.02110170347383189, -286.4640280874083373, -288.4017372538645532 ) ) ;
#39063 = CARTESIAN_POINT ( 'NONE',  ( -92.68705999424723530, -275.2592177793211476, -219.7270143720013778 ) ) ;
#39064 = CARTESIAN_POINT ( 'NONE',  ( 0.7375189523886449550, -275.1298386140090884, -336.6674802013300791 ) ) ;
#39065 = PLANE ( 'NONE',  #47484 ) ;
#39066 = CARTESIAN_POINT ( 'NONE',  ( -105.2667651259092736, -289.3847149114924946, -297.6777755072259879 ) ) ;
#39067 = CARTESIAN_POINT ( 'NONE',  ( -107.8293684223767315, -284.2946244181899829, -239.4903874724545005 ) ) ;
#39068 = CARTESIAN_POINT ( 'NONE',  ( -8.114428241124437946, -280.9038493841821378, -338.3592105526763021 ) ) ;
#39070 = CARTESIAN_POINT ( 'NONE',  ( -107.8893236561030733, -282.9433505169986915, -246.4438844820208203 ) ) ;
#39069 = CARTESIAN_POINT ( 'NONE',  ( 34.03148051693681708, -279.8916278831450200, -252.3865886998769668 ) ) ;
#39071 = CARTESIAN_POINT ( 'NONE',  ( -110.3029948668050508, -292.3286092238428182, -287.7833098781530907 ) ) ;
#39072 = CARTESIAN_POINT ( 'NONE',  ( -43.80124609601869423, -281.1739228157629782, -197.1983356964263407 ) ) ;
#39073 = CARTESIAN_POINT ( 'NONE',  ( 121.2562178857222364, 149.7689829628632197, -263.4557525892608965 ) ) ;
#39074 = CARTESIAN_POINT ( 'NONE',  ( -83.41586613599116617, -282.0713700429554365, -331.1201782945501577 ) ) ;
#39075 = CARTESIAN_POINT ( 'NONE',  ( 35.14292206396039830, -295.3041644955467291, -251.0507882953545504 ) ) ;
#39076 = CARTESIAN_POINT ( 'NONE',  ( -105.2596579256097584, -277.2375362024735068, -236.1687128667616662 ) ) ;
#39077 = CARTESIAN_POINT ( 'NONE',  ( -31.74671705337128103, -284.9818726723361806, -345.3322223354393827 ) ) ;
#39078 = FACE_OUTER_BOUND ( 'NONE', #23820, .T. ) ;
#39079 = CARTESIAN_POINT ( 'NONE',  ( -61.25644552779765206, -293.6643020961961383, -198.6303524078388705 ) ) ;
#39080 = CARTESIAN_POINT ( 'NONE',  ( -15.83096643689033911, -274.7738702360429670, -342.2646442902983495 ) ) ;
#39081 = CARTESIAN_POINT ( 'NONE',  ( 23.73930902040109814, -286.1262571540097497, -223.7212068313149871 ) ) ;
#39082 = CARTESIAN_POINT ( 'NONE',  ( -60.49078163218569415, -290.1468668022767474, -200.2321114891611842 ) ) ;
#39083 = CARTESIAN_POINT ( 'NONE',  ( -48.18343439339133027, -281.1257490775032579, -435.6442049083771053 ) ) ;
#39084 = CARTESIAN_POINT ( 'NONE',  ( 12.06694098884280564, -275.0329944022522568, -324.8363142391011138 ) ) ;
#39085 = CARTESIAN_POINT ( 'NONE',  ( 6.778348401442580773, -292.5847899992535304, -330.1268138434207913 ) ) ;
#39086 = DIRECTION ( 'NONE',  ( 1.000000000000000000, 0.000000000000000000, 0.000000000000000000 ) ) ;
#39087 = CARTESIAN_POINT ( 'NONE',  ( 197.0471578326374527, 42.02301189210707122, 12.21301650322624432 ) ) ;
#39088 = CARTESIAN_POINT ( 'NONE',  ( 37.38763089432415399, -292.2268243310051048, -285.7959759287206793 ) ) ;
#39089 = CARTESIAN_POINT ( 'NONE',  ( -90.25045991324962813, -286.8888408193017767, -218.8377516844456636 ) ) ;
#39090 = CARTESIAN_POINT ( 'NONE',  ( -43.12778944242869272, -287.3641256548171441, -346.1271736032116451 ) ) ;
#39091 = CARTESIAN_POINT ( 'NONE',  ( 33.95495618862442910, -288.7381880323155769, -252.0850026225271563 ) ) ;
#39092 = CARTESIAN_POINT ( 'NONE',  ( 151.6916247871641303, 20.99999999999999645, -4.896253172919318608 ) ) ;
#39093 = CARTESIAN_POINT ( 'NONE',  ( 32.47077699069772194, -288.6463593815438458, -292.4117572671948437 ) ) ;
#39094 = CARTESIAN_POINT ( 'NONE',  ( 37.19344518559813650, -295.6737268671845413, -281.4479983466865178 ) ) ;
#39095 = CARTESIAN_POINT ( 'NONE',  ( 175.2296996224750103, 20.99999999999998934, 0.000000000000000000 ) ) ;
#39096 = VECTOR ( 'NONE', #63622, 1000.000000000000000 ) ;
#39097 = CARTESIAN_POINT ( 'NONE',  ( 26.02025418839926729, -288.1864000262094123, -227.2880529151445046 ) ) ;
#39098 = CARTESIAN_POINT ( 'NONE',  ( -23.23223106991694209, -274.9530651570714213, -344.6452581387861756 ) ) ;
#39099 = CARTESIAN_POINT ( 'NONE',  ( -114.0232400600147287, -278.9772664380271863, -263.0201646655798413 ) ) ;
#39100 = CARTESIAN_POINT ( 'NONE',  ( -28.22329423508226043, -279.8314409507368055, -193.8706122946222195 ) ) ;
#39101 = CARTESIAN_POINT ( 'NONE',  ( 10.21538519671316436, -300.6301984948891004, -195.7001660573785387 ) ) ;
#39102 = CARTESIAN_POINT ( 'NONE',  ( -43.18343439339132317, -283.1093320178188151, -507.6442049081570076 ) ) ;
#39103 = CARTESIAN_POINT ( 'NONE',  ( -84.89686901255474538, -283.3965685805841304, -212.2979121390890498 ) ) ;
#39104 = DIRECTION ( 'NONE',  ( 1.000000000000000000, 0.000000000000000000, 0.000000000000000000 ) ) ;
#39105 = CARTESIAN_POINT ( 'NONE',  ( -109.9782047793844129, -276.4929592356365333, -285.6844229600759490 ) ) ;
#39106 = CARTESIAN_POINT ( 'NONE',  ( 26.58656734916524300, -280.0792582632824974, -309.6790888600927474 ) ) ;
#39107 = CARTESIAN_POINT ( 'NONE',  ( 113.5000000000000568, -211.8141737103562434, -518.0411269958476623 ) ) ;
#39108 = CARTESIAN_POINT ( 'NONE',  ( -51.20581444962512307, -275.7061765038387762, -345.3977362771613571 ) ) ;
#39109 =( BOUNDED_SURFACE ( )  B_SPLINE_SURFACE ( 3, 2, ( 
 ( #33768, #62680, #19556 ),
 ( #48422, #32374, #11040 ),
 ( #61274, #25261, #83007 ),
 ( #39910, #68830, #86743 ),
 ( #42724, #12954, #21905 ),
 ( #27608, #21426, #49381 ),
 ( #29001, #72110, #7226 ),
 ( #79664, #20965, #77804 ) ),
 .UNSPECIFIED., .F., .F., .F. ) 
 B_SPLINE_SURFACE_WITH_KNOTS ( ( 4, 2, 2, 4 ),
 ( 3, 3 ),
 ( 0.005169333131380775964, 0.006119585499875557916, 0.006594711684122948891, 0.007069837868370339000 ),
 ( 0.1676400288617256873, 1.000000000000000000 ),
 .UNSPECIFIED. ) 
 GEOMETRIC_REPRESENTATION_ITEM ( )  RATIONAL_B_SPLINE_SURFACE ( (
 ( 0.9182612059639421176, 0.7562074088418391238, 1.000000000000000000),
 ( 0.9234184755582998116, 0.7715893842249726964, 1.000000000000000000),
 ( 0.9290856680301433634, 0.7884922460006588141, 1.000000000000000000),
 ( 0.9358458655730186315, 0.8086550841628119546, 1.000000000000000000),
 ( 0.9377882735816500670, 0.8144484737900394844, 1.000000000000000000),
 ( 0.9404881272938196979, 0.8225010067396629765, 1.000000000000000000),
 ( 0.9412390135326376139, 0.8247405859258407634, 1.000000000000000000),
 ( 0.9412312448011985744, 0.8247174150534309911, 1.000000000000000000) ) ) 
 REPRESENTATION_ITEM ( '' )  SURFACE ( )  );
#39110 = CARTESIAN_POINT ( 'NONE',  ( -102.0671319982980805, -297.5958823943206539, -305.5935777317882298 ) ) ;
#39111 = CARTESIAN_POINT ( 'NONE',  ( -31.67291075209326223, -281.9025378275022149, -346.8554240143182028 ) ) ;
#39112 = CARTESIAN_POINT ( 'NONE',  ( -79.87440459920578917, -298.4020738051065678, -210.7425177149031867 ) ) ;
#39113 = CARTESIAN_POINT ( 'NONE',  ( -99.53052609969535069, -298.4616263663543236, -225.7982612776796429 ) ) ;
#39114 = CARTESIAN_POINT ( 'NONE',  ( -51.56142321081932778, -273.5320927703592702, -198.6860848071059138 ) ) ;
#39115 = CARTESIAN_POINT ( 'NONE',  ( 23.41019998294785864, -294.9531667766371470, -226.3596651026312827 ) ) ;
#39116 = CARTESIAN_POINT ( 'NONE',  ( 36.78498938113761341, -287.9805158355109143, -291.2477568069825224 ) ) ;
#39117 =( BOUNDED_SURFACE ( )  B_SPLINE_SURFACE ( 3, 2, ( 
 ( #76987, #41443, #41916 ),
 ( #12116, #85007, #20161 ),
 ( #40961, #36691, #43336 ),
 ( #87334, #78854, #35302 ),
 ( #93058, #14004, #79343 ),
 ( #85942, #73619, #72685 ) ),
 .UNSPECIFIED., .F., .F., .F. ) 
 B_SPLINE_SURFACE_WITH_KNOTS ( ( 4, 2, 4 ),
 ( 3, 3 ),
 ( 0.005169333131380775964, 0.006119585499875832002, 0.007069837868370888040 ),
 ( 0.4216207772072607107, 1.000000000000000000 ),
 .UNSPECIFIED. ) 
 GEOMETRIC_REPRESENTATION_ITEM ( )  RATIONAL_B_SPLINE_SURFACE ( (
 ( 0.8571520539184378507, 0.8305966477414123972, 1.000000000000000000),
 ( 0.8661649758441183344, 0.8412850701495542260, 1.000000000000000000),
 ( 0.8760690466613034744, 0.8530303058596961918, 1.000000000000000000),
 ( 0.8918213438905483459, 0.8717109521665329375, 1.000000000000000000),
 ( 0.8974258578414069376, 0.8783573442015528698, 1.000000000000000000),
 ( 0.8972948393364401642, 0.8782019693812764816, 1.000000000000000000) ) ) 
 REPRESENTATION_ITEM ( '' )  SURFACE ( )  );
#39118 = CARTESIAN_POINT ( 'NONE',  ( -68.06420618579394954, -277.7317965669738555, -201.3148241212551284 ) ) ;
#39119 = CARTESIAN_POINT ( 'NONE',  ( -78.13820641377049014, -289.4175317387495738, -335.7275662592843446 ) ) ;
#39120 = CARTESIAN_POINT ( 'NONE',  ( 22.14584001274747038, -287.2061345901546474, -313.0769349186299451 ) ) ;
#39121 = CARTESIAN_POINT ( 'NONE',  ( 11.98281780226643534, -290.7376934790190148, -213.8625111247438895 ) ) ;
#39122 = ORIENTED_EDGE ( 'NONE', *, *, #81466, .T. ) ;
#39123 = CARTESIAN_POINT ( 'NONE',  ( -49.37856652629597676, -155.6656457446864010, -366.7448178265262868 ) ) ;
#39124 = CARTESIAN_POINT ( 'NONE',  ( -0.9662438810527488320, -288.0632857770915507, -333.7819143788195220 ) ) ;
#39125 = FACE_OUTER_BOUND ( 'NONE', #36184, .T. ) ;
#39126 = CARTESIAN_POINT ( 'NONE',  ( -83.73144776340052431, -284.6123414491839299, -331.5900576903684396 ) ) ;
#39127 = CARTESIAN_POINT ( 'NONE',  ( 4.024866690522677537, -291.6532025264916115, -205.6326011215083156 ) ) ;
#39128 = CARTESIAN_POINT ( 'NONE',  ( 38.90978637575963717, -283.1466346999904999, -269.9144059094882664 ) ) ;
#39129 = ADVANCED_FACE ( 'NONE', ( #34014 ), #91752, .T. ) ;
#39130 = CARTESIAN_POINT ( 'NONE',  ( -25.48861644633841195, -281.5153657426774316, -194.7780333742352923 ) ) ;
#39131 = CARTESIAN_POINT ( 'NONE',  ( 11.91512519495077704, -282.1777297027140889, -324.2384338361215441 ) ) ;
#39132 = CARTESIAN_POINT ( 'NONE',  ( -114.3662121264988514, -296.5257802791869040, -272.4697928229329023 ) ) ;
#39133 = CARTESIAN_POINT ( 'NONE',  ( -57.00959231293859375, -275.1084223918394400, -199.4954901923533725 ) ) ;
#39134 = CARTESIAN_POINT ( 'NONE',  ( 7.688098436528640889, -290.6904391448102842, -210.8282359685273946 ) ) ;
#39135 = CARTESIAN_POINT ( 'NONE',  ( -1.515474592538123444, -273.3332820062719293, -206.2872836043779330 ) ) ;
#39136 = EDGE_LOOP ( 'NONE', ( #61477, #74306, #29666, #91451 ) ) ;
#39137 = DIRECTION ( 'NONE',  ( -0.000000000000000000, -0.000000000000000000, -1.000000000000000000 ) ) ;
#39138 = CARTESIAN_POINT ( 'NONE',  ( -110.0770768630098360, -286.6779795003275808, -254.4623533305098135 ) ) ;
#39139 = CARTESIAN_POINT ( 'NONE',  ( 15.27663094474967664, -295.4091959345665259, -326.1536241480708895 ) ) ;
#39140 = CARTESIAN_POINT ( 'NONE',  ( -104.6946986636557710, -285.5859788167392139, -241.8150223254299647 ) ) ;
#39141 = CARTESIAN_POINT ( 'NONE',  ( -38.55330232588386252, -276.1257497584532530, -347.1162626573317311 ) ) ;
#39142 = CARTESIAN_POINT ( 'NONE',  ( 23.02288617697955431, -293.5653158833952716, -222.7015498795072972 ) ) ;
#39143 = CARTESIAN_POINT ( 'NONE',  ( 15.45568152725684463, -284.9286340258303767, -216.0219795157446185 ) ) ;
#39144 = B_SPLINE_CURVE_WITH_KNOTS ( 'NONE', 3,
 ( #90645, #10667, #25807, #54687, #83561, #84042, #40456, #10196 ),
 .UNSPECIFIED., .F., .F.,
 ( 4, 2, 2, 4 ),
 ( 5.346692419836454808E-16, 0.001939204242612728663, 0.002908806363918823353, 0.003878408485224918260 ),
 .UNSPECIFIED. ) ;
#39145 = CARTESIAN_POINT ( 'NONE',  ( 22.19020729555418470, -293.2298965614671715, -221.5584921295464653 ) ) ;
#39146 = CARTESIAN_POINT ( 'NONE',  ( -109.6432861772453862, -290.7493954880410456, -280.6766433401361382 ) ) ;
#39147 = CARTESIAN_POINT ( 'NONE',  ( 183.0442525570908288, 264.6571197653884155, -7.500000000000000000 ) ) ;
#39148 = CARTESIAN_POINT ( 'NONE',  ( 154.1270911980395226, 19.37729811922127610, -12.09914501918770924 ) ) ;
#39149 = CARTESIAN_POINT ( 'NONE',  ( 202.6186562182569730, 291.9839156117442940, -53.99999999998471623 ) ) ;
#39150 = CARTESIAN_POINT ( 'NONE',  ( -107.5812874519488958, -285.6877340002882306, -300.3141271305244118 ) ) ;
#39151 = CARTESIAN_POINT ( 'NONE',  ( 25.18497378105905682, -273.6952119285918457, -320.2651865833026363 ) ) ;
#39152 = ORIENTED_EDGE ( 'NONE', *, *, #65408, .T. ) ;
#39153 = CARTESIAN_POINT ( 'NONE',  ( -45.68825912565812786, -282.0806108211816650, -343.2447461898660208 ) ) ;
#39154 = CARTESIAN_POINT ( 'NONE',  ( -114.2111188623227065, -278.1675406940815378, -274.4643794785486079 ) ) ;
#39155 = CARTESIAN_POINT ( 'NONE',  ( -52.21607459267105611, -281.8615825287808434, -196.9679092636669395 ) ) ;
#39156 = CARTESIAN_POINT ( 'NONE',  ( -101.4906385538783979, -256.4535248988104286, -325.6885106913075560 ) ) ;
#39157 = CARTESIAN_POINT ( 'NONE',  ( -5.716086811928156486, -281.2190912455022271, -339.9199195617673013 ) ) ;
#39158 = CARTESIAN_POINT ( 'NONE',  ( -19.39655578048297002, -284.3042442637076874, -197.9054860830946723 ) ) ;
#39159 = CARTESIAN_POINT ( 'NONE',  ( -77.68371183542342351, -299.2785238985585465, -205.9678255979188464 ) ) ;
#39160 = CARTESIAN_POINT ( 'NONE',  ( -47.79564887872264478, -295.6808908574199108, -342.7222144880499286 ) ) ;
#39161 = ORIENTED_EDGE ( 'NONE', *, *, #26867, .F. ) ;
#39162 = CARTESIAN_POINT ( 'NONE',  ( 33.10658487813985573, -291.9596945361947178, -249.2504135550059914 ) ) ;
#39163 = CARTESIAN_POINT ( 'NONE',  ( -68.96586422155552043, -278.1085800970627133, -340.4699035502929405 ) ) ;
#39164 = CARTESIAN_POINT ( 'NONE',  ( 0.6124664196134874672, -274.5735718893940316, -208.0034300710455568 ) ) ;
#39165 = CARTESIAN_POINT ( 'NONE',  ( 39.07133972923853804, -274.5543815347095915, -276.8833759425634753 ) ) ;
#39166 = CARTESIAN_POINT ( 'NONE',  ( 140.6539576904058606, 250.5000000000000568, -10.49999999999999822 ) ) ;
#39167 = CARTESIAN_POINT ( 'NONE',  ( 21.38441682075998784, -272.9106887342970253, -223.6906697486223834 ) ) ;
#39168 = CARTESIAN_POINT ( 'NONE',  ( 1.485778912310653288, -295.9691076023856340, -336.1717034843913439 ) ) ;
#39169 = CARTESIAN_POINT ( 'NONE',  ( 153.9755810662746569, 128.3195885613610869, 13.16651113973756715 ) ) ;
#39170 = AXIS2_PLACEMENT_3D ( 'NONE', #17235, #44701, #80690 ) ;
#39171 = DIRECTION ( 'NONE',  ( -0.000000000000000000, 1.000000000000000000, -0.000000000000000000 ) ) ;
#39172 = CARTESIAN_POINT ( 'NONE',  ( -65.42143309300976739, -284.5077384583489675, -338.0929732961477612 ) ) ;
#39173 = CARTESIAN_POINT ( 'NONE',  ( -16.39931441994946582, -284.5453960787947381, -343.4594389166588826 ) ) ;
#39174 = CARTESIAN_POINT ( 'NONE',  ( -110.4924841550375305, -283.8936123408574304, -270.9017860693681996 ) ) ;
#39175 = CARTESIAN_POINT ( 'NONE',  ( -13.54652497288685176, -275.1380186982442524, -340.2734753092330493 ) ) ;
#39176 = CARTESIAN_POINT ( 'NONE',  ( -4.255718922491010581, -284.4716355098751137, -336.8154882768932907 ) ) ;
#39177 = CARTESIAN_POINT ( 'NONE',  ( -39.19441413202154223, -275.5556986400789015, -344.0311607746497771 ) ) ;
#39178 = CARTESIAN_POINT ( 'NONE',  ( 34.47012510449684441, -276.8254605182967225, -285.1018042379710096 ) ) ;
#39179 = DIRECTION ( 'NONE',  ( 1.000000000000000000, 0.000000000000000000, -0.000000000000000000 ) ) ;
#39180 = CARTESIAN_POINT ( 'NONE',  ( -114.2164696528975583, -279.3752018324797177, -268.7478607598796998 ) ) ;
#39181 = CARTESIAN_POINT ( 'NONE',  ( -45.27326818481799364, -280.4467181314177537, -193.7796318452997468 ) ) ;
#39182 = VERTEX_POINT ( 'NONE', #86981 ) ;
#39183 = DIRECTION ( 'NONE',  ( 2.220446049250312686E-15, 0.000000000000000000, 1.000000000000000000 ) ) ;
#39184 = CARTESIAN_POINT ( 'NONE',  ( 32.70820596841620898, -289.0381642780544098, -241.3569490274842337 ) ) ;
#39185 = CARTESIAN_POINT ( 'NONE',  ( -75.75151563270300414, -294.7759445622058365, -332.6880569481569410 ) ) ;
#39186 = CARTESIAN_POINT ( 'NONE',  ( -62.73782756125602589, -288.7226680088817830, -343.0008268572557313 ) ) ;
#39187 = CARTESIAN_POINT ( 'NONE',  ( -1.678702082059443157, -284.7710603968801024, -205.4489646690272764 ) ) ;
#39189 = CARTESIAN_POINT ( 'NONE',  ( -95.06734814741933803, -289.4379520340669956, -224.0190299883646219 ) ) ;
#39188 = CARTESIAN_POINT ( 'NONE',  ( -14.36493683927242060, -284.9305665826997256, -200.3974148420774668 ) ) ;
#39190 = CARTESIAN_POINT ( 'NONE',  ( 4.941657197055613793, -287.8425488357234485, -210.3051975103153097 ) ) ;
#39191 = CARTESIAN_POINT ( 'NONE',  ( -41.30491071720452823, -275.1018660214030547, -345.2692011847943832 ) ) ;
#39192 = CARTESIAN_POINT ( 'NONE',  ( 35.18005549901627660, -286.2492492666621047, -293.7499053798907767 ) ) ;
#39193 = CARTESIAN_POINT ( 'NONE',  ( -33.84668973151497795, -288.0962950621700429, -195.4425918820251411 ) ) ;
#39194 = CARTESIAN_POINT ( 'NONE',  ( 31.18285516593091700, -285.9562495464727476, -301.2547054288272648 ) ) ;
#39195 = CARTESIAN_POINT ( 'NONE',  ( -3.502037048887692627, -283.5352508045358491, -335.3234998129452720 ) ) ;
#39196 = CARTESIAN_POINT ( 'NONE',  ( -95.84667634917079226, -291.9039756218037382, -317.5745879250472399 ) ) ;
#39197 = CARTESIAN_POINT ( 'NONE',  ( 156.4851178187871312, 69.18068689461284748, -7.000000000000000888 ) ) ;
#39198 = CARTESIAN_POINT ( 'NONE',  ( 154.5739546116916472, 19.95362051968762529, -14.09237539257703276 ) ) ;
#39199 = CARTESIAN_POINT ( 'NONE',  ( -111.7259169901823697, -298.6415263055387186, -257.0832235117029541 ) ) ;
#39200 = CARTESIAN_POINT ( 'NONE',  ( 28.60176447538386668, -280.0264956302277710, -306.0887000737391759 ) ) ;
#39201 = CARTESIAN_POINT ( 'NONE',  ( 15.33492168232747588, -291.9706378633057966, -214.3476170998381463 ) ) ;
#39202 = CARTESIAN_POINT ( 'NONE',  ( -110.1555178763190810, -294.7951160924662304, -282.3856080295178685 ) ) ;
#39203 = CARTESIAN_POINT ( 'NONE',  ( 25.56702707961839494, -279.7163180401468594, -232.2659407596154324 ) ) ;
#39204 = CARTESIAN_POINT ( 'NONE',  ( -63.79605198023946855, -271.7844004016682220, -200.7666052905431684 ) ) ;
#39205 = CARTESIAN_POINT ( 'NONE',  ( -47.84708356565414533, -296.5035851753454494, -343.1511811434824040 ) ) ;
#39206 = CARTESIAN_POINT ( 'NONE',  ( -34.06437162994986778, -296.5723644529182934, -194.0552759049878944 ) ) ;
#39207 = CARTESIAN_POINT ( 'NONE',  ( 14.76727711359516704, -292.5698407363801152, -325.6659866909026277 ) ) ;
#39208 = CARTESIAN_POINT ( 'NONE',  ( -36.21517100176666304, -293.4917875990831249, -196.7679327184013687 ) ) ;
#39209 = FACE_OUTER_BOUND ( 'NONE', #15781, .T. ) ;
#39210 = CARTESIAN_POINT ( 'NONE',  ( 32.50399829062326518, -294.6429087089654786, -292.1367956863843460 ) ) ;
#39211 = CARTESIAN_POINT ( 'NONE',  ( 195.2403266774578583, 20.74618149458048677, 13.25394924001932395 ) ) ;
#39213 = CARTESIAN_POINT ( 'NONE',  ( -4.336659316753177507, -294.6045509917273648, -335.4878436705264448 ) ) ;
#39212 = CARTESIAN_POINT ( 'NONE',  ( -24.83200130879724199, -280.9135769167810395, -344.7236589037539716 ) ) ;
#39214 = CARTESIAN_POINT ( 'NONE',  ( -69.18645551823109940, -283.4595737223696688, -340.4819622638265741 ) ) ;
#39215 = CARTESIAN_POINT ( 'NONE',  ( -20.10885610051680672, -282.1919246494306890, -196.7387464819910292 ) ) ;
#39216 = CARTESIAN_POINT ( 'NONE',  ( -91.88501575833059576, -284.9662400875823778, -216.0401182537028433 ) ) ;
#39217 = CARTESIAN_POINT ( 'NONE',  ( -55.43148450691934670, -289.8186799472982216, -197.7471515260073431 ) ) ;
#39218 = CARTESIAN_POINT ( 'NONE',  ( 29.14817507504886507, -280.5234630654710486, -307.9094349044098635 ) ) ;
#39219 = CARTESIAN_POINT ( 'NONE',  ( 37.72379479509600486, -286.2744757424396198, -254.5919392249556665 ) ) ;
#39220 = DIRECTION ( 'NONE',  ( -0.2156506209390900430, 0.000000000000000000, -0.9764705882352960886 ) ) ;
#39221 = CARTESIAN_POINT ( 'NONE',  ( -92.77829237184437261, -297.4643602268567406, -319.0768716641624678 ) ) ;
#39222 = CARTESIAN_POINT ( 'NONE',  ( 0.7690221592165564779, -277.9799232077851343, -336.6493755738805476 ) ) ;
#39224 = CARTESIAN_POINT ( 'NONE',  ( -66.07411270941601344, -279.3322056802392126, -203.2167376533870708 ) ) ;
#39223 = CARTESIAN_POINT ( 'NONE',  ( 36.71359360977782416, -291.3941658529361689, -256.4248245494214871 ) ) ;
#39225 = CARTESIAN_POINT ( 'NONE',  ( -19.38883471001782155, -292.4434811104758865, -195.4284313988002566 ) ) ;
#39226 = CARTESIAN_POINT ( 'NONE',  ( -66.60830445785840936, -283.7516311058159886, -200.6992197125136386 ) ) ;
#39227 = CARTESIAN_POINT ( 'NONE',  ( -8.626191620539108484, -278.6765642235279188, -339.6600988359395501 ) ) ;
#39228 = EDGE_CURVE ( 'NONE', #6380, #57488, #57658, .T. ) ;
#39230 = CARTESIAN_POINT ( 'NONE',  ( 19.87008729753278757, -293.2548619872140421, -316.1000268374112352 ) ) ;
#39229 = AXIS2_PLACEMENT_3D ( 'NONE', #22368, #88144, #51698 ) ;
#39231 = CARTESIAN_POINT ( 'NONE',  ( -88.88668731264839096, -271.3304146053313275, -215.5804413312784789 ) ) ;
#39232 = VERTEX_POINT ( 'NONE', #85591 ) ;
#39233 = CARTESIAN_POINT ( 'NONE',  ( 197.7335303680046650, 24.96166607582781083, 12.00000000000000000 ) ) ;
#39234 = CARTESIAN_POINT ( 'NONE',  ( -38.34942626026715828, -294.5727733374662307, -343.4157066810456627 ) ) ;
#39235 = CARTESIAN_POINT ( 'NONE',  ( 175.2296996224750103, 149.6461846693799487, -24.00000000000001066 ) ) ;
#39236 = CIRCLE ( 'NONE', #63501, 6.654241149514406040 ) ;
#39237 = CARTESIAN_POINT ( 'NONE',  ( -102.0455923789670294, -287.6237833571632905, -301.4846348637937581 ) ) ;
#39238 = CARTESIAN_POINT ( 'NONE',  ( -23.40085525011318879, -297.2814403089774942, -193.5985747488931565 ) ) ;
#39239 = CARTESIAN_POINT ( 'NONE',  ( 13.90405535230756229, -288.0681059394203771, -213.4818634071896497 ) ) ;
#39240 = CARTESIAN_POINT ( 'NONE',  ( 21.96045292213683098, -287.9805814045535612, -312.9317022882359538 ) ) ;
#39241 = CARTESIAN_POINT ( 'NONE',  ( -109.8174618690418072, -280.2466066697485871, -257.0205140322607917 ) ) ;
#39242 = CARTESIAN_POINT ( 'NONE',  ( -96.92929746259173385, -298.9193605371821718, -226.4387761807520008 ) ) ;
#39243 = CARTESIAN_POINT ( 'NONE',  ( -27.48996652852445877, -278.9748759069121320, -197.5767535893036495 ) ) ;
#39244 = ORIENTED_EDGE ( 'NONE', *, *, #38852, .F. ) ;
#39245 = CARTESIAN_POINT ( 'NONE',  ( -43.28388814980958443, -297.6459089744346329, -193.5587550616638168 ) ) ;
#39246 = CARTESIAN_POINT ( 'NONE',  ( -14.42588679147071851, -294.2717350668584686, -199.5361245461241424 ) ) ;
#39247 = CARTESIAN_POINT ( 'NONE',  ( 38.64179651915917191, -295.0797377589528310, -264.6210264208356762 ) ) ;
#39248 = CARTESIAN_POINT ( 'NONE',  ( 85.55100297371609486, -296.0521521680024080, -525.1711561948568487 ) ) ;
#39249 = ADVANCED_FACE ( 'NONE', ( #22134 ), #35416, .F. ) ;
#39250 = CARTESIAN_POINT ( 'NONE',  ( -110.3479786306968577, -291.2644785409744372, -265.7374262183761857 ) ) ;
#39251 = CARTESIAN_POINT ( 'NONE',  ( 156.9186793294233837, 275.7877658745666167, 16.89624193776998595 ) ) ;
#39252 = CARTESIAN_POINT ( 'NONE',  ( -2.600766629777929051, -290.6461393623806657, -203.0162477819706908 ) ) ;
#39253 = CARTESIAN_POINT ( 'NONE',  ( -68.05254770667625053, -297.3042076727552399, -204.0984398096427128 ) ) ;
#39254 = FACE_OUTER_BOUND ( 'NONE', #52663, .T. ) ;
#39255 = CARTESIAN_POINT ( 'NONE',  ( 195.6468468325649326, 26.28259184625311207, 14.75238424381223723 ) ) ;
#39256 = CARTESIAN_POINT ( 'NONE',  ( -113.6757650018220289, -292.0971223824941490, -268.3920952787018450 ) ) ;
#39257 = CARTESIAN_POINT ( 'NONE',  ( 25.22466315766300227, -290.6948066931273047, -320.2154176792147382 ) ) ;
#39258 = CARTESIAN_POINT ( 'NONE',  ( -19.40037603436253733, -288.2836563974520914, -197.7103278067051804 ) ) ;
#39259 = CARTESIAN_POINT ( 'NONE',  ( -5.731981148427274242, -272.4686196271861718, -202.5315219597227951 ) ) ;
#39260 = CARTESIAN_POINT ( 'NONE',  ( 14.48196961711430575, -276.7083022451811303, -216.9231029507884330 ) ) ;
#39261 = CARTESIAN_POINT ( 'NONE',  ( -80.34299539760660025, -289.5448267694019933, -209.5344511864218759 ) ) ;
#39262 = CARTESIAN_POINT ( 'NONE',  ( -99.43932283705458985, -279.8293676274468567, -313.7683839085281647 ) ) ;
#39263 = ORIENTED_EDGE ( 'NONE', *, *, #75203, .F. ) ;
#39264 = CARTESIAN_POINT ( 'NONE',  ( -10.94669580006989484, -282.0474463661087725, -338.5851188835326866 ) ) ;
#39265 = CARTESIAN_POINT ( 'NONE',  ( -108.3649693109729952, -279.2628577419237672, -299.2953147673320586 ) ) ;
#39266 = CARTESIAN_POINT ( 'NONE',  ( 39.31318636514456699, -280.3418819737761396, -269.9478070697722387 ) ) ;
#39267 = CARTESIAN_POINT ( 'NONE',  ( 197.4647849659431813, 287.3553758152445994, -96.51471344131978469 ) ) ;
#39268 = CARTESIAN_POINT ( 'NONE',  ( 37.95392641538847300, -276.6808955572237778, -285.3073160645459438 ) ) ;
#39269 = SHAPE_DEFINITION_REPRESENTATION ( #59426, #80896 ) ;
#39270 = CARTESIAN_POINT ( 'NONE',  ( -69.85410986235015685, -275.1519190444135461, -201.3131386302572423 ) ) ;
#39271 = CARTESIAN_POINT ( 'NONE',  ( 27.36219212280431989, -278.4805209788416391, -301.4846348637938149 ) ) ;
#39272 = ORIENTED_EDGE ( 'NONE', *, *, #9884, .T. ) ;
#39273 = VERTEX_POINT ( 'NONE', #6539 ) ;
#39274 = FACE_OUTER_BOUND ( 'NONE', #49551, .T. ) ;
#39275 = CARTESIAN_POINT ( 'NONE',  ( -72.49505816637696398, -290.6088331526117372, -334.6920397291250993 ) ) ;
#39276 = CARTESIAN_POINT ( 'NONE',  ( -72.68242731066128215, -291.2736709485791380, -337.6438508129793377 ) ) ;
#39277 = CARTESIAN_POINT ( 'NONE',  ( -109.8000173480027968, -290.0331828083702703, -260.3068860336741750 ) ) ;
#39278 = CARTESIAN_POINT ( 'NONE',  ( -68.47010882348477878, -285.1616790808510586, -199.9866153932235875 ) ) ;
#39279 = CARTESIAN_POINT ( 'NONE',  ( 196.7383257810085695, 24.47698789593440694, 10.99999999999999112 ) ) ;
#39280 = CARTESIAN_POINT ( 'NONE',  ( 22.44823254245317301, -280.5509465998648579, -313.6447904709196450 ) ) ;
#39281 = CARTESIAN_POINT ( 'NONE',  ( -15.46541120563776417, -290.6265462162186850, -341.3535031152059105 ) ) ;
#39282 = CARTESIAN_POINT ( 'NONE',  ( -70.54448389114365625, -281.9779698152066203, -336.1649177699672464 ) ) ;
#39283 = CARTESIAN_POINT ( 'NONE',  ( 11.62199682767608344, -282.0640414943837868, -215.5541854168594398 ) ) ;
#39284 = CARTESIAN_POINT ( 'NONE',  ( 19.45824493826854251, -289.1975058586792784, -322.0197022495066221 ) ) ;
#39285 = CARTESIAN_POINT ( 'NONE',  ( -102.2134076509238554, -279.5025225748929074, -236.6407266879552367 ) ) ;
#39286 = CARTESIAN_POINT ( 'NONE',  ( -113.6099547600766044, -289.4438718525689751, -262.6615319410354914 ) ) ;
#39287 = CARTESIAN_POINT ( 'NONE',  ( -78.44473344933318515, -286.3166699123464696, -205.4404011655635429 ) ) ;
#39288 = CARTESIAN_POINT ( 'NONE',  ( -36.57234973182783477, -286.5539098866731820, -193.4134744558207046 ) ) ;
#39289 = CARTESIAN_POINT ( 'NONE',  ( -108.9790853781976381, -284.5336390521810586, -284.3998158941558927 ) ) ;
#39290 = ORIENTED_EDGE ( 'NONE', *, *, #12262, .F. ) ;
#39291 = CARTESIAN_POINT ( 'NONE',  ( 144.2857639756989272, -299.5541904835127980, -189.2068768330456123 ) ) ;
#39292 = CARTESIAN_POINT ( 'NONE',  ( -47.59998609859089669, -293.7836280128283306, -195.2410608317548792 ) ) ;
#39293 = CARTESIAN_POINT ( 'NONE',  ( -11.24129318960841672, -293.4039942207975287, -342.3344044683004199 ) ) ;
#39294 = CARTESIAN_POINT ( 'NONE',  ( 29.36366256375835704, -275.0170223632680404, -300.5902932201364592 ) ) ;
#39295 = CARTESIAN_POINT ( 'NONE',  ( -30.60815077471541912, -294.3177082494300407, -346.9638078808094974 ) ) ;
#39296 = CONICAL_SURFACE ( 'NONE', #16616, 4.999999999999990230, 1.029744258676648538 ) ;
#39297 = CARTESIAN_POINT ( 'NONE',  ( -107.6574253200685547, -289.3220798146726906, -248.2640183937235179 ) ) ;
#39298 = CARTESIAN_POINT ( 'NONE',  ( 17.82105747384601813, -292.4884735886940916, -319.7263859475435197 ) ) ;
#39299 = CARTESIAN_POINT ( 'NONE',  ( -38.92142805470328426, -293.2369742287043550, -196.9810459899228476 ) ) ;
#39300 = DIRECTION ( 'NONE',  ( 0.000000000000000000, 1.000000000000000000, 0.000000000000000000 ) ) ;
#39301 = CARTESIAN_POINT ( 'NONE',  ( -14.40115280315599655, -290.3485889834909131, -198.7260271446300237 ) ) ;
#39302 = CIRCLE ( 'NONE', #4589, 24.00000000000001066 ) ;
#39303 = CARTESIAN_POINT ( 'NONE',  ( 17.46314378952469326, -296.2697726892754986, -321.6357982095648254 ) ) ;
#39304 = CARTESIAN_POINT ( 'NONE',  ( -21.06542623132290615, -289.7793954503864029, -341.7648388618358126 ) ) ;
#39305 = CARTESIAN_POINT ( 'NONE',  ( -5.946555528809022384, -278.6214061465901750, -338.8647799437262051 ) ) ;
#39306 = CARTESIAN_POINT ( 'NONE',  ( -94.92251092261561496, -276.6598835008269361, -320.8829840158118145 ) ) ;
#39307 = CARTESIAN_POINT ( 'NONE',  ( -0.08755179755317563095, -273.8829805189726585, -203.0747441809488691 ) ) ;
#39308 = CARTESIAN_POINT ( 'NONE',  ( 32.70139175005581933, -279.9629629010212852, -295.7181358301613159 ) ) ;
#39309 = CARTESIAN_POINT ( 'NONE',  ( -39.95612857935881124, -275.4843307480408043, -346.5291870796427247 ) ) ;
#39310 = CARTESIAN_POINT ( 'NONE',  ( -110.2230550656959736, -295.3659986220739597, -260.5141729916349504 ) ) ;
#39311 = CARTESIAN_POINT ( 'NONE',  ( -103.9471565363187437, -275.0099693548993969, -235.7717892038255627 ) ) ;
#39312 = CARTESIAN_POINT ( 'NONE',  ( -108.0408062550929316, -273.4509941876315224, -251.5785169547469309 ) ) ;
#39313 = B_SPLINE_CURVE_WITH_KNOTS ( 'NONE', 3,
 ( #32695, #48276, #12308, #34101 ),
 .UNSPECIFIED., .F., .F.,
 ( 4, 4 ),
 ( 6.973502068242161363E-17, 0.001032852107770819081 ),
 .UNSPECIFIED. ) ;
#39314 = CARTESIAN_POINT ( 'NONE',  ( 209.3503997127169214, 0.03340139000135424613, 7.446935725088736469 ) ) ;
#39316 = CARTESIAN_POINT ( 'NONE',  ( 26.63754940813002037, -274.9040520871092212, -235.1038649520244519 ) ) ;
#39315 = CARTESIAN_POINT ( 'NONE',  ( -51.40362738262570730, -287.2512183850509473, -344.3926585705142429 ) ) ;
#39317 = CARTESIAN_POINT ( 'NONE',  ( -23.31193716973744401, -288.8776533954240335, -346.1263001555414007 ) ) ;
#39318 = CARTESIAN_POINT ( 'NONE',  ( -80.22584383435339817, -275.4735302329809770, -208.5649068823958032 ) ) ;
#39319 = CARTESIAN_POINT ( 'NONE',  ( -106.6697043890098087, -294.1838755843298827, -298.5330232998869064 ) ) ;
#39320 = CARTESIAN_POINT ( 'NONE',  ( -55.67358304561735594, -282.4794958268097389, -344.9808264294359219 ) ) ;
#39321 = DIRECTION ( 'NONE',  ( -0.000000000000000000, -1.000000000000000000, -0.000000000000000000 ) ) ;
#39322 = CARTESIAN_POINT ( 'NONE',  ( -111.2935469783898554, -276.7133963233690110, -257.7905639762915371 ) ) ;
#39323 = CYLINDRICAL_SURFACE ( 'NONE', #68619, 1.000000000000000888 ) ;
#39324 = CARTESIAN_POINT ( 'NONE',  ( -95.41922696600950360, -289.9755429035691350, -225.4820428757223283 ) ) ;
#39325 = CARTESIAN_POINT ( 'NONE',  ( 73.43068321062709458, -134.2391364535880598, 5.025000000000002132 ) ) ;
#39326 = DIRECTION ( 'NONE',  ( -0.000000000000000000, 1.000000000000000000, -0.000000000000000000 ) ) ;
#39327 = CARTESIAN_POINT ( 'NONE',  ( -37.53008654365596186, -290.0496729215050777, -195.3485651561823033 ) ) ;
#39328 = CARTESIAN_POINT ( 'NONE',  ( -31.30200224120455843, -275.6499083600147628, -196.9029277449011488 ) ) ;
#39329 = CARTESIAN_POINT ( 'NONE',  ( -24.61372194124369273, -284.3181932555432354, -345.7580688073879287 ) ) ;
#39331 = CARTESIAN_POINT ( 'NONE',  ( -90.74146049882578779, -283.8363703792340402, -320.1352638049352208 ) ) ;
#39330 = CARTESIAN_POINT ( 'NONE',  ( 24.16914792535496659, -273.0394208769029660, -226.4558368042394818 ) ) ;
#39332 = CARTESIAN_POINT ( 'NONE',  ( -21.82736098460249607, -275.6801792865140328, -198.4258679561123699 ) ) ;
#39333 = CARTESIAN_POINT ( 'NONE',  ( -5.246425846308414798, -275.2885298001637580, -204.6015794358588948 ) ) ;
#39334 = CARTESIAN_POINT ( 'NONE',  ( -31.75906638102517121, -284.9818726717181221, -345.1659850968312639 ) ) ;
#39335 = ADVANCED_FACE ( 'NONE', ( #57205 ), #2172, .F. ) ;
#39336 = EDGE_LOOP ( 'NONE', ( #84928, #37732, #50799, #8347 ) ) ;
#39337 = CARTESIAN_POINT ( 'NONE',  ( 203.9781100709074906, 292.2290856633177327, -53.99999999998790656 ) ) ;
#39338 = CARTESIAN_POINT ( 'NONE',  ( 29.57361841262769886, -293.8814194832198723, -308.5652814451379982 ) ) ;
#39339 = CARTESIAN_POINT ( 'NONE',  ( -60.51260985763347833, -287.7300306075464960, -199.4036959377695837 ) ) ;
#39340 = DIRECTION ( 'NONE',  ( -0.7981962569173468580, -5.551115123125764401E-14, 0.6023974895724060197 ) ) ;
#39341 = CARTESIAN_POINT ( 'NONE',  ( -119.3990491898856732, -288.0523547857347353, -270.3284710469131937 ) ) ;
#39342 = CARTESIAN_POINT ( 'NONE',  ( -112.0206741183781531, -277.5219310159710631, -288.5051951738792582 ) ) ;
#39343 = CARTESIAN_POINT ( 'NONE',  ( -76.73802342891927708, -289.9343341773857787, -205.0747402354498945 ) ) ;
#39344 = CARTESIAN_POINT ( 'NONE',  ( -97.14874021825423256, -286.6689279724830612, -227.2835070044734209 ) ) ;
#39345 = CARTESIAN_POINT ( 'NONE',  ( -7.073009339664039885, -278.4096030137305320, -337.9020712899364867 ) ) ;
#39346 = CARTESIAN_POINT ( 'NONE',  ( 2.418795387446579959, -287.9993242518474972, -205.1099931741326827 ) ) ;
#39347 = CARTESIAN_POINT ( 'NONE',  ( -31.97792536911539685, -284.9846209709714344, -345.1690759134061750 ) ) ;
#39348 = CARTESIAN_POINT ( 'NONE',  ( -48.49188936316339493, -277.3568926635672369, -346.6034186737189202 ) ) ;
#39349 = CARTESIAN_POINT ( 'NONE',  ( -54.13331621003629124, -277.0952148529740384, -345.5625591572148778 ) ) ;
#39350 = CARTESIAN_POINT ( 'NONE',  ( -111.8154482312025237, -298.4934762073689285, -268.7251782247659548 ) ) ;
#39351 = FACE_BOUND ( 'NONE', #3795, .T. ) ;
#39352 = EDGE_CURVE ( 'NONE', #40992, #29264, #71882, .T. ) ;
#39353 = CARTESIAN_POINT ( 'NONE',  ( 195.5881128153457098, 0.000000000000000000, 21.50000000000000000 ) ) ;
#39354 = CIRCLE ( 'NONE', #74128, 203.9779373800640485 ) ;
#39355 = CARTESIAN_POINT ( 'NONE',  ( 7.109802698612255334, -296.7425731821555814, -194.6102166994000982 ) ) ;
#39356 = CARTESIAN_POINT ( 'NONE',  ( 193.6552470326849402, 275.0000000000000568, 16.89672165344822119 ) ) ;
#39357 = CARTESIAN_POINT ( 'NONE',  ( -70.48631613441757793, -277.0091378617260034, -335.4719686269543217 ) ) ;
#39358 = CARTESIAN_POINT ( 'NONE',  ( -18.66173394645513639, -275.4924843028174450, -196.0159471884904292 ) ) ;
#39359 = CONICAL_SURFACE ( 'NONE', #72, 8.500000000000007105, 0.7853981633974591592 ) ;
#39360 = CARTESIAN_POINT ( 'NONE',  ( 37.91250760616882332, -280.8009992371690942, -285.5144817020773758 ) ) ;
#39361 = CARTESIAN_POINT ( 'NONE',  ( -16.91340317285666472, -288.0795991765610324, -199.1692346478915852 ) ) ;
#39362 = CARTESIAN_POINT ( 'NONE',  ( -108.7815380698851868, -297.7282887020181761, -297.3253355459070804 ) ) ;
#39363 = CARTESIAN_POINT ( 'NONE',  ( -93.38843113568697163, -297.0414993757552793, -322.5989414986647716 ) ) ;
#39364 = CARTESIAN_POINT ( 'NONE',  ( -55.48079342112846746, -293.8183571034266492, -197.7594532776019776 ) ) ;
#39365 = CARTESIAN_POINT ( 'NONE',  ( -34.21177587356489624, -278.0914102176075744, -195.5804055599008393 ) ) ;
#39366 = CARTESIAN_POINT ( 'NONE',  ( 34.11005880877600305, -283.2014305034372228, -249.4814545779736363 ) ) ;
#39367 = CARTESIAN_POINT ( 'NONE',  ( -107.8520031293320471, -270.8908921432557690, -245.8632819064056321 ) ) ;
#39368 = CARTESIAN_POINT ( 'NONE',  ( -113.5408757646612656, -286.1567666718097485, -270.0060888298507962 ) ) ;
#39369 = CARTESIAN_POINT ( 'NONE',  ( 35.96415068357816835, -286.4815592327109357, -271.0527171521861192 ) ) ;
#39370 = CARTESIAN_POINT ( 'NONE',  ( 38.32378069700226320, -281.0733851889031030, -284.1472664677301623 ) ) ;
#39371 = CARTESIAN_POINT ( 'NONE',  ( 104.8672404336123662, 115.1756038169428820, -282.3939451955034201 ) ) ;
#39372 = ORIENTED_EDGE ( 'NONE', *, *, #20462, .T. ) ;
#39373 = CARTESIAN_POINT ( 'NONE',  ( 23.55404352819028446, -286.6588602852423264, -229.9732141583376972 ) ) ;
#39374 = ORIENTED_EDGE ( 'NONE', *, *, #66535, .F. ) ;
#39375 = CARTESIAN_POINT ( 'NONE',  ( -111.1900897473225882, -285.3715620525608756, -291.0470518728193952 ) ) ;
#39376 = CARTESIAN_POINT ( 'NONE',  ( 22.48559948038277057, -276.4701542840274442, -312.3141692455732255 ) ) ;
#39377 = CARTESIAN_POINT ( 'NONE',  ( 0.1031674301827133072, -285.3340557518053515, -203.5188271791187731 ) ) ;
#39378 = EDGE_CURVE ( 'NONE', #76413, #90266, #91342, .T. ) ;
#39379 = CARTESIAN_POINT ( 'NONE',  ( -96.33225375960206804, -290.1343310065495871, -221.3346342840754062 ) ) ;
#39380 = CARTESIAN_POINT ( 'NONE',  ( 19.94508063452825652, -281.7982973283400838, -219.2429714974994681 ) ) ;
#39381 = CARTESIAN_POINT ( 'NONE',  ( 194.7453183674699915, 19.99999999999999645, -15.62499999999999112 ) ) ;
#39382 = CARTESIAN_POINT ( 'NONE',  ( -90.58835705372274560, -280.8346987716189460, -215.6293970588049831 ) ) ;
#39383 = CARTESIAN_POINT ( 'NONE',  ( 37.84579318765830180, -282.0927320991972351, -286.9321597870633127 ) ) ;
#39384 = CARTESIAN_POINT ( 'NONE',  ( -92.08974858914540107, -281.4094976428775112, -313.9805196606274080 ) ) ;
#39385 = CARTESIAN_POINT ( 'NONE',  ( -83.35433501583091243, -219.9715334812069614, -352.6155196686340787 ) ) ;
#39386 = ORIENTED_EDGE ( 'NONE', *, *, #75203, .T. ) ;
#39387 = CARTESIAN_POINT ( 'NONE',  ( 35.96552309920986090, -277.7458007094012373, -285.3970566872844188 ) ) ;
#39388 = CARTESIAN_POINT ( 'NONE',  ( -84.73245238795870193, -218.9744008934607677, -352.0618779874953930 ) ) ;
#39389 = CARTESIAN_POINT ( 'NONE',  ( 16.46206323133144878, -278.8410301536602560, -218.5474991839913343 ) ) ;
#39390 = CARTESIAN_POINT ( 'NONE',  ( -47.27840444084209537, -297.2712796092406506, -197.8863971304570839 ) ) ;
#39391 = CARTESIAN_POINT ( 'NONE',  ( -92.76339991600542589, -290.7916625009636959, -216.9190290128747733 ) ) ;
#39392 = CARTESIAN_POINT ( 'NONE',  ( 161.2494399300530290, -11.64849832608277325, -3.999999999999998224 ) ) ;
#39394 = CARTESIAN_POINT ( 'NONE',  ( 33.44300810395984058, -285.6782063436313024, -249.4367087552971896 ) ) ;
#39393 = CARTESIAN_POINT ( 'NONE',  ( -113.8479272357090224, -271.2730514282568492, -267.4953093779189999 ) ) ;
#39395 = CARTESIAN_POINT ( 'NONE',  ( 32.96332416060278803, -295.0992764220783329, -246.3670528101350783 ) ) ;
#39396 = CARTESIAN_POINT ( 'NONE',  ( -19.71367887470570679, -287.5987801801365435, -199.0134036303937535 ) ) ;
#39397 = EDGE_LOOP ( 'NONE', ( #29074, #61580, #6089, #31975 ) ) ;
#39398 = CARTESIAN_POINT ( 'NONE',  ( 29.26551624276460828, -293.9960542012869382, -232.1996329519579660 ) ) ;
#39399 = CARTESIAN_POINT ( 'NONE',  ( -90.78219977634950055, -284.3286381202823350, -320.1818108625622585 ) ) ;
#39400 = CARTESIAN_POINT ( 'NONE',  ( -114.0320774532610812, -271.5085161411282684, -267.4914475766567534 ) ) ;
#39401 = CARTESIAN_POINT ( 'NONE',  ( -50.54867280931357953, -292.6904255554932206, -194.6661069670267352 ) ) ;
#39402 = CARTESIAN_POINT ( 'NONE',  ( -108.3127885092914369, -291.4226761038412974, -240.6520029324727830 ) ) ;
#39403 = CARTESIAN_POINT ( 'NONE',  ( 3.616363193716710445, -288.6510550656896612, -330.8491941804259113 ) ) ;
#39404 = VERTEX_POINT ( 'NONE', #7004 ) ;
#39405 = CARTESIAN_POINT ( 'NONE',  ( 212.4629471475955427, 32.98517505407394168, 13.08022668053247095 ) ) ;
#39406 = CARTESIAN_POINT ( 'NONE',  ( -88.78725214128012055, -299.1998239713085468, -214.6693415879454960 ) ) ;
#39407 = CARTESIAN_POINT ( 'NONE',  ( -112.6749436771190602, -271.5252420894163379, -256.1889733280397650 ) ) ;
#39408 = CARTESIAN_POINT ( 'NONE',  ( 34.71480816512652723, -280.7839039600362412, -283.5182673523386256 ) ) ;
#39409 = ORIENTED_EDGE ( 'NONE', *, *, #49120, .F. ) ;
#39410 = ORIENTED_EDGE ( 'NONE', *, *, #48459, .T. ) ;
#39411 = CARTESIAN_POINT ( 'NONE',  ( -48.49127145023283703, -276.6979715578750643, -346.5412725406817458 ) ) ;
#39412 = CARTESIAN_POINT ( 'NONE',  ( -99.01732784681938426, -295.5868639402693816, -229.9348940629868423 ) ) ;
#39413 = CARTESIAN_POINT ( 'NONE',  ( -89.94464095535288095, -279.6646816932357638, -322.8153463981730056 ) ) ;
#39414 = CARTESIAN_POINT ( 'NONE',  ( -21.65022116096443838, -272.3950198152109010, -197.8032585511467971 ) ) ;
#39415 = CARTESIAN_POINT ( 'NONE',  ( -44.62366856959528860, -299.1631778943439031, -197.2755151012489137 ) ) ;
#39416 = CARTESIAN_POINT ( 'NONE',  ( -109.5828009065488402, -297.7956066439823530, -257.8931818092237904 ) ) ;
#39417 = CARTESIAN_POINT ( 'NONE',  ( -113.5382024664509402, -298.1615101387588425, -269.6307449282184621 ) ) ;
#39418 = CARTESIAN_POINT ( 'NONE',  ( -77.93385925765447553, -271.5296901496937494, -206.8734544676563871 ) ) ;
#39419 = CARTESIAN_POINT ( 'NONE',  ( 34.42602821600245733, -294.3867119136889983, -284.2638456570648486 ) ) ;
#39420 = CARTESIAN_POINT ( 'NONE',  ( -32.09732282844340290, -290.6942902907457551, -196.9462744039742859 ) ) ;
#39421 = CARTESIAN_POINT ( 'NONE',  ( 73.43068321062709458, -134.2641364535880939, 0.000000000000000000 ) ) ;
#39422 = CARTESIAN_POINT ( 'NONE',  ( -2.590953013314785114, -274.9916180478309116, -201.7030557405360867 ) ) ;
#39423 = CARTESIAN_POINT ( 'NONE',  ( -35.81928768007912112, -298.4050094559723334, -197.3398847052345388 ) ) ;
#39424 = CARTESIAN_POINT ( 'NONE',  ( -85.80301146869595641, -282.3921359563429405, -329.5624657254462591 ) ) ;
#39425 = FACE_OUTER_BOUND ( 'NONE', #6035, .T. ) ;
#39426 = CARTESIAN_POINT ( 'NONE',  ( -45.66797648873498616, -282.3574050291476851, -343.0983647735912427 ) ) ;
#39427 = CARTESIAN_POINT ( 'NONE',  ( -111.3369149988693465, -282.3789735844816278, -283.8662294229106919 ) ) ;
#39428 = ADVANCED_FACE ( 'NONE', ( #36333 ), #55094, .F. ) ;
#39429 = CARTESIAN_POINT ( 'NONE',  ( 18.74582431062491850, -274.7988787307726284, -318.0010646748665977 ) ) ;
#39430 = CARTESIAN_POINT ( 'NONE',  ( 32.35641970274551937, -283.9146217680333848, -298.1977297619083629 ) ) ;
#39431 = CARTESIAN_POINT ( 'NONE',  ( 61.37083282337847123, -250.8548725835408391, -21.50000000000000000 ) ) ;
#39432 = FACE_OUTER_BOUND ( 'NONE', #88048, .T. ) ;
#39433 = CARTESIAN_POINT ( 'NONE',  ( -35.52224807768872239, -272.4744712586767150, -194.1698466212318408 ) ) ;
#39434 = CARTESIAN_POINT ( 'NONE',  ( -108.8145862638233581, -280.8541387049481841, -246.9222601696184825 ) ) ;
#39435 = CARTESIAN_POINT ( 'NONE',  ( 219.8344101925596021, 35.72494958537217968, -7.000000000000000000 ) ) ;
#39436 = CARTESIAN_POINT ( 'NONE',  ( -71.07352685953270566, -285.4140054913966082, -337.9738243863387765 ) ) ;
#39437 = CARTESIAN_POINT ( 'NONE',  ( 158.9078607026157499, 16.88031981475993959, -10.36078569760457491 ) ) ;
#39438 = CARTESIAN_POINT ( 'NONE',  ( -86.29322184692237840, -287.7308180053328215, -327.2508025193205299 ) ) ;
#39439 = CARTESIAN_POINT ( 'NONE',  ( 140.6539576904058606, 275.5000000000000568, -12.50000000000000000 ) ) ;
#39440 = CARTESIAN_POINT ( 'NONE',  ( -90.70643078340208376, -294.6245137195579105, -320.8261543529608844 ) ) ;
#39441 = CARTESIAN_POINT ( 'NONE',  ( -40.02613873826641822, -287.2256944840024744, -344.5981888845363983 ) ) ;
#39442 = CARTESIAN_POINT ( 'NONE',  ( -94.07136297056315755, -227.2831051785662737, -345.8935872616412439 ) ) ;
#39443 = CARTESIAN_POINT ( 'NONE',  ( -112.2402595566569801, -294.5019180862730082, -274.2606617501634219 ) ) ;
#39444 = CARTESIAN_POINT ( 'NONE',  ( -101.9213024232333140, -283.5691575445194417, -229.7140674216624916 ) ) ;
#39445 = CARTESIAN_POINT ( 'NONE',  ( -1.596244285866922130, -282.1345257086524043, -205.7956256302265672 ) ) ;
#39446 = CARTESIAN_POINT ( 'NONE',  ( -0.8816117824729906571, -280.8148015125112238, -337.0439616038644317 ) ) ;
#39447 = CARTESIAN_POINT ( 'NONE',  ( -31.87135465118553412, -288.9813445993796108, -343.2064891216612068 ) ) ;
#39448 = CARTESIAN_POINT ( 'NONE',  ( 34.33017151230868791, -282.7590313300437401, -253.6722673727451820 ) ) ;
#39449 = CARTESIAN_POINT ( 'NONE',  ( 34.72438982383177830, -282.1889724468341569, -257.7484098556087133 ) ) ;
#39450 = CARTESIAN_POINT ( 'NONE',  ( 20.80456886803262861, -288.8739467082240822, -222.4297273436147577 ) ) ;
#39451 = CARTESIAN_POINT ( 'NONE',  ( -29.06176134435187564, -298.3198158566332836, -193.3608907624496283 ) ) ;
#39452 = EDGE_LOOP ( 'NONE', ( #25431, #60983, #64404, #4012 ) ) ;
#39453 = CARTESIAN_POINT ( 'NONE',  ( -93.17216557534000287, -273.2770318234245224, -217.3139676789490409 ) ) ;
#39454 = CARTESIAN_POINT ( 'NONE',  ( 20.60709865574768784, -294.8807720032332327, -223.2900503420511598 ) ) ;
#39455 = FACE_OUTER_BOUND ( 'NONE', #75250, .T. ) ;
#39456 = CARTESIAN_POINT ( 'NONE',  ( -20.19161114001083490, -279.3376638359844719, -345.3538533559490702 ) ) ;
#39457 = ORIENTED_EDGE ( 'NONE', *, *, #25669, .F. ) ;
#39458 = CARTESIAN_POINT ( 'NONE',  ( 22.05334534205814734, -274.1823983539516689, -316.4499450874267836 ) ) ;
#39459 = DIRECTION ( 'NONE',  ( 0.9998346970812741485, 0.000000000000000000, -0.01818181818182024179 ) ) ;
#39460 = CARTESIAN_POINT ( 'NONE',  ( -113.1494281489257503, -294.8544379786490595, -278.0830857777785923 ) ) ;
#39461 = CARTESIAN_POINT ( 'NONE',  ( -36.72689055191467133, -273.4086625487323090, -197.2493374621504358 ) ) ;
#39462 = CARTESIAN_POINT ( 'NONE',  ( -108.4257412633100301, -292.3266485621357447, -250.9248927945805860 ) ) ;
#39463 = CARTESIAN_POINT ( 'NONE',  ( 20.15320880504508239, -283.9628890537467214, -316.9891425258840059 ) ) ;
#39464 = CARTESIAN_POINT ( 'NONE',  ( -81.60394424953923931, -292.8878585811157791, -208.0758064170695150 ) ) ;
#39465 = CARTESIAN_POINT ( 'NONE',  ( -99.63928747872814995, -292.4593067683714480, -225.9504336414273098 ) ) ;
#39466 = CARTESIAN_POINT ( 'NONE',  ( 35.64185255868094515, -293.4267605252102271, -273.4910876524156720 ) ) ;
#39467 = CARTESIAN_POINT ( 'NONE',  ( 28.80610798149704621, -290.0225726947860494, -305.8195370953117731 ) ) ;
#39468 = CARTESIAN_POINT ( 'NONE',  ( 33.56675751606402969, -282.1023878138273631, -300.5137983929928964 ) ) ;
#39469 = CARTESIAN_POINT ( 'NONE',  ( -98.73696105212438567, -295.2268209213725072, -226.3164118804131135 ) ) ;
#39470 = CARTESIAN_POINT ( 'NONE',  ( -33.06086875028397998, -282.8329825812398894, -347.2551640514894871 ) ) ;
#39471 = CARTESIAN_POINT ( 'NONE',  ( 35.19065165195718947, -277.7601887854273173, -288.0475296649000825 ) ) ;
#39472 = CARTESIAN_POINT ( 'NONE',  ( -74.74732862405285516, -275.6841686836183385, -336.2483279547302004 ) ) ;
#39473 = DIRECTION ( 'NONE',  ( 1.000000000000000000, 0.000000000000000000, 0.000000000000000000 ) ) ;
#39474 = CARTESIAN_POINT ( 'NONE',  ( -38.89266775796220088, -282.5797451354689542, -343.4186940332111249 ) ) ;
#39475 = CARTESIAN_POINT ( 'NONE',  ( -68.52501057723200972, -280.8565210478287213, -200.3781700284350791 ) ) ;
#39476 = CARTESIAN_POINT ( 'NONE',  ( 18.46550512483153028, -287.3329708841433785, -323.0714211002008938 ) ) ;
#39477 = CARTESIAN_POINT ( 'NONE',  ( 20.11850829645359084, -294.6610565969639310, -223.6902672264335763 ) ) ;
#39478 = CARTESIAN_POINT ( 'NONE',  ( 21.12999181155816331, -277.8166928310874937, -319.2231856773271375 ) ) ;
#39479 = CARTESIAN_POINT ( 'NONE',  ( 39.13744086591733407, -276.8414087900904406, -268.3021706118074121 ) ) ;
#39480 = CARTESIAN_POINT ( 'NONE',  ( -90.96929360578974411, -277.6734542073776311, -319.9632383244808125 ) ) ;
#39481 = CARTESIAN_POINT ( 'NONE',  ( -72.54952591492519787, -299.5851584090474944, -204.3129529917309810 ) ) ;
#39482 = CARTESIAN_POINT ( 'NONE',  ( -3.749311614363324718, -284.4963017828312104, -203.4912453617877190 ) ) ;
#39483 = CARTESIAN_POINT ( 'NONE',  ( 4.212312833704223713, -294.1755038163753966, -335.2236302310901692 ) ) ;
#39484 = CARTESIAN_POINT ( 'NONE',  ( -57.06398587337482553, -290.9024232745837821, -344.0191233604846843 ) ) ;
#39485 = EDGE_CURVE ( 'NONE', #48324, #68290, #83801, .T. ) ;
#39486 = CARTESIAN_POINT ( 'NONE',  ( 35.60436343034251649, -292.3702979548440908, -262.5827232592980636 ) ) ;
#39487 = CARTESIAN_POINT ( 'NONE',  ( 14.89360017505270228, -292.4801586074845545, -219.2635910995844313 ) ) ;
#39488 = ORIENTED_EDGE ( 'NONE', *, *, #67721, .T. ) ;
#39489 = CARTESIAN_POINT ( 'NONE',  ( -103.5246886435165692, -291.1242876625852887, -309.2127964404897966 ) ) ;
#39490 = CARTESIAN_POINT ( 'NONE',  ( -107.3271000201876006, -279.4827603638244113, -249.2439100650014154 ) ) ;
#39491 = EDGE_CURVE ( 'NONE', #64985, #9910, #9729, .T. ) ;
#39492 = CARTESIAN_POINT ( 'NONE',  ( -112.3059315314913249, -295.2692924983359717, -286.5430993583566419 ) ) ;
#39493 = CARTESIAN_POINT ( 'NONE',  ( -99.26709784780788937, -285.8110466102579039, -224.6822880096740391 ) ) ;
#39494 = CARTESIAN_POINT ( 'NONE',  ( 39.55626317759415400, -287.8285666947950290, -265.8154133698561736 ) ) ;
#39495 = CARTESIAN_POINT ( 'NONE',  ( -109.4426836976394384, -285.0388752939804249, -258.7261244418466504 ) ) ;
#39496 = CARTESIAN_POINT ( 'NONE',  ( -78.32199257514537294, -208.3160289897915618, -357.0357957823952688 ) ) ;
#39497 = CARTESIAN_POINT ( 'NONE',  ( 183.6448409953721068, 263.3645142227682641, -152.5370271569391605 ) ) ;
#39498 = CARTESIAN_POINT ( 'NONE',  ( 200.3489741029065101, 290.3571495942200613, -82.34907451253036470 ) ) ;
#39499 = AXIS2_PLACEMENT_3D ( 'NONE', #52891, #24017, #16920 ) ;
#39500 = CARTESIAN_POINT ( 'NONE',  ( -97.78799147175118378, -277.1771591182297811, -311.5781968440978176 ) ) ;
#39501 = CARTESIAN_POINT ( 'NONE',  ( -43.24563289694334856, -276.0487820814591373, -343.4321084754016624 ) ) ;
#39502 = CARTESIAN_POINT ( 'NONE',  ( -73.24632235394444990, -297.0970792890462349, -202.2553899741700150 ) ) ;
#39503 = CARTESIAN_POINT ( 'NONE',  ( 186.0019925103573826, 260.3827756688246495, -151.4387398898385300 ) ) ;
#39504 = CARTESIAN_POINT ( 'NONE',  ( -73.87618826675560513, -276.2117220566859714, -337.5960332078474266 ) ) ;
#39505 = CARTESIAN_POINT ( 'NONE',  ( -29.91010277892296543, -275.9076503794852897, -196.7218256594801460 ) ) ;
#39506 = CARTESIAN_POINT ( 'NONE',  ( -96.60486256646255754, -290.4474137011943640, -313.0912714994801149 ) ) ;
#39507 = CARTESIAN_POINT ( 'NONE',  ( -93.55162380140724565, -298.0713291434958023, -217.8945343081029478 ) ) ;
#39508 = CARTESIAN_POINT ( 'NONE',  ( -99.87519521369294750, -297.6389324643556051, -225.5382566759741962 ) ) ;
#39509 = CARTESIAN_POINT ( 'NONE',  ( -69.72216010194318869, -295.6575341551252905, -335.7866926183041869 ) ) ;
#39510 = ORIENTED_EDGE ( 'NONE', *, *, #62017, .T. ) ;
#39511 = CARTESIAN_POINT ( 'NONE',  ( 5.083347969299850000, -278.4035571443839672, -332.8865487279412037 ) ) ;
#39512 = CARTESIAN_POINT ( 'NONE',  ( -18.93919614269879048, -282.3291811168978711, -345.1212832107209465 ) ) ;
#39513 = CARTESIAN_POINT ( 'NONE',  ( -53.99582515532129179, -278.2123704211160771, -341.7299628314298161 ) ) ;
#39514 = CARTESIAN_POINT ( 'NONE',  ( 35.10338877093467147, -277.6043020401518788, -293.2888982509517177 ) ) ;
#39515 = CARTESIAN_POINT ( 'NONE',  ( -40.52544210569926975, -296.5860943348123442, -196.8281392923204578 ) ) ;
#39516 = CARTESIAN_POINT ( 'NONE',  ( 196.1347706148621057, 72.64529849370360637, -11.79135490535123942 ) ) ;
#39517 = CARTESIAN_POINT ( 'NONE',  ( -91.29824953101562812, -279.4239033647737074, -221.1910988546306100 ) ) ;
#39518 = CARTESIAN_POINT ( 'NONE',  ( -1.386125550053831201, -275.3195223355920120, -202.4541560592924156 ) ) ;
#39519 = CARTESIAN_POINT ( 'NONE',  ( 38.18538596417830178, -286.3946528426932900, -282.8875900945142803 ) ) ;
#39520 = CARTESIAN_POINT ( 'NONE',  ( -24.52705601584984052, -276.2157303281430245, -196.4112334349327114 ) ) ;
#39521 = CARTESIAN_POINT ( 'NONE',  ( 31.31779611622292236, -274.5621408734106694, -304.0148409389797166 ) ) ;
#39522 = CARTESIAN_POINT ( 'NONE',  ( 205.7786681169002350, 32.98517505407394168, 10.00000000000000000 ) ) ;
#39523 = CARTESIAN_POINT ( 'NONE',  ( -82.65426739764424724, -288.8870834772864100, -327.8012866266201968 ) ) ;
#39524 = CARTESIAN_POINT ( 'NONE',  ( -112.1219757187193409, -283.6755994814863016, -288.3395832999151480 ) ) ;
#39525 = CARTESIAN_POINT ( 'NONE',  ( 24.97164517709344622, -280.3380760612016616, -310.3930068161527629 ) ) ;
#39527 = CARTESIAN_POINT ( 'NONE',  ( -111.4250203434557704, -282.7327101095763737, -262.5756090973935670 ) ) ;
#39526 = CARTESIAN_POINT ( 'NONE',  ( 33.68704139694921196, -279.8741471083410488, -251.0698688757379102 ) ) ;
#39528 = CARTESIAN_POINT ( 'NONE',  ( 20.26165323421227882, -290.2158563739235433, -318.4105624031598154 ) ) ;
#39529 = CARTESIAN_POINT ( 'NONE',  ( -94.75408410926364411, -279.1147150926993277, -316.1080809135002028 ) ) ;
#39530 = CARTESIAN_POINT ( 'NONE',  ( 153.8045584215660710, 20.39561363287349849, -12.88435682625986267 ) ) ;
#39531 = CARTESIAN_POINT ( 'NONE',  ( 35.70586767038074072, -280.2290987185073163, -292.2333273351335379 ) ) ;
#39532 = CARTESIAN_POINT ( 'NONE',  ( -14.36976991830608519, -296.7544549676699148, -341.7564334400602206 ) ) ;
#39533 = CARTESIAN_POINT ( 'NONE',  ( -36.73779531599069514, -278.2995094804257405, -194.3639735198903225 ) ) ;
#39534 = CARTESIAN_POINT ( 'NONE',  ( -36.45662826106128307, -277.6922210603075882, -343.4701778058862374 ) ) ;
#39535 = CARTESIAN_POINT ( 'NONE',  ( -64.56390392834998693, -285.4068306245200120, -340.4390952921592088 ) ) ;
#39536 = EDGE_CURVE ( 'NONE', #83322, #92884, #38442, .T. ) ;
#39537 = ADVANCED_FACE ( 'NONE', ( #63854 ), #42976, .F. ) ;
#39538 = DIRECTION ( 'NONE',  ( 1.000000000000000000, 0.000000000000000000, 0.000000000000000000 ) ) ;
#39539 = CARTESIAN_POINT ( 'NONE',  ( -110.6044890883900962, -292.7086618137713003, -251.8189914200655721 ) ) ;
#39540 = CARTESIAN_POINT ( 'NONE',  ( 39.19480708611742159, -286.6568534857642589, -262.9829575811123732 ) ) ;
#39541 = CARTESIAN_POINT ( 'NONE',  ( -44.35617560996669084, -290.3619624410597453, -196.8438500617731961 ) ) ;
#39542 = CARTESIAN_POINT ( 'NONE',  ( -43.35412708609305099, -267.5894485949402224, -434.2348519691648221 ) ) ;
#39543 = CARTESIAN_POINT ( 'NONE',  ( 3.393623833971007198, -275.1765498547301831, -331.5320004258667836 ) ) ;
#39544 = CARTESIAN_POINT ( 'NONE',  ( 22.30503788460377024, -292.3011106193121122, -314.5553724384204202 ) ) ;
#39545 = DIRECTION ( 'NONE',  ( -0.000000000000000000, 1.000000000000000000, -0.000000000000000000 ) ) ;
#39546 = CARTESIAN_POINT ( 'NONE',  ( 38.16870806871002486, -291.8887970428065159, -259.0111584744097399 ) ) ;
#39547 = CARTESIAN_POINT ( 'NONE',  ( -110.2142911208002687, -286.3055179672390977, -258.6179202281561516 ) ) ;
#39548 = CARTESIAN_POINT ( 'NONE',  ( 17.89263496086532257, -286.5142137692236588, -322.5448533879898037 ) ) ;
#39549 = CARTESIAN_POINT ( 'NONE',  ( -33.22369036685279298, -287.5301557072505148, -196.8369752689445704 ) ) ;
#39550 = CARTESIAN_POINT ( 'NONE',  ( 208.4306832106270804, -124.2391364535881024, 0.000000000000000000 ) ) ;
#39551 = CARTESIAN_POINT ( 'NONE',  ( 35.43397495977787770, -288.2562236379149567, -262.8575959919190268 ) ) ;
#39552 = CARTESIAN_POINT ( 'NONE',  ( -9.150464633899238365, -294.3988370069307052, -200.4779222555517038 ) ) ;
#39553 = CARTESIAN_POINT ( 'NONE',  ( -74.64693530627204154, -275.6244402020410575, -336.0698208081736311 ) ) ;
#39554 = AXIS2_PLACEMENT_3D ( 'NONE', #14543, #86946, #43850 ) ;
#39555 = CARTESIAN_POINT ( 'NONE',  ( -111.8059065654491349, -278.6405037740643138, -289.9276711227866485 ) ) ;
#39556 = CARTESIAN_POINT ( 'NONE',  ( 34.09927956404828819, -291.3141040677170963, -245.5956636797952513 ) ) ;
#39557 = CARTESIAN_POINT ( 'NONE',  ( -111.7310279967723403, -278.8016461197647686, -250.4298744472197598 ) ) ;
#39558 = CARTESIAN_POINT ( 'NONE',  ( -108.2775947103428535, -298.8355497049901146, -246.9603479777366886 ) ) ;
#39559 = CARTESIAN_POINT ( 'NONE',  ( -43.28560281309416524, -274.0583670422044520, -506.4787804120613828 ) ) ;
#39560 = CARTESIAN_POINT ( 'NONE',  ( -111.9822501674346142, -282.6527165842720137, -262.5162098752384168 ) ) ;
#39561 = CARTESIAN_POINT ( 'NONE',  ( -48.18343439339133027, -265.6166469183427807, -497.0604155083162823 ) ) ;
#39562 = CARTESIAN_POINT ( 'NONE',  ( -110.5074648862690907, -276.5278871823754798, -282.9917234980234184 ) ) ;
#39563 = CARTESIAN_POINT ( 'NONE',  ( 20.06237325652579884, -280.2192876587023420, -318.6288402295327273 ) ) ;
#39564 = DIRECTION ( 'NONE',  ( 0.000000000000000000, 0.000000000000000000, 1.000000000000000000 ) ) ;
#39565 = CARTESIAN_POINT ( 'NONE',  ( 23.80040341266763804, -274.6449210392831901, -316.0158102821628177 ) ) ;
#39566 = VECTOR ( 'NONE', #35414, 1000.000000000000000 ) ;
#39567 = CARTESIAN_POINT ( 'NONE',  ( -68.79585177553632036, -296.9933984051726270, -337.0183883640967224 ) ) ;
#39568 = CARTESIAN_POINT ( 'NONE',  ( -0.5359154468656786019, -281.4951614167088110, -337.6576926782354349 ) ) ;
#39569 = CARTESIAN_POINT ( 'NONE',  ( -102.7478552766864226, -297.9404755921403876, -237.3021005556155671 ) ) ;
#39570 = CARTESIAN_POINT ( 'NONE',  ( -98.70698364546758796, -298.4791566786168460, -224.6489826538643229 ) ) ;
#39571 = CARTESIAN_POINT ( 'NONE',  ( 15.46501485645788421, -274.4909083938114804, -219.8544147194975267 ) ) ;
#39572 = CARTESIAN_POINT ( 'NONE',  ( 36.29268740888299050, -295.7352411305830628, -284.6081395539021628 ) ) ;
#39573 = CARTESIAN_POINT ( 'NONE',  ( 38.78525149925633997, -287.5731310874433007, -258.7110261510833311 ) ) ;
#39574 = CARTESIAN_POINT ( 'NONE',  ( -5.820619020157095314, -274.7817193097764630, -339.2576123025530705 ) ) ;
#39575 = CARTESIAN_POINT ( 'NONE',  ( -105.1569721839799172, -289.9139449501035415, -306.8315015899572700 ) ) ;
#39576 = CARTESIAN_POINT ( 'NONE',  ( 31.19903599478780620, -286.2660291231490532, -244.4191415195332979 ) ) ;
#39577 = CARTESIAN_POINT ( 'NONE',  ( -95.02391647623375093, -289.2139908503600623, -222.4062975314594723 ) ) ;
#39578 = ORIENTED_EDGE ( 'NONE', *, *, #12627, .F. ) ;
#39579 = CARTESIAN_POINT ( 'NONE',  ( 198.0538618622170191, 70.37887259939165574, 10.53035661854988270 ) ) ;
#39580 = CARTESIAN_POINT ( 'NONE',  ( 19.55746676059235867, -287.7072381380466481, -316.1920382139415437 ) ) ;
#39581 = CARTESIAN_POINT ( 'NONE',  ( 175.2296996224750103, 275.0000000000000568, 24.00000000000000355 ) ) ;
#39582 = CARTESIAN_POINT ( 'NONE',  ( -112.7693390258945527, -285.6757783252675722, -255.8192634680230810 ) ) ;
#39583 = CARTESIAN_POINT ( 'NONE',  ( 39.20733441517335649, -292.5387666794915731, -264.6108551255226189 ) ) ;
#39584 = CARTESIAN_POINT ( 'NONE',  ( -19.95873125215370791, -281.8719504599476977, -196.1161337112993692 ) ) ;
#39585 = CARTESIAN_POINT ( 'NONE',  ( -31.13060539442625796, -281.4441023927697074, -194.0544495326429058 ) ) ;
#39586 = CARTESIAN_POINT ( 'NONE',  ( -53.69173315707597993, -283.1010384103417437, -341.5586623051245851 ) ) ;
#39587 = CARTESIAN_POINT ( 'NONE',  ( 17.06581591602746428, -278.2765412748610743, -321.9830401343415360 ) ) ;
#39588 = CARTESIAN_POINT ( 'NONE',  ( -106.5133198205408434, -296.9865379864292549, -236.5338061011563866 ) ) ;
#39589 = CARTESIAN_POINT ( 'NONE',  ( -93.30008874856969214, -274.5406000743387835, -222.6981953964760237 ) ) ;
#39590 = CARTESIAN_POINT ( 'NONE',  ( 28.95877907738960388, -291.1161866959914732, -236.0669018985278456 ) ) ;
#39591 = UNCERTAINTY_MEASURE_WITH_UNIT (LENGTH_MEASURE( 1.000000000000000082E-05 ), #78729, 'distance_accuracy_value', 'NONE');
#39592 = CARTESIAN_POINT ( 'NONE',  ( -84.26217448119713538, -296.3096047027069631, -213.9681678806313130 ) ) ;
#39593 = ORIENTED_EDGE ( 'NONE', *, *, #47455, .T. ) ;
#39594 = CARTESIAN_POINT ( 'NONE',  ( -83.63170945779074827, -373.0521521680024648, -521.1711561948568487 ) ) ;
#39595 = CARTESIAN_POINT ( 'NONE',  ( -110.3458981331085482, -286.6605318393076232, -255.8111601022635568 ) ) ;
#39596 = CARTESIAN_POINT ( 'NONE',  ( -24.94417792124987798, -295.9773838221981350, -346.0971585270480091 ) ) ;
#39597 = CARTESIAN_POINT ( 'NONE',  ( -110.4114593512874194, -285.2321374479657834, -268.1924882522145026 ) ) ;
#39598 = CARTESIAN_POINT ( 'NONE',  ( -4.107595489404640254, -275.6833631239210831, -339.5732192568361825 ) ) ;
#39599 = CARTESIAN_POINT ( 'NONE',  ( -27.86988528739975379, -292.8206873134328134, -193.9950161240570594 ) ) ;
#39600 = CARTESIAN_POINT ( 'NONE',  ( -7.802488213262869898, -284.5745774425386116, -200.5361680304797289 ) ) ;
#39601 = EDGE_CURVE ( 'NONE', #77887, #1585, #49608, .T. ) ;
#39602 = CARTESIAN_POINT ( 'NONE',  ( -0.8176332796311546192, -292.8569861591918198, -202.5987624123526984 ) ) ;
#39603 = CARTESIAN_POINT ( 'NONE',  ( -48.05989454545237294, -289.5254125194103949, -342.6423960824848791 ) ) ;
#39604 = CARTESIAN_POINT ( 'NONE',  ( 222.8344101925596306, -44.55766379199611293, 22.08578643762690419 ) ) ;
#39605 = CARTESIAN_POINT ( 'NONE',  ( -109.5186219979625974, -268.8715237626327053, -295.3229297537549201 ) ) ;
#39606 = CARTESIAN_POINT ( 'NONE',  ( -99.21482380618097352, -285.4737047574824942, -315.1083697265177079 ) ) ;
#39607 = CARTESIAN_POINT ( 'NONE',  ( -19.05039376806006857, -277.7666405000204577, -190.3683826091709363 ) ) ;
#39608 = ORIENTED_EDGE ( 'NONE', *, *, #37667, .T. ) ;
#39609 = CARTESIAN_POINT ( 'NONE',  ( 33.94753095691120137, -280.6976765370531552, -287.5045854713155791 ) ) ;
#39610 = CARTESIAN_POINT ( 'NONE',  ( -108.4914965712454915, -278.5924476445994173, -240.9765853583650141 ) ) ;
#39611 = CARTESIAN_POINT ( 'NONE',  ( -6.024868469727883813, -282.4648206990967765, -202.3818130691016961 ) ) ;
#39612 = CARTESIAN_POINT ( 'NONE',  ( 140.6027560640470142, 178.2755120123287611, -239.6641268871332500 ) ) ;
#39613 = CARTESIAN_POINT ( 'NONE',  ( -61.06609947409423711, -281.9288151696048317, -343.0508027466426597 ) ) ;
#39614 = CARTESIAN_POINT ( 'NONE',  ( 36.19206204641257330, -285.4029588444121259, -257.2380762053180661 ) ) ;
#39615 = CARTESIAN_POINT ( 'NONE',  ( -75.29349592602395091, -299.3140378956080667, -204.4703696497196859 ) ) ;
#39616 = CARTESIAN_POINT ( 'NONE',  ( -31.59126198278418940, -295.4700904781654458, -343.2461613136113669 ) ) ;
#39618 = ORIENTED_EDGE ( 'NONE', *, *, #88318, .T. ) ;
#39617 = EDGE_CURVE ( 'NONE', #13346, #78803, #67202, .T. ) ;
#39619 = CARTESIAN_POINT ( 'NONE',  ( 17.11479098862842108, -291.5338982140329449, -220.9333012391132343 ) ) ;
#39620 = CARTESIAN_POINT ( 'NONE',  ( -2.763504090707678884, -277.2585595331883610, -339.0610095549510561 ) ) ;
#39621 = CARTESIAN_POINT ( 'NONE',  ( -51.56145966796525215, -273.8653203209354956, -198.7076633503091330 ) ) ;
#39622 = CARTESIAN_POINT ( 'NONE',  ( 34.90511988341609850, -274.8002694296607729, -296.2447807844613976 ) ) ;
#39623 = DIRECTION ( 'NONE',  ( 0.000000000000000000, 1.000000000000000000, -0.000000000000000000 ) ) ;
#39624 = CARTESIAN_POINT ( 'NONE',  ( 27.62765049496321268, -273.0507116727614516, -232.7887045907048389 ) ) ;
#39625 = CARTESIAN_POINT ( 'NONE',  ( -47.53486938215063873, -296.6045794102851119, -346.0889569348577766 ) ) ;
#39626 = CARTESIAN_POINT ( 'NONE',  ( 180.4306473129080359, 214.7033776542919270, -24.48382199637807943 ) ) ;
#39627 = CIRCLE ( 'NONE', #59343, 24.50000000000000355 ) ;
#39628 = DIRECTION ( 'NONE',  ( -0.000000000000000000, -0.000000000000000000, -1.000000000000000000 ) ) ;
#39629 = AXIS2_PLACEMENT_3D ( 'NONE', #83605, #9845, #1349 ) ;
#39630 = CARTESIAN_POINT ( 'NONE',  ( -82.97644637447366733, -284.7729323286050658, -327.7995511489230580 ) ) ;
#39631 = CARTESIAN_POINT ( 'NONE',  ( -2.084156676595279478, -284.3519597862401724, -337.6729270923661375 ) ) ;
#39632 = CARTESIAN_POINT ( 'NONE',  ( -82.86467103295676395, -283.0421262334570542, -327.6235596081834842 ) ) ;
#39633 = CARTESIAN_POINT ( 'NONE',  ( 12.27060056339095517, -274.7480859062198988, -325.0661477351733879 ) ) ;
#39634 = CARTESIAN_POINT ( 'NONE',  ( -53.94323939252092970, -285.1278082313111781, -342.7691370784489777 ) ) ;
#39635 = CARTESIAN_POINT ( 'NONE',  ( -68.34658320717315405, -275.9468758556681109, -337.2286067586991294 ) ) ;
#39636 = CIRCLE ( 'NONE', #92576, 35.00000000000002842 ) ;
#39637 = CARTESIAN_POINT ( 'NONE',  ( 34.19793077050955787, -276.8428787879513493, -286.4278464394835737 ) ) ;
#39638 = CARTESIAN_POINT ( 'NONE',  ( 194.2870706637141325, 39.56299966811847924, 14.58823529411763431 ) ) ;
#39639 = VECTOR ( 'NONE', #45039, 1000.000000000000000 ) ;
#39640 = CARTESIAN_POINT ( 'NONE',  ( -111.1849022949874524, -279.6219005887551248, -249.1163465217204021 ) ) ;
#39641 = ORIENTED_EDGE ( 'NONE', *, *, #62083, .F. ) ;
#39642 = CARTESIAN_POINT ( 'NONE',  ( 196.8865788344785699, 19.32388290151978438, 12.43054049968610997 ) ) ;
#39643 = CARTESIAN_POINT ( 'NONE',  ( -77.88185896896445115, -287.3740828116817738, -206.3548604724969948 ) ) ;
#39644 = CARTESIAN_POINT ( 'NONE',  ( -61.07519455262079333, -294.5653072566602191, -339.6197483953746428 ) ) ;
#39645 = CARTESIAN_POINT ( 'NONE',  ( -80.49028880831879462, -288.9685695071562463, -334.0769388608529766 ) ) ;
#39646 = CARTESIAN_POINT ( 'NONE',  ( 33.27376178377338789, -286.0837990396106534, -292.6997589782764635 ) ) ;
#39648 = CARTESIAN_POINT ( 'NONE',  ( -52.55648522724863625, -290.0945818635508431, -197.8758809785319386 ) ) ;
#39647 = CARTESIAN_POINT ( 'NONE',  ( -19.65681778267361324, -284.8587748896123344, -198.9284934201445196 ) ) ;
#39649 = CARTESIAN_POINT ( 'NONE',  ( -85.10863555245676082, -284.9342144054907067, -326.0876860077471520 ) ) ;
#39650 = CARTESIAN_POINT ( 'NONE',  ( -9.966185078670209307, -274.6945206846938277, -340.1864846127739384 ) ) ;
#39651 = CARTESIAN_POINT ( 'NONE',  ( -57.10328329638918632, -287.7026815511279096, -344.0085911247178387 ) ) ;
#39652 = CARTESIAN_POINT ( 'NONE',  ( -8.145820723512962047, -288.4345302531881430, -201.2219278970269158 ) ) ;
#39653 = CARTESIAN_POINT ( 'NONE',  ( 34.93560693069736089, -285.2848066327330798, -249.5358395156733593 ) ) ;
#39654 = CARTESIAN_POINT ( 'NONE',  ( -13.44128764559060585, -283.6754403573763170, -339.6404627502159315 ) ) ;
#39655 = CARTESIAN_POINT ( 'NONE',  ( -7.620811099606910943, -290.6636682921705415, -339.4162931606959432 ) ) ;
#39656 = PLANE ( 'NONE',  #70119 ) ;
#39657 = EDGE_CURVE ( 'NONE', #61737, #1911, #86848, .T. ) ;
#39658 = DIRECTION ( 'NONE',  ( -0.000000000000000000, 0.000000000000000000, -1.000000000000000000 ) ) ;
#39659 = CARTESIAN_POINT ( 'NONE',  ( -88.64879474235468138, -299.2595524808058371, -214.8204408018097524 ) ) ;
#39660 =( BOUNDED_CURVE ( )  B_SPLINE_CURVE ( 3, ( #41678, #92336, #6667, #56389 ),
 .UNSPECIFIED., .F., .F. ) 
 B_SPLINE_CURVE_WITH_KNOTS ( ( 4, 4 ),
 ( 3.141592653589779349, 4.712388980384689674 ),
 .UNSPECIFIED. ) 
 CURVE ( )  GEOMETRIC_REPRESENTATION_ITEM ( )  RATIONAL_B_SPLINE_CURVE ( ( 1.000000000000000000, 0.8047378541243617178, 0.8047378541243617178, 1.000000000000000000 ) ) 
 REPRESENTATION_ITEM ( '' )  );
#39661 = CARTESIAN_POINT ( 'NONE',  ( -30.04307726684865543, -278.1442228730077773, -195.6653560981789894 ) ) ;
#39662 = CARTESIAN_POINT ( 'NONE',  ( 8.762224741406479112, -291.8630777705416222, -208.8244934466491998 ) ) ;
#39663 = CARTESIAN_POINT ( 'NONE',  ( -110.8983861085746128, -294.8660274973246374, -276.9510221037945144 ) ) ;
#39664 = CARTESIAN_POINT ( 'NONE',  ( 34.12580315037016021, -280.4622120882492595, -287.5505193294093829 ) ) ;
#39665 = CARTESIAN_POINT ( 'NONE',  ( -32.57486717372825780, -272.1925185161367153, -196.0611216984173382 ) ) ;
#39666 = CARTESIAN_POINT ( 'NONE',  ( -9.025499807376524686, -295.9890977240772827, -338.1939611895390385 ) ) ;
#39667 = CARTESIAN_POINT ( 'NONE',  ( 22.62177241418591933, -301.3029683736232300, -195.3356572496892625 ) ) ;
#39668 = CARTESIAN_POINT ( 'NONE',  ( -87.63479199453202284, -271.9410463940280351, -212.7650420924811669 ) ) ;
#39670 =( BOUNDED_CURVE ( )  B_SPLINE_CURVE ( 3, ( #9281, #81264, #44810, #30155 ),
 .UNSPECIFIED., .F., .F. ) 
 B_SPLINE_CURVE_WITH_KNOTS ( ( 4, 4 ),
 ( 4.712388980384688786, 5.759586531581284419 ),
 .UNSPECIFIED. ) 
 CURVE ( )  GEOMETRIC_REPRESENTATION_ITEM ( )  RATIONAL_B_SPLINE_CURVE ( ( 1.000000000000000000, 0.9106836025229594345, 0.9106836025229594345, 1.000000000000000000 ) ) 
 REPRESENTATION_ITEM ( '' )  );
#39669 = CARTESIAN_POINT ( 'NONE',  ( 36.11120101886904621, -292.0388766214174439, -289.8199290694760180 ) ) ;
#39671 = FACE_OUTER_BOUND ( 'NONE', #1068, .T. ) ;
#39672 = CARTESIAN_POINT ( 'NONE',  ( 35.69517182657597232, -294.2883065242595535, -265.2949977014166052 ) ) ;
#39673 = EDGE_CURVE ( 'NONE', #26249, #76130, #72783, .T. ) ;
#39674 = DIRECTION ( 'NONE',  ( 0.000000000000000000, -1.000000000000000000, 0.000000000000000000 ) ) ;
#39676 = CARTESIAN_POINT ( 'NONE',  ( -34.30119463534659019, -295.0128625237863957, -343.2977708146487998 ) ) ;
#39675 = CARTESIAN_POINT ( 'NONE',  ( -19.33637210163773901, -280.8418754809615621, -343.5873989137619446 ) ) ;
#39677 = CARTESIAN_POINT ( 'NONE',  ( 17.82627695980227500, -282.2893252683851415, -324.1541018679840249 ) ) ;
#39678 = CARTESIAN_POINT ( 'NONE',  ( -113.5790427396694042, -284.0808196680319497, -281.3966533056985213 ) ) ;
#39679 = CARTESIAN_POINT ( 'NONE',  ( -110.1396696716633130, -288.3289069964955615, -287.6955940677410695 ) ) ;
#39680 = CARTESIAN_POINT ( 'NONE',  ( -27.48105051923313980, -281.4090623402646543, -346.0808686061739650 ) ) ;
#39681 = CARTESIAN_POINT ( 'NONE',  ( -26.20308914757249497, -287.8338521637489862, -346.2388080799579484 ) ) ;
#39682 = DIRECTION ( 'NONE',  ( -0.000000000000000000, -0.000000000000000000, -1.000000000000000000 ) ) ;
#39683 = CARTESIAN_POINT ( 'NONE',  ( -50.59509220362742354, -296.8243748854167734, -342.9613109005114779 ) ) ;
#39684 = CARTESIAN_POINT ( 'NONE',  ( 3.204342167205097791, -277.9444558263751333, -335.1893331159667468 ) ) ;
#39685 = CARTESIAN_POINT ( 'NONE',  ( -107.2461319274750338, -278.4982249338487463, -249.2552443545260417 ) ) ;
#39686 = CARTESIAN_POINT ( 'NONE',  ( -7.192158773138485728, -292.6035089675882546, -199.4948017430098730 ) ) ;
#39687 = CARTESIAN_POINT ( 'NONE',  ( -88.88572816199265958, -283.4151340673147388, -215.0402960077908574 ) ) ;
#39688 = CARTESIAN_POINT ( 'NONE',  ( -70.65889170467927727, -279.4917056388626975, -337.5546102152597427 ) ) ;
#39689 = CARTESIAN_POINT ( 'NONE',  ( 35.43936246825725789, -292.7238329486046950, -278.9499967125762510 ) ) ;
#39690 = AXIS2_PLACEMENT_3D ( 'NONE', #84388, #47937, #63131 ) ;
#39691 = CARTESIAN_POINT ( 'NONE',  ( -98.28124022598166221, -295.1468274312157973, -226.6418647505824140 ) ) ;
#39692 = ORIENTED_EDGE ( 'NONE', *, *, #55527, .F. ) ;
#39693 = LINE ( 'NONE', #69541, #49867 ) ;
#39694 = AXIS2_PLACEMENT_3D ( 'NONE', #6491, #84601, #21153 ) ;
#39695 = CARTESIAN_POINT ( 'NONE',  ( 35.76953186481645730, -293.0651450879711319, -270.7665164003734617 ) ) ;
#39696 = CARTESIAN_POINT ( 'NONE',  ( 140.6539576904058606, 249.5000000000000568, 12.50000000000000000 ) ) ;
#39697 = CARTESIAN_POINT ( 'NONE',  ( -109.1418805571601069, -294.0523547857346784, -270.3284710469131937 ) ) ;
#39698 = CARTESIAN_POINT ( 'NONE',  ( 19.18545054807930228, -297.8023799065100548, -193.6051735408791785 ) ) ;
#39699 = VECTOR ( 'NONE', #26074, 1000.000000000000000 ) ;
#39700 = CARTESIAN_POINT ( 'NONE',  ( 1.258312855294479782, -287.8715244392993213, -204.2903176100155065 ) ) ;
#39701 = CARTESIAN_POINT ( 'NONE',  ( -88.66257608494407805, -289.6306402131138498, -322.2761225141631485 ) ) ;
#39702 = AXIS2_PLACEMENT_3D ( 'NONE', #65376, #488, #43561 ) ;
#39703 = CARTESIAN_POINT ( 'NONE',  ( -110.1743798349186676, -279.9255328864710464, -281.5909229495017030 ) ) ;
#39704 = CARTESIAN_POINT ( 'NONE',  ( -72.16127415136023160, -299.3451779327166378, -205.0353799725195927 ) ) ;
#39705 = CARTESIAN_POINT ( 'NONE',  ( -70.64661801114796447, -276.2965246263129870, -335.7668742335099523 ) ) ;
#39706 = VERTEX_POINT ( 'NONE', #27373 ) ;
#39707 = CARTESIAN_POINT ( 'NONE',  ( -109.1658334348097270, -272.7386872876663801, -242.4601928849913008 ) ) ;
#39708 = CARTESIAN_POINT ( 'NONE',  ( -93.48193564286293622, -291.7880724401666725, -319.3215310150362143 ) ) ;
#39709 = CARTESIAN_POINT ( 'NONE',  ( 34.68962801281556096, -294.8338191310930370, -245.3433624781305582 ) ) ;
#39710 = CARTESIAN_POINT ( 'NONE',  ( -113.1465174729249270, -274.3934560397275391, -270.3845621914958883 ) ) ;
#39711 = CARTESIAN_POINT ( 'NONE',  ( -107.8523963470944409, -291.4580801992955230, -251.0703329511936772 ) ) ;
#39712 = CARTESIAN_POINT ( 'NONE',  ( -48.18343439339133738, -248.5908270566111753, -461.0970999203888141 ) ) ;
#39713 = ORIENTED_EDGE ( 'NONE', *, *, #5733, .F. ) ;
#39714 = CARTESIAN_POINT ( 'NONE',  ( 10.35979044841188035, -290.8416062541252813, -211.4304278360350793 ) ) ;
#39715 = CARTESIAN_POINT ( 'NONE',  ( -51.80080555010563614, -298.2054241824904466, -194.6980728815351540 ) ) ;
#39716 = CARTESIAN_POINT ( 'NONE',  ( -41.86541348196897872, -297.6602956599268168, -197.4802322559225445 ) ) ;
#39717 = CARTESIAN_POINT ( 'NONE',  ( 170.2297021224755724, 215.0000000000000568, -25.00499999999998835 ) ) ;
#39718 = CARTESIAN_POINT ( 'NONE',  ( 175.2296996224750103, 249.5000000000000568, 0.000000000000000000 ) ) ;
#39719 = CARTESIAN_POINT ( 'NONE',  ( -90.31864062599562715, -292.8394148066545313, -215.3682653294903275 ) ) ;
#39720 = CARTESIAN_POINT ( 'NONE',  ( 36.57525178469696669, -289.6233781216987495, -234.7283546768995564 ) ) ;
#39721 = CARTESIAN_POINT ( 'NONE',  ( -110.7318193497294345, -286.7405253257752520, -255.7351537302855888 ) ) ;
#39722 = CARTESIAN_POINT ( 'NONE',  ( 23.79292097534147032, -272.9641282565760889, -227.1812320932447165 ) ) ;
#39723 = CARTESIAN_POINT ( 'NONE',  ( -67.66607105041461523, -275.5713059889473584, -202.3637226577957051 ) ) ;
#39724 = CARTESIAN_POINT ( 'NONE',  ( 9.778903110907036123, -290.7860816474361627, -212.6664447397970150 ) ) ;
#39725 = CARTESIAN_POINT ( 'NONE',  ( -111.7870033245331172, -280.5923878887890623, -256.2131863788128499 ) ) ;
#39726 = VERTEX_POINT ( 'NONE', #92687 ) ;
#39727 = CARTESIAN_POINT ( 'NONE',  ( -51.04512795253646829, -282.5803749545330561, -342.2188167373320766 ) ) ;
#39728 = CARTESIAN_POINT ( 'NONE',  ( -109.4414312862656686, -279.2986155744231382, -296.6529795015550235 ) ) ;
#39729 = CARTESIAN_POINT ( 'NONE',  ( -17.08216137139889312, -279.1030095750335249, -196.4858189516522771 ) ) ;
#39730 = CARTESIAN_POINT ( 'NONE',  ( 137.1993315682407513, 179.5396152623583816, -238.8328485414318436 ) ) ;
#39731 = CARTESIAN_POINT ( 'NONE',  ( 35.84194613142251740, -276.7855449304253170, -293.5338203081345227 ) ) ;
#39732 = SHAPE_DEFINITION_REPRESENTATION ( #49709, #42162 ) ;
#39733 = CARTESIAN_POINT ( 'NONE',  ( -32.74389777622274522, -275.6291922407170887, -194.1800611126437843 ) ) ;
#39734 = CARTESIAN_POINT ( 'NONE',  ( -54.49178911615187815, -300.3376638359845856, -195.3683826091709363 ) ) ;
#39735 = ORIENTED_EDGE ( 'NONE', *, *, #62500, .T. ) ;
#39736 = VERTEX_POINT ( 'NONE', #27857 ) ;
#39737 = DIRECTION ( 'NONE',  ( 0.000000000000000000, 0.000000000000000000, 1.000000000000000000 ) ) ;
#39738 = CARTESIAN_POINT ( 'NONE',  ( -31.83446811926402731, -290.0608417822717229, -343.5139151645066136 ) ) ;
#39739 = CARTESIAN_POINT ( 'NONE',  ( 22.50343835863060704, -289.9466763791970152, -317.2065722804399002 ) ) ;
#39740 = CARTESIAN_POINT ( 'NONE',  ( -86.80444592184629471, -289.1103571408332300, -324.2566429272066557 ) ) ;
#39741 = CARTESIAN_POINT ( 'NONE',  ( -15.42497997227498630, -285.8359702797824866, -196.5549427593896894 ) ) ;
#39742 = FACE_OUTER_BOUND ( 'NONE', #42578, .T. ) ;
#39743 = CARTESIAN_POINT ( 'NONE',  ( -18.55140352823800853, -281.2060668890777606, -341.7819079804012290 ) ) ;
#39744 = CARTESIAN_POINT ( 'NONE',  ( 34.27982309166126385, -289.6684566812014623, -290.0770342393511214 ) ) ;
#39745 = CARTESIAN_POINT ( 'NONE',  ( -65.59928976714695636, -281.9083649889072944, -338.4352352226174503 ) ) ;
#39746 = CARTESIAN_POINT ( 'NONE',  ( -87.88183246933533610, -280.6432015741103783, -216.9340625338751067 ) ) ;
#39747 = CARTESIAN_POINT ( 'NONE',  ( 37.27853583509865842, -288.7200889668467312, -288.4344708695062423 ) ) ;
#39748 = CARTESIAN_POINT ( 'NONE',  ( -39.15300923662992005, -277.5678422768293672, -343.4002006790905170 ) ) ;
#39749 = CARTESIAN_POINT ( 'NONE',  ( -95.35013347247358695, -290.0263799320351836, -220.3107788947947370 ) ) ;
#39750 = CARTESIAN_POINT ( 'NONE',  ( -63.15682724680156213, -286.5271062904726591, -197.9888993338646799 ) ) ;
#39751 = CARTESIAN_POINT ( 'NONE',  ( -40.81997165677712758, -286.5019795035723291, -193.4491690200500784 ) ) ;
#39752 = CARTESIAN_POINT ( 'NONE',  ( -37.53839109535314833, -283.2213979392259375, -343.3732823468525908 ) ) ;
#39753 = EDGE_LOOP ( 'NONE', ( #30373, #64019 ) ) ;
#39754 = CARTESIAN_POINT ( 'NONE',  ( 194.1581894022642416, 20.00000000000000000, -14.79860320208535107 ) ) ;
#39755 = CARTESIAN_POINT ( 'NONE',  ( -110.7197263458815257, -292.1720032796042119, -289.2801411478302498 ) ) ;
#39756 = CIRCLE ( 'NONE', #36749, 0.9999999999999977796 ) ;
#39757 = CARTESIAN_POINT ( 'NONE',  ( -0.9555650506191690763, -293.2643335911649274, -337.6763333024496774 ) ) ;
#39758 = CARTESIAN_POINT ( 'NONE',  ( -32.66406834142569693, -273.1712625433654011, -197.2627920962744952 ) ) ;
#39759 = EDGE_CURVE ( 'NONE', #84950, #13726, #78504, .T. ) ;
#39760 = CARTESIAN_POINT ( 'NONE',  ( -65.57380561601503643, -294.7603512162481820, -341.9033653222387557 ) ) ;
#39761 = CARTESIAN_POINT ( 'NONE',  ( -93.06822552151373884, -289.7127123954507510, -222.1401461826363288 ) ) ;
#39762 = CARTESIAN_POINT ( 'NONE',  ( -96.42663509871108829, -294.1742092870052829, -314.9571589436030763 ) ) ;
#39763 = CIRCLE ( 'NONE', #59479, 5.568361562975243650 ) ;
#39764 = CARTESIAN_POINT ( 'NONE',  ( -101.4780791103513593, -292.2438030974962544, -234.5683815685820548 ) ) ;
#39765 = PLANE ( 'NONE',  #5160 ) ;
#39766 = AXIS2_PLACEMENT_3D ( 'NONE', #2419, #30357, #17078 ) ;
#39767 = CARTESIAN_POINT ( 'NONE',  ( 36.26989864591389079, -291.7468634837658783, -285.5716720862241687 ) ) ;
#39768 = CARTESIAN_POINT ( 'NONE',  ( -34.05362665422288160, -297.0110893642420820, -345.3392244205235784 ) ) ;
#39769 = CARTESIAN_POINT ( 'NONE',  ( 33.93655589983130483, -288.2715593302011712, -253.4897439839930371 ) ) ;
#39770 = CONICAL_SURFACE ( 'NONE', #3509, 2.395975569037533948, 0.09862129276975308001 ) ;
#39771 = CARTESIAN_POINT ( 'NONE',  ( 0.2488915315052253607, -278.5344535952655178, -335.7299933199262227 ) ) ;
#39772 = CARTESIAN_POINT ( 'NONE',  ( -6.747456131714818284, -275.4543248688745507, -340.6035053402041513 ) ) ;
#39773 = CARTESIAN_POINT ( 'NONE',  ( -29.07093834134551713, -297.3504034485424086, -193.5236867680119133 ) ) ;
#39774 = CARTESIAN_POINT ( 'NONE',  ( -10.91284753882835190, -274.9426332593550342, -339.4949719501360619 ) ) ;
#39775 = CARTESIAN_POINT ( 'NONE',  ( -95.04150366694798890, -277.2849096088735337, -223.3287156075291762 ) ) ;
#39776 = CARTESIAN_POINT ( 'NONE',  ( -41.36281958430816275, -275.5018334940079967, -346.4680198426538027 ) ) ;
#39777 = AXIS2_PLACEMENT_3D ( 'NONE', #76852, #11978, #63143 ) ;
#39778 = ADVANCED_FACE ( 'NONE', ( #1739 ), #87434, .T. ) ;
#39779 = DIRECTION ( 'NONE',  ( 0.000000000000000000, 0.000000000000000000, -1.000000000000000000 ) ) ;
#39780 = CARTESIAN_POINT ( 'NONE',  ( -63.35073241327500426, -274.3555528266676333, -202.0290649443586801 ) ) ;
#39781 = DIRECTION ( 'NONE',  ( -0.000000000000000000, 1.000000000000000000, -0.000000000000000000 ) ) ;
#39783 = CARTESIAN_POINT ( 'NONE',  ( -29.98775596008918853, -273.9811398031532690, -197.7324768712551304 ) ) ;
#39782 = CARTESIAN_POINT ( 'NONE',  ( -10.18022559315754982, -286.7194527106200326, -340.6509544034244072 ) ) ;
#39784 = VECTOR ( 'NONE', #52031, 1000.000000000000000 ) ;
#39785 = CARTESIAN_POINT ( 'NONE',  ( 39.34744552469121004, -287.6385955382169755, -277.2730597537149038 ) ) ;
#39786 = CARTESIAN_POINT ( 'NONE',  ( -35.54682324546423189, -300.0544014925458782, -195.0053073947756559 ) ) ;
#39787 = CARTESIAN_POINT ( 'NONE',  ( -89.80486420785283030, -293.7939382221726419, -323.7972950000556125 ) ) ;
#39788 = CARTESIAN_POINT ( 'NONE',  ( 33.41323309201952441, -281.1330312446541484, -300.4619046728660123 ) ) ;
#39789 = CARTESIAN_POINT ( 'NONE',  ( 201.2104617360081704, 41.21457449016151031, 10.00000000000000000 ) ) ;
#39790 = CARTESIAN_POINT ( 'NONE',  ( -26.48868791700703440, -278.1899538328263475, -196.0989576444739271 ) ) ;
#39791 = VECTOR ( 'NONE', #10834, 1000.000000000000000 ) ;
#39792 = CARTESIAN_POINT ( 'NONE',  ( 155.7140808774800007, 21.00000000000000000, 15.62500000000000000 ) ) ;
#39793 = CARTESIAN_POINT ( 'NONE',  ( -108.1127691114707545, -289.0891583803602884, -290.0058528152225676 ) ) ;
#39794 = CARTESIAN_POINT ( 'NONE',  ( 201.0592549708492243, 40.73798607845792930, 9.999999999999998224 ) ) ;
#39795 =( NAMED_UNIT ( * ) PLANE_ANGLE_UNIT ( ) SI_UNIT ( $, .RADIAN. ) );
#39796 = CARTESIAN_POINT ( 'NONE',  ( -47.23371169119993596, -289.9262888776588625, -196.0163215659109710 ) ) ;
#39797 = CARTESIAN_POINT ( 'NONE',  ( -43.55974445737484047, -275.4924468666928874, -196.8793887419329849 ) ) ;
#39798 = CARTESIAN_POINT ( 'NONE',  ( -4.401282570986539078, -284.0517898906515484, -339.3213841356649141 ) ) ;
#39800 = CARTESIAN_POINT ( 'NONE',  ( -24.06549518659920039, -282.8778344105186306, -342.1437229948592744 ) ) ;
#39799 = CARTESIAN_POINT ( 'NONE',  ( -107.8145378871846987, -270.9854956299136575, -242.9611489228998380 ) ) ;
#39801 = CARTESIAN_POINT ( 'NONE',  ( 15.86032821095262690, -276.2491782610504174, -219.4452743736653417 ) ) ;
#39802 = CARTESIAN_POINT ( 'NONE',  ( 34.86821958725052895, -276.5138298591160151, -282.4288300823610030 ) ) ;
#39803 = CARTESIAN_POINT ( 'NONE',  ( -46.97361172118782946, -285.1746618732933598, -344.7400593985273645 ) ) ;
#39804 = CARTESIAN_POINT ( 'NONE',  ( -40.51621138919293941, -297.0700364246780509, -197.1820682965733624 ) ) ;
#39805 = ORIENTED_EDGE ( 'NONE', *, *, #55943, .F. ) ;
#39806 = DIRECTION ( 'NONE',  ( -1.000000000000000000, -0.000000000000000000, 0.000000000000000000 ) ) ;
#39807 = CARTESIAN_POINT ( 'NONE',  ( 38.32563184522916799, -293.2070849189560704, -256.0973570282072842 ) ) ;
#39808 = CARTESIAN_POINT ( 'NONE',  ( -96.40272711318992549, -285.9032532665411850, -316.0289007689420941 ) ) ;
#39809 = DIRECTION ( 'NONE',  ( 0.9531768234071978929, -0.3024135303179465439, -0.000000000000000000 ) ) ;
#39810 = CARTESIAN_POINT ( 'NONE',  ( -88.52914483777347243, -275.1952119285919025, -334.4957818155094174 ) ) ;
#39811 = CARTESIAN_POINT ( 'NONE',  ( -113.8820721935425695, -277.8413357026964263, -263.0191635710657465 ) ) ;
#39812 = CARTESIAN_POINT ( 'NONE',  ( -113.3881522850110173, -289.0131285028289767, -265.5260866407580806 ) ) ;
#39813 = CARTESIAN_POINT ( 'NONE',  ( -33.44034290159669354, -284.5223116261956875, -343.9638035118141488 ) ) ;
#39814 = CARTESIAN_POINT ( 'NONE',  ( -35.06430666747245084, -278.7833057854938374, -344.3394086807946906 ) ) ;
#39815 = CARTESIAN_POINT ( 'NONE',  ( -46.45337606932299224, -287.3639393147903434, -194.4955549543988980 ) ) ;
#39816 = CARTESIAN_POINT ( 'NONE',  ( -27.31555767499168041, -282.1795958621367504, -195.9817001519840858 ) ) ;
#39817 = CARTESIAN_POINT ( 'NONE',  ( 31.24933441125983435, -275.2681994449073954, -235.3715483180508272 ) ) ;
#39818 = CARTESIAN_POINT ( 'NONE',  ( -28.60314493002260150, -276.7776896760775003, -346.9172268872580958 ) ) ;
#39820 = CARTESIAN_POINT ( 'NONE',  ( -89.49359142643116627, -297.7136211299420552, -323.5512755501623587 ) ) ;
#39819 = CONICAL_SURFACE ( 'NONE', #11124, 2.395975569037533948, 0.09862129276975308001 ) ;
#39821 = CARTESIAN_POINT ( 'NONE',  ( 156.1688672180385709, 17.06233518523205106, 10.31625060074216726 ) ) ;
#39822 = CARTESIAN_POINT ( 'NONE',  ( 152.6878475589607262, 19.85941866395974031, -8.897000670449973114 ) ) ;
#39823 = CARTESIAN_POINT ( 'NONE',  ( -51.54544036838969845, -296.0120801104989141, -195.8861563920898732 ) ) ;
#39824 = CARTESIAN_POINT ( 'NONE',  ( -100.6392797531233327, -277.5587018973620843, -306.9511625713876128 ) ) ;
#39825 = CARTESIAN_POINT ( 'NONE',  ( -31.30673008393911871, -275.3318181946322056, -193.9830712550185012 ) ) ;
#39826 = CARTESIAN_POINT ( 'NONE',  ( 36.13283947421767550, -289.4282842924586134, -279.2754908239335805 ) ) ;
#39827 = CARTESIAN_POINT ( 'NONE',  ( -41.88475481592588778, -296.6284003057389782, -346.5843498001004832 ) ) ;
#39828 = CARTESIAN_POINT ( 'NONE',  ( -113.9135278707518637, -297.8023800467317983, -266.7692820837592080 ) ) ;
#39829 = CARTESIAN_POINT ( 'NONE',  ( -112.1375019110005269, -292.5051888326643734, -274.0234576335558359 ) ) ;
#39830 = CARTESIAN_POINT ( 'NONE',  ( -54.89881208862858841, -277.8258897682926545, -197.5630188277108630 ) ) ;
#39831 = AXIS2_PLACEMENT_3D ( 'NONE', #51802, #15371, #74519 ) ;
#39832 = CARTESIAN_POINT ( 'NONE',  ( 5.736976495290038613, -282.5612118126936707, -209.6524545500743670 ) ) ;
#39833 = CARTESIAN_POINT ( 'NONE',  ( -105.0177499493420612, -295.0435134676999951, -239.2328409918157490 ) ) ;
#39834 = CARTESIAN_POINT ( 'NONE',  ( -68.65398484356734343, -285.3196887404208724, -339.3669378444746485 ) ) ;
#39835 = CARTESIAN_POINT ( 'NONE',  ( 33.33090819253290960, -286.2161143851173506, -250.8775734543809506 ) ) ;
#39836 = CARTESIAN_POINT ( 'NONE',  ( -54.34854212782089178, -170.4010203859631645, -363.8413129607317273 ) ) ;
#39837 = EDGE_LOOP ( 'NONE', ( #36526, #92299, #64421, #82263 ) ) ;
#39838 = CARTESIAN_POINT ( 'NONE',  ( 34.01757299924511813, -287.0145897466731526, -254.8710687375991313 ) ) ;
#39839 = EDGE_LOOP ( 'NONE', ( #6016, #32768 ) ) ;
#39840 = CARTESIAN_POINT ( 'NONE',  ( -30.22981603279387031, -284.0438337334412608, -346.7215371418542418 ) ) ;
#39841 = CIRCLE ( 'NONE', #92800, 0.5000000000000004441 ) ;
#39842 = CARTESIAN_POINT ( 'NONE',  ( -81.08706607163028934, -273.7728029653857220, -211.8303224405265155 ) ) ;
#39843 = CARTESIAN_POINT ( 'NONE',  ( -2.390312730128070662, -285.2990705822073778, -202.1818655209577003 ) ) ;
#39844 = VECTOR ( 'NONE', #24977, 1000.000000000000227 ) ;
#39845 = CARTESIAN_POINT ( 'NONE',  ( 10.66648957686888366, -281.6380748477394036, -210.3927946783440177 ) ) ;
#39846 = CARTESIAN_POINT ( 'NONE',  ( 169.2744399300530347, 8.542400036368780647, 10.00000000000000000 ) ) ;
#39847 = CARTESIAN_POINT ( 'NONE',  ( -59.12292222997164259, -281.2953699237994556, -197.2291406064128694 ) ) ;
#39848 = CARTESIAN_POINT ( 'NONE',  ( 38.85094398147693084, -282.0227129027796309, -281.3349630293132577 ) ) ;
#39849 = CARTESIAN_POINT ( 'NONE',  ( 30.89617123739170168, -285.2666405000203440, -285.9686137636504668 ) ) ;
#39850 = CARTESIAN_POINT ( 'NONE',  ( -47.70296038983430265, -155.1840385668599538, -365.3184360848422898 ) ) ;
#39851 = VERTEX_POINT ( 'NONE', #45270 ) ;
#39852 = CARTESIAN_POINT ( 'NONE',  ( -9.277769870770052663, -278.6846286850316119, -339.7468093962818898 ) ) ;
#39853 = CARTESIAN_POINT ( 'NONE',  ( 198.8369974573453192, 289.4883165844757968, -97.36247972072811763 ) ) ;
#39854 = CIRCLE ( 'NONE', #18733, 3.842139515347647638 ) ;
#39855 = CARTESIAN_POINT ( 'NONE',  ( 37.06645056988301690, -279.6568738698627499, -276.9202094849629816 ) ) ;
#39856 = CARTESIAN_POINT ( 'NONE',  ( -4.914356814633031867, -296.3911815409174437, -339.0954218122809607 ) ) ;
#39857 = CARTESIAN_POINT ( 'NONE',  ( -55.83709986365592215, -294.6450891098947977, -341.1370720201487643 ) ) ;
#39858 = CARTESIAN_POINT ( 'NONE',  ( -111.1713454743743341, -290.3315761753734705, -248.7113980921081122 ) ) ;
#39859 = DIRECTION ( 'NONE',  ( 1.000000000000000000, 0.000000000000000000, 0.000000000000000000 ) ) ;
#39861 = CARTESIAN_POINT ( 'NONE',  ( 32.14587634846064645, -286.2794187540621920, -295.2190569507674240 ) ) ;
#39860 = CARTESIAN_POINT ( 'NONE',  ( -112.0330643881362107, -294.9237475370731545, -286.4796290860215890 ) ) ;
#39862 = CARTESIAN_POINT ( 'NONE',  ( 20.67368585677700565, -296.0560761843204318, -316.6964045232886633 ) ) ;
#39863 = CARTESIAN_POINT ( 'NONE',  ( -107.4513170884046076, -285.5771229778363249, -292.4039192537188114 ) ) ;
#39864 = ORIENTED_EDGE ( 'NONE', *, *, #72960, .F. ) ;
#39865 = CARTESIAN_POINT ( 'NONE',  ( 22.91589289952115038, -293.8551077152234825, -222.7812833551403457 ) ) ;
#39866 = CARTESIAN_POINT ( 'NONE',  ( -104.6566933204832281, -285.4269383999828733, -241.8289387030356750 ) ) ;
#39867 = CARTESIAN_POINT ( 'NONE',  ( -81.65457398396021915, -294.4352005469737605, -332.9109350206140334 ) ) ;
#39868 = VECTOR ( 'NONE', #51027, 1000.000000000000114 ) ;
#39869 = CARTESIAN_POINT ( 'NONE',  ( -113.8470875312444406, -291.4514566630433023, -262.6633235361706511 ) ) ;
#39870 = CARTESIAN_POINT ( 'NONE',  ( -107.2071811897092601, -291.4584643097590515, -238.0108554379469012 ) ) ;
#39871 = CARTESIAN_POINT ( 'NONE',  ( -42.66179500164579252, -289.2876755957583441, -343.2176048613244461 ) ) ;
#39872 = ORIENTED_EDGE ( 'NONE', *, *, #22475, .T. ) ;
#39873 = DIRECTION ( 'NONE',  ( -0.000000000000000000, -0.000000000000000000, -1.000000000000000000 ) ) ;
#39874 = CARTESIAN_POINT ( 'NONE',  ( 7.062238062185569376, -300.4628266708469368, -194.5824113571880503 ) ) ;
#39875 = CARTESIAN_POINT ( 'NONE',  ( -49.64028476192080319, -272.6937164334059958, -194.6983753253464897 ) ) ;
#39876 = CARTESIAN_POINT ( 'NONE',  ( -51.86232481402274885, -278.9206433638852332, -198.5278881975040122 ) ) ;
#39877 = ORIENTED_EDGE ( 'NONE', *, *, #67912, .T. ) ;
#39878 = ADVANCED_FACE ( 'NONE', ( #15486 ), #52395, .F. ) ;
#39879 = CARTESIAN_POINT ( 'NONE',  ( 11.75125115413071164, -274.2202303522391844, -211.0516182497405850 ) ) ;
#39880 = CARTESIAN_POINT ( 'NONE',  ( -97.43702802450373213, -295.6220396974227356, -227.7083417737426316 ) ) ;
#39881 = CARTESIAN_POINT ( 'NONE',  ( -95.40457104334377902, -279.7699491780040830, -316.6368852998749617 ) ) ;
#39882 = CARTESIAN_POINT ( 'NONE',  ( 12.39131684248492959, -272.8926628506566203, -215.1784298547269429 ) ) ;
#39883 = CARTESIAN_POINT ( 'NONE',  ( -95.61362895822911412, -298.3818479192134987, -225.7142651774272508 ) ) ;
#39884 = CARTESIAN_POINT ( 'NONE',  ( -107.0048185663945475, -297.9354740795042176, -247.3686203846012575 ) ) ;
#39885 = DIRECTION ( 'NONE',  ( -0.000000000000000000, -0.000000000000000000, -1.000000000000000000 ) ) ;
#39886 = CARTESIAN_POINT ( 'NONE',  ( -110.8557563086801849, -298.4082980940353309, -250.1129179588720888 ) ) ;
#39887 = CARTESIAN_POINT ( 'NONE',  ( -96.50567071643585848, -271.2101287116694266, -223.6917341026262704 ) ) ;
#39888 = CARTESIAN_POINT ( 'NONE',  ( 33.21726461501619099, -294.4562650530234578, -289.5222139637552345 ) ) ;
#39889 = CARTESIAN_POINT ( 'NONE',  ( 22.29277605024654463, -291.5282874515282856, -227.2223528185431576 ) ) ;
#39890 = FACE_OUTER_BOUND ( 'NONE', #45668, .T. ) ;
#39891 = CARTESIAN_POINT ( 'NONE',  ( 22.70638377164603483, -275.3994269881756622, -222.2387259433414499 ) ) ;
#39892 = CARTESIAN_POINT ( 'NONE',  ( -60.52663324946901469, -298.0764108567388462, -201.0649693514104683 ) ) ;
#39893 = CARTESIAN_POINT ( 'NONE',  ( 34.59780140026816042, -283.2441020441747241, -247.9308945565724684 ) ) ;
#39894 = CARTESIAN_POINT ( 'NONE',  ( -76.51984852833768969, -282.2491880421223414, -336.1368618603453911 ) ) ;
#39895 = CARTESIAN_POINT ( 'NONE',  ( -75.29312218112123389, -276.8929762310203841, -337.2416259860366949 ) ) ;
#39896 = LINE ( 'NONE', #38519, #26120 ) ;
#39897 = CARTESIAN_POINT ( 'NONE',  ( -64.12398131338626683, -282.6078747705284968, -338.4442373411538370 ) ) ;
#39898 = CARTESIAN_POINT ( 'NONE',  ( 26.72865974338654382, -280.0792582641491322, -309.7664139892644926 ) ) ;
#39899 = EDGE_CURVE ( 'NONE', #26691, #6854, #16880, .T. ) ;
#39900 = CARTESIAN_POINT ( 'NONE',  ( 17.86534855371302655, -274.8163437526249595, -319.0376675416437706 ) ) ;
#39901 = CARTESIAN_POINT ( 'NONE',  ( -10.66344824300929162, -278.7044963706738940, -340.5099735875199940 ) ) ;
#39902 = DIRECTION ( 'NONE',  ( -1.000000000000000000, 0.000000000000000000, 0.000000000000000000 ) ) ;
#39903 = CARTESIAN_POINT ( 'NONE',  ( 195.4602890156073443, 20.04204674317102430, 14.69963036182647720 ) ) ;
#39904 = CARTESIAN_POINT ( 'NONE',  ( -103.5244894767228203, -271.4489132294216347, -232.4891674483793338 ) ) ;
#39905 = AXIS2_PLACEMENT_3D ( 'NONE', #5468, #6395, #34800 ) ;
#39906 = CARTESIAN_POINT ( 'NONE',  ( -102.0150896752214464, -280.0399051690092165, -308.7695419381665829 ) ) ;
#39907 = CARTESIAN_POINT ( 'NONE',  ( 152.4536156746142410, 275.0000000000000568, 11.50000000000000000 ) ) ;
#39908 = CARTESIAN_POINT ( 'NONE',  ( -82.99336479221003060, -285.5910860038545707, -330.6367910575937117 ) ) ;
#39909 = VERTEX_POINT ( 'NONE', #88376 ) ;
#39910 = CARTESIAN_POINT ( 'NONE',  ( 208.6643680990008534, 36.42852971205770984, 14.80559097128779911 ) ) ;
#39911 = CARTESIAN_POINT ( 'NONE',  ( 8.286716363009247743, -286.4281190546503808, -329.9493301367932077 ) ) ;
#39912 = DIRECTION ( 'NONE',  ( 0.000000000000000000, 0.000000000000000000, 1.000000000000000000 ) ) ;
#39913 = CARTESIAN_POINT ( 'NONE',  ( -80.40005331173402681, -294.4453725542026064, -329.8010769738037311 ) ) ;
#39914 = CARTESIAN_POINT ( 'NONE',  ( -72.97218697348505145, -287.6692207758283644, -335.4866420795630688 ) ) ;
#39915 = CARTESIAN_POINT ( 'NONE',  ( 157.0248177074734315, 17.42562647115670060, -9.460300111311761739 ) ) ;
#39916 = CARTESIAN_POINT ( 'NONE',  ( -102.9521984419405385, -295.0353824857957079, -234.0256923327315803 ) ) ;
#39917 = CARTESIAN_POINT ( 'NONE',  ( -60.28286420397969891, -284.2400137719881741, -197.5296040163914029 ) ) ;
#39918 = CARTESIAN_POINT ( 'NONE',  ( 31.81288479365725763, -282.8105580342979692, -244.4447926933517579 ) ) ;
#39919 = CARTESIAN_POINT ( 'NONE',  ( 10.83262658920518540, -280.6366957417903905, -329.1931955109091064 ) ) ;
#39920 = CARTESIAN_POINT ( 'NONE',  ( -98.11067330276347320, -289.9903813939259862, -310.8330020887377145 ) ) ;
#39921 = AXIS2_PLACEMENT_3D ( 'NONE', #45863, #44474, #80932 ) ;
#39922 = AXIS2_PLACEMENT_3D ( 'NONE', #64974, #77, #88080 ) ;
#39923 = CARTESIAN_POINT ( 'NONE',  ( -108.1904886280531599, -280.2388526553801853, -250.4190437213241864 ) ) ;
#39924 = CARTESIAN_POINT ( 'NONE',  ( -32.96354380183094435, -280.9115548554800625, -197.3307580329334314 ) ) ;
#39925 = CARTESIAN_POINT ( 'NONE',  ( 31.37552165241656255, -289.9356616415514054, -301.2860307649806941 ) ) ;
#39926 = ORIENTED_EDGE ( 'NONE', *, *, #22600, .F. ) ;
#39927 = AXIS2_PLACEMENT_3D ( 'NONE', #88580, #39300, #10899 ) ;
#39928 = CARTESIAN_POINT ( 'NONE',  ( -34.10319493175585848, -274.0918282862901378, -193.4292514765836017 ) ) ;
#39929 = CARTESIAN_POINT ( 'NONE',  ( -109.3450010223550350, -292.7863444923192446, -250.6793633558575038 ) ) ;
#39930 = CARTESIAN_POINT ( 'NONE',  ( 120.8395553409046528, -299.5541904835127980, -195.3611179825600175 ) ) ;
#39931 = CARTESIAN_POINT ( 'NONE',  ( -37.30987171927208124, -297.5519495502701375, -350.3611179825600175 ) ) ;
#39932 = EDGE_LOOP ( 'NONE', ( #57835, #77377 ) ) ;
#39933 = CARTESIAN_POINT ( 'NONE',  ( 36.42460406899568426, -273.3669764058590204, -255.9194839109920565 ) ) ;
#39934 = DIRECTION ( 'NONE',  ( -0.000000000000000000, -0.000000000000000000, -1.000000000000000000 ) ) ;
#39935 = CARTESIAN_POINT ( 'NONE',  ( -88.08801166768149926, -294.1478237462674770, -327.2759970417426416 ) ) ;
#39936 = CARTESIAN_POINT ( 'NONE',  ( -64.59910141930529903, -273.0352558882165113, -202.5174885453004663 ) ) ;
#39937 = CARTESIAN_POINT ( 'NONE',  ( -71.47688267531636086, -291.0316460661204587, -335.6861459932318326 ) ) ;
#39938 = CIRCLE ( 'NONE', #92888, 0.5000000000000004441 ) ;
#39939 = CARTESIAN_POINT ( 'NONE',  ( -40.25207304407012288, -284.8493794377538393, -344.3172113402604282 ) ) ;
#39940 = CARTESIAN_POINT ( 'NONE',  ( -73.17359136916491025, -293.0119222085804154, -202.8579474814561650 ) ) ;
#39941 = CARTESIAN_POINT ( 'NONE',  ( -73.21738478106122727, -292.9018417216164494, -202.7724006240360666 ) ) ;
#39942 = CARTESIAN_POINT ( 'NONE',  ( -9.725509357622222240, -292.2564084769883266, -202.7325883287784620 ) ) ;
#39943 = CARTESIAN_POINT ( 'NONE',  ( -47.00718327411643571, -287.9296857594567314, -195.9343640610834427 ) ) ;
#39944 = CARTESIAN_POINT ( 'NONE',  ( 39.41153979145496322, -281.6417979951140751, -264.2015590417603903 ) ) ;
#39945 = CARTESIAN_POINT ( 'NONE',  ( -112.1721864685637087, -294.7666823356152577, -259.7933638427709298 ) ) ;
#39946 = CARTESIAN_POINT ( 'NONE',  ( -34.48109616090975038, -282.8504461847399511, -347.3079629436462596 ) ) ;
#39947 = CARTESIAN_POINT ( 'NONE',  ( 31.68645494205470214, -277.1581030884285610, -241.8184552063757451 ) ) ;
#39948 = CARTESIAN_POINT ( 'NONE',  ( -21.33282851196159058, -291.3376638359844719, -340.3538533559490702 ) ) ;
#39949 = CARTESIAN_POINT ( 'NONE',  ( -48.33850316556904403, -275.3301231220715977, -345.3766458612280985 ) ) ;
#39950 = CARTESIAN_POINT ( 'NONE',  ( 185.2169494693457921, 250.5000000000000568, 22.91843887563416615 ) ) ;
#39951 = CARTESIAN_POINT ( 'NONE',  ( 1.128384709536257580, -282.0314394668641853, -332.5333217831845332 ) ) ;
#39952 = CARTESIAN_POINT ( 'NONE',  ( -111.7041864223648417, -279.9890994613726320, -251.9162434612984782 ) ) ;
#39953 = CARTESIAN_POINT ( 'NONE',  ( 21.30149730118791851, -287.2803279334011677, -319.8969192676487978 ) ) ;
#39954 = CARTESIAN_POINT ( 'NONE',  ( -22.55985524192942648, -294.0041234129637360, -197.8389070902159403 ) ) ;
#39955 = CARTESIAN_POINT ( 'NONE',  ( 32.96744214091626901, -276.7731805041838129, -240.8469596105385619 ) ) ;
#39956 = CARTESIAN_POINT ( 'NONE',  ( 37.11583154547785313, -277.0893658874636571, -288.0066386532004685 ) ) ;
#39957 = CARTESIAN_POINT ( 'NONE',  ( -36.46830422599426669, -276.8742602266501081, -343.3683603301077483 ) ) ;
#39958 = CARTESIAN_POINT ( 'NONE',  ( -83.08440284735091552, -299.4249573799679069, -211.0701488321134889 ) ) ;
#39959 = CARTESIAN_POINT ( 'NONE',  ( -110.7218213990089595, -282.7408513039162585, -255.6850751936578376 ) ) ;
#39960 = CARTESIAN_POINT ( 'NONE',  ( 22.19560467496934208, -292.5634420680644325, -221.5650768682015155 ) ) ;
#39961 = CARTESIAN_POINT ( 'NONE',  ( -23.43769816913287229, -290.4775242474386232, -345.3354248793496595 ) ) ;
#39962 = CARTESIAN_POINT ( 'NONE',  ( -4.683071405612477811, -291.4130872516424802, -204.7145191384604459 ) ) ;
#39963 = ORIENTED_EDGE ( 'NONE', *, *, #56745, .F. ) ;
#39964 = CARTESIAN_POINT ( 'NONE',  ( -58.75602935051295361, -290.3551797664517267, -197.0124111400807010 ) ) ;
#39965 = CARTESIAN_POINT ( 'NONE',  ( 6.692368853513653626, -292.3367851412401137, -212.1108969048224253 ) ) ;
#39966 = EDGE_LOOP ( 'NONE', ( #20299, #71251, #1124, #18518 ) ) ;
#39967 = CARTESIAN_POINT ( 'NONE',  ( -28.99709303471507482, -290.0285433223718314, -346.6499859984701857 ) ) ;
#39968 = CARTESIAN_POINT ( 'NONE',  ( -107.7186955520845686, -279.4651185866747483, -250.5417127838931322 ) ) ;
#39969 = EDGE_CURVE ( 'NONE', #46265, #42209, #67064, .T. ) ;
#39970 = CARTESIAN_POINT ( 'NONE',  ( -111.6724675631351005, -295.2346947412398777, -289.2935132128879445 ) ) ;
#39971 = CARTESIAN_POINT ( 'NONE',  ( -18.21541169642240732, -286.9436573448576837, -195.8245628828794054 ) ) ;
#39972 = B_SPLINE_CURVE_WITH_KNOTS ( 'NONE', 3,
 ( #55103, #55578, #20043, #19118, #5397, #84426, #34262, #63169 ),
 .UNSPECIFIED., .F., .F.,
 ( 4, 2, 2, 4 ),
 ( 0.000000000000000000, 0.0009268394340039834076, 0.001390259151005943669, 0.001853678868007904148 ),
 .UNSPECIFIED. ) ;
#39973 = CARTESIAN_POINT ( 'NONE',  ( 2.726382592704248431, -286.9075092234311910, -204.6321818997711830 ) ) ;
#39974 = CARTESIAN_POINT ( 'NONE',  ( -96.59446676261966047, -285.4822789304688513, -227.6642990782339950 ) ) ;
#39975 = CARTESIAN_POINT ( 'NONE',  ( -13.18397878099063014, -91.46032863585759287, -359.9971981747313521 ) ) ;
#39976 = CARTESIAN_POINT ( 'NONE',  ( 201.5604602716146871, 295.4035874922714697, -68.51738880406409749 ) ) ;
#39977 = CARTESIAN_POINT ( 'NONE',  ( 166.7545789058513037, 230.2666759795009739, -189.9084627180601501 ) ) ;
#39978 = CARTESIAN_POINT ( 'NONE',  ( 29.29714726640905909, -275.1554194970757976, -300.5582328177343356 ) ) ;
#39979 = CARTESIAN_POINT ( 'NONE',  ( 34.93271569847851055, -274.3102733244279534, -258.0131353880378811 ) ) ;
#39980 = CARTESIAN_POINT ( 'NONE',  ( -113.0774333050036518, -296.2294148263135298, -256.8102647436851953 ) ) ;
#39981 = CARTESIAN_POINT ( 'NONE',  ( -29.40099482351953597, -125.5565301473652653, -361.1960649407547521 ) ) ;
#39982 = CARTESIAN_POINT ( 'NONE',  ( 7.935645567813509160, -275.1330490791634134, -332.0972777557471431 ) ) ;
#39983 = CARTESIAN_POINT ( 'NONE',  ( -81.69594748424621855, -275.1994334023129909, -211.0458463439749721 ) ) ;
#39984 = CARTESIAN_POINT ( 'NONE',  ( -73.81004576435181264, -274.6595910587539606, -202.8368858384544637 ) ) ;
#39985 = CARTESIAN_POINT ( 'NONE',  ( -94.14817941614803942, -290.3951673907260442, -316.3068724411707535 ) ) ;
#39986 = CARTESIAN_POINT ( 'NONE',  ( -113.7815417226453434, -297.2570117141732453, -278.1783705180720858 ) ) ;
#39987 = CARTESIAN_POINT ( 'NONE',  ( -78.17511752514417367, -298.0109342361442941, -205.1525378198847989 ) ) ;
#39988 = CARTESIAN_POINT ( 'NONE',  ( 16.16058330017424538, -294.4326508754061820, -320.0250452585168546 ) ) ;
#39989 = ORIENTED_EDGE ( 'NONE', *, *, #84897, .F. ) ;
#39990 = AXIS2_PLACEMENT_3D ( 'NONE', #36985, #1458, #80522 ) ;
#39991 = CARTESIAN_POINT ( 'NONE',  ( -105.0440616761899406, -280.0315030321415861, -304.0302800101594585 ) ) ;
#39992 = CARTESIAN_POINT ( 'NONE',  ( -4.964175337356663498, -279.9747947529875773, -200.5669721539795489 ) ) ;
#39993 = CARTESIAN_POINT ( 'NONE',  ( -6.165610532423705159, -277.5733958302975566, -336.6430231450327710 ) ) ;
#39994 = CARTESIAN_POINT ( 'NONE',  ( 36.61092157524898028, -277.5342610683098314, -287.8810195974373300 ) ) ;
#39995 = CARTESIAN_POINT ( 'NONE',  ( -31.60127331474626899, -275.0002645543697781, -345.5488556988973414 ) ) ;
#39996 = CARTESIAN_POINT ( 'NONE',  ( -92.06841172516563176, -273.7354706260273929, -221.9568260288448869 ) ) ;
#39997 = CARTESIAN_POINT ( 'NONE',  ( -65.78382479129551541, -296.2473607405311782, -202.4905023772381867 ) ) ;
#39998 = FACE_OUTER_BOUND ( 'NONE', #69096, .T. ) ;
#39999 = CARTESIAN_POINT ( 'NONE',  ( -71.65230676159261236, -277.6854781189082360, -334.8095427585091670 ) ) ;
#40000 = AXIS2_PLACEMENT_3D ( 'NONE', #25076, #15642, #59204 ) ;
#40001 = CARTESIAN_POINT ( 'NONE',  ( 31.23789265634772150, -286.6769697346300063, -304.3942256849774139 ) ) ;
#40002 = CARTESIAN_POINT ( 'NONE',  ( -54.89100213468034895, -275.8266867059796823, -197.4432008104436136 ) ) ;
#40003 = CARTESIAN_POINT ( 'NONE',  ( -26.41588298435790350, -486.4924983417995463, -465.6442049081569508 ) ) ;
#40004 = CIRCLE ( 'NONE', #12827, 160.1282194813176716 ) ;
#40005 = CARTESIAN_POINT ( 'NONE',  ( -86.84614854937542816, -288.9589621501868919, -324.2992449736664753 ) ) ;
#40006 = CARTESIAN_POINT ( 'NONE',  ( -112.2585427403858915, -284.1179303563596932, -253.0181228491142349 ) ) ;
#40007 = CARTESIAN_POINT ( 'NONE',  ( 36.53264934074726966, -279.7330155334875030, -265.8274106709538955 ) ) ;
#40009 = CARTESIAN_POINT ( 'NONE',  ( -38.62569617740881966, -284.1158090869892590, -195.9194602071358133 ) ) ;
#40008 = CARTESIAN_POINT ( 'NONE',  ( 35.28215392580813869, -280.2823464980983772, -282.2418056774371280 ) ) ;
#40010 = CARTESIAN_POINT ( 'NONE',  ( 34.54820075568754589, -289.8281575918870203, -291.7793293692994325 ) ) ;
#40011 = CARTESIAN_POINT ( 'NONE',  ( -108.8697823169071626, -279.5405664881534449, -286.8747125391779491 ) ) ;
#40012 = CARTESIAN_POINT ( 'NONE',  ( 153.4730978675979998, 20.31600801108083587, 12.31661104704794951 ) ) ;
#40013 = CARTESIAN_POINT ( 'NONE',  ( -50.24789740371854663, -293.8875607099926697, -196.4799247197483965 ) ) ;
#40014 = CARTESIAN_POINT ( 'NONE',  ( -113.3635260201611885, -276.8126404626281101, -268.7332873345537791 ) ) ;
#40015 = CARTESIAN_POINT ( 'NONE',  ( 16.61198336187223035, -276.9103012581261964, -319.7041527892966997 ) ) ;
#40016 = CARTESIAN_POINT ( 'NONE',  ( -110.7294915276277010, -286.3440450689752765, -286.6172092936743070 ) ) ;
#40017 = FACE_OUTER_BOUND ( 'NONE', #40177, .T. ) ;
#40018 = CARTESIAN_POINT ( 'NONE',  ( -54.15690983343117892, -291.1864617378162166, -344.0800113258711690 ) ) ;
#40019 = CARTESIAN_POINT ( 'NONE',  ( -93.30674143646977825, -293.8563470380150306, -320.3657480697832511 ) ) ;
#40020 = EDGE_CURVE ( 'NONE', #6020, #6460, #54951, .T. ) ;
#40021 = CARTESIAN_POINT ( 'NONE',  ( -26.63347344892401480, -285.3821013558943491, -194.2190146525946091 ) ) ;
#40022 = CARTESIAN_POINT ( 'NONE',  ( -97.40066215283101769, -289.5457846169106801, -227.3869316750085545 ) ) ;
#40023 = CARTESIAN_POINT ( 'NONE',  ( 222.4306832106270804, -135.2391364535880882, 21.50000000000000000 ) ) ;
#40024 = CARTESIAN_POINT ( 'NONE',  ( -4.863123912941094140, -275.3001110874826054, -336.3022241359696523 ) ) ;
#40025 = CARTESIAN_POINT ( 'NONE',  ( -37.01348553373327377, -293.1875517288375477, -344.6082301598522690 ) ) ;
#40026 = FACE_OUTER_BOUND ( 'NONE', #17293, .T. ) ;
#40027 = CARTESIAN_POINT ( 'NONE',  ( -22.31123950296460379, -290.7210068484206431, -195.4955616898351707 ) ) ;
#40028 = CARTESIAN_POINT ( 'NONE',  ( -94.75714959288885098, -286.8010729087941399, -223.9739966762575136 ) ) ;
#40029 = CARTESIAN_POINT ( 'NONE',  ( 9.584321126841764737, -286.6569690972931426, -330.1936042499539781 ) ) ;
#40030 = CARTESIAN_POINT ( 'NONE',  ( -77.38479068328094002, -286.9291271721886005, -208.5598538230038628 ) ) ;
#40031 = EDGE_CURVE ( 'NONE', #4210, #16726, #23526, .T. ) ;
#40032 = DIRECTION ( 'NONE',  ( 0.000000000000000000, -1.000000000000000000, 0.000000000000000000 ) ) ;
#40033 = CARTESIAN_POINT ( 'NONE',  ( -38.63800055468101391, -286.8383551428286182, -197.1986168144262592 ) ) ;
#40034 = CARTESIAN_POINT ( 'NONE',  ( 37.86253805835301023, -295.6027371407022883, -275.8927440713060832 ) ) ;
#40035 = CARTESIAN_POINT ( 'NONE',  ( -94.14471879594898951, -275.9449207122509051, -320.1881314391042110 ) ) ;
#40036 = CARTESIAN_POINT ( 'NONE',  ( 34.16619138577753034, -276.2487381832852975, -299.0068814999503957 ) ) ;
#40037 = CARTESIAN_POINT ( 'NONE',  ( -71.49901856070748352, -289.6844723970174300, -202.9480414160184978 ) ) ;
#40038 = CARTESIAN_POINT ( 'NONE',  ( -108.5126566038881322, -278.9256751619376473, -240.9724304596572608 ) ) ;
#40039 = CARTESIAN_POINT ( 'NONE',  ( -91.25083380922150411, -299.2613291753639260, -218.6571652577696057 ) ) ;
#40040 = FACE_OUTER_BOUND ( 'NONE', #67862, .T. ) ;
#40041 = CARTESIAN_POINT ( 'NONE',  ( -48.18343439339133027, -253.0206516614774159, -474.6281350925841025 ) ) ;
#40042 = CARTESIAN_POINT ( 'NONE',  ( -100.2339573658729250, -276.1550768808709222, -309.8961176989543560 ) ) ;
#40043 = CARTESIAN_POINT ( 'NONE',  ( 36.29599654916341223, -279.3692829281176842, -256.1312100543079850 ) ) ;
#40044 = DIRECTION ( 'NONE',  ( 0.000000000000000000, 0.000000000000000000, -1.000000000000000000 ) ) ;
#40045 = CARTESIAN_POINT ( 'NONE',  ( 3.117325199323299323, -274.9995362870396320, -335.1208733944317828 ) ) ;
#40046 = CARTESIAN_POINT ( 'NONE',  ( -86.94248631422881601, -297.2778366144847837, -324.8631340983842506 ) ) ;
#40047 = CARTESIAN_POINT ( 'NONE',  ( 26.45707897364511041, -281.0349414596341830, -312.9194108852886984 ) ) ;
#40048 = CARTESIAN_POINT ( 'NONE',  ( -109.3713788792648813, -297.3184795589700116, -283.6643407293334462 ) ) ;
#40049 = CARTESIAN_POINT ( 'NONE',  ( -101.9092417073094197, -298.4086930955334651, -229.3205180033799309 ) ) ;
#40050 = CARTESIAN_POINT ( 'NONE',  ( -4.091270186654704766, -274.1698896770649867, -205.3355709942789247 ) ) ;
#40051 = CARTESIAN_POINT ( 'NONE',  ( 21.74316944361589066, -294.9182611452085325, -224.1453261717357179 ) ) ;
#40052 = CARTESIAN_POINT ( 'NONE',  ( 24.70201101716289571, -287.1130874018446661, -224.7587286608693091 ) ) ;
#40053 = CARTESIAN_POINT ( 'NONE',  ( 34.87795658004070276, -273.9843290321488212, -293.2658481795883176 ) ) ;
#40054 = CIRCLE ( 'NONE', #68819, 4.999999999999990230 ) ;
#40055 = CARTESIAN_POINT ( 'NONE',  ( -17.72637478188769578, -288.6392367472355431, -344.8207648797098841 ) ) ;
#40056 = CARTESIAN_POINT ( 'NONE',  ( 35.50967673622771770, -286.5124201141092612, -262.8721035741455125 ) ) ;
#40057 = CARTESIAN_POINT ( 'NONE',  ( -61.03204588874937286, -289.7446191059484022, -199.1462678954401895 ) ) ;
#40058 = ORIENTED_EDGE ( 'NONE', *, *, #83215, .F. ) ;
#40059 = CARTESIAN_POINT ( 'NONE',  ( -28.16072294498304274, -126.4832272301380556, -368.1402060870429409 ) ) ;
#40060 = CARTESIAN_POINT ( 'NONE',  ( -72.39388981885420549, -289.0370685149600263, -334.4651930453189266 ) ) ;
#40061 = CARTESIAN_POINT ( 'NONE',  ( -113.5873327694909420, -285.6052001264109208, -261.4491195654939588 ) ) ;
#40062 = CARTESIAN_POINT ( 'NONE',  ( 38.09624213391255410, -292.4326381615786090, -256.1506612417577458 ) ) ;
#40063 = CARTESIAN_POINT ( 'NONE',  ( 12.45383555886490434, -282.3326653276039906, -212.6823087093894173 ) ) ;
#40064 = CARTESIAN_POINT ( 'NONE',  ( 37.19323330833030639, -282.6494379105075723, -253.0455154827602087 ) ) ;
#40065 = CARTESIAN_POINT ( 'NONE',  ( -93.42343300352005997, -283.7223755569215200, -317.0926837836212826 ) ) ;
#40066 = CARTESIAN_POINT ( 'NONE',  ( 32.14024677237936345, -277.9220439890176522, -298.7352100012137726 ) ) ;
#40067 = CARTESIAN_POINT ( 'NONE',  ( -108.3750413894235436, -296.1725969528496876, -300.2188811053798077 ) ) ;
#40068 = CARTESIAN_POINT ( 'NONE',  ( -109.0195591655429297, -274.0800385051354624, -254.1275723580045280 ) ) ;
#40069 = CARTESIAN_POINT ( 'NONE',  ( -111.4249662102223510, -288.4543579125047472, -279.4998535989397510 ) ) ;
#40070 = AXIS2_PLACEMENT_3D ( 'NONE', #11248, #9840, #90294 ) ;
#40071 = CARTESIAN_POINT ( 'NONE',  ( -101.0548689193594072, -271.8448885987381800, -233.8204735609783995 ) ) ;
#40072 = ORIENTED_EDGE ( 'NONE', *, *, #10248, .F. ) ;
#40073 = CARTESIAN_POINT ( 'NONE',  ( 175.2296996224749250, 275.5000000000000568, -29.99999999999998224 ) ) ;
#40074 = CARTESIAN_POINT ( 'NONE',  ( -107.9050110815833392, -286.7830395481826713, -246.4902024312568756 ) ) ;
#40075 = CARTESIAN_POINT ( 'NONE',  ( 13.20247590706343388, -295.4448738187893468, -328.1097753205187928 ) ) ;
#40076 = CARTESIAN_POINT ( 'NONE',  ( -104.2031909254667852, -284.8063894256897015, -299.9150300112569312 ) ) ;
#40077 = CARTESIAN_POINT ( 'NONE',  ( 39.32012050874717346, -274.5495035605681551, -265.4667616949154194 ) ) ;
#40078 = CARTESIAN_POINT ( 'NONE',  ( -92.74441215752203505, -291.9352384738761543, -216.9575723052588216 ) ) ;
#40079 = CARTESIAN_POINT ( 'NONE',  ( -101.4603330445561369, -283.2289184265076187, -229.9989278496601059 ) ) ;
#40080 = CARTESIAN_POINT ( 'NONE',  ( -68.32414956125494143, -291.9894821483059104, -199.8780940707751768 ) ) ;
#40081 = CARTESIAN_POINT ( 'NONE',  ( -106.9709706704877163, -290.5919344085515377, -292.5249666946191383 ) ) ;
#40082 = CARTESIAN_POINT ( 'NONE',  ( 195.0629117428269126, 293.9636489450776367, -54.00000000000000000 ) ) ;
#40083 = CARTESIAN_POINT ( 'NONE',  ( 154.5815831708048336, 19.45636901171593180, -12.71858327454078363 ) ) ;
#40084 = CARTESIAN_POINT ( 'NONE',  ( -38.65064075601802074, -140.2996819125500565, -360.9686471963671011 ) ) ;
#40085 = CARTESIAN_POINT ( 'NONE',  ( -16.31414505355634859, -284.3054154541990783, -343.7681407864705534 ) ) ;
#40086 = CARTESIAN_POINT ( 'NONE',  ( -37.37352853689063181, -292.5523547857347353, -345.3611179825600175 ) ) ;
#40087 = ORIENTED_EDGE ( 'NONE', *, *, #18823, .T. ) ;
#40088 = ADVANCED_FACE ( 'NONE', ( #66165 ), #31105, .F. ) ;
#40089 = CARTESIAN_POINT ( 'NONE',  ( 5.762795176377190742, -281.3725869330493765, -329.6589135343029966 ) ) ;
#40090 = CARTESIAN_POINT ( 'NONE',  ( -48.49511986439432576, -276.8570119589404044, -346.5815622534594809 ) ) ;
#40091 = CARTESIAN_POINT ( 'NONE',  ( -103.7953643696253891, -281.0100932169717680, -235.8398544096079377 ) ) ;
#40092 = CARTESIAN_POINT ( 'NONE',  ( -61.32887853807750389, -183.8452602080190559, -360.6299234569646615 ) ) ;
#40093 = CARTESIAN_POINT ( 'NONE',  ( -13.62220642536452431, -281.3248584795038028, -342.9971414855608600 ) ) ;
#40094 = CARTESIAN_POINT ( 'NONE',  ( -108.9252590724021985, -282.8481418639596541, -249.0245356062137319 ) ) ;
#40095 = CARTESIAN_POINT ( 'NONE',  ( -15.20086602440459167, -300.0858634728058405, -194.3679151187695027 ) ) ;
#40096 = CARTESIAN_POINT ( 'NONE',  ( -94.81796891096114166, -296.4089913983243036, -315.4661838695809024 ) ) ;
#40097 = VERTEX_POINT ( 'NONE', #38173 ) ;
#40098 = CARTESIAN_POINT ( 'NONE',  ( 26.67228065799706371, -291.7448882022110865, -234.1537904275760127 ) ) ;
#40099 = CARTESIAN_POINT ( 'NONE',  ( 39.27963928983869835, -276.2851872958053150, -276.8790265555686005 ) ) ;
#40100 = CARTESIAN_POINT ( 'NONE',  ( 35.37821433383642500, -275.4605971271983549, -263.4207455564619522 ) ) ;
#40101 = CARTESIAN_POINT ( 'NONE',  ( 9.333141660948436780, -273.5971488577953323, -209.5092350794786569 ) ) ;
#40102 = CARTESIAN_POINT ( 'NONE',  ( 185.3457823239910738, 214.6360786829742437, 22.87680765314584264 ) ) ;
#40103 = CARTESIAN_POINT ( 'NONE',  ( -64.66280059341735864, -271.6953017060425282, -200.5007660474314832 ) ) ;
#40104 = CARTESIAN_POINT ( 'NONE',  ( 150.7108941768076420, 20.99999999999999645, 5.100416763304269629 ) ) ;
#40105 = EDGE_CURVE ( 'NONE', #87677, #83522, #1280, .T. ) ;
#40106 = CARTESIAN_POINT ( 'NONE',  ( -43.37497677679506580, -265.5639373360739341, -503.0380110733032666 ) ) ;
#40107 = CARTESIAN_POINT ( 'NONE',  ( 33.26084032723394301, -282.8915765668057247, -290.0970586854664930 ) ) ;
#40108 = CARTESIAN_POINT ( 'NONE',  ( 0.3849813559168659971, -284.3169310994955481, -336.3357722944173247 ) ) ;
#40109 = CARTESIAN_POINT ( 'NONE',  ( -106.2726213801001620, -283.5754797676106023, -294.8516004122698746 ) ) ;
#40110 = CARTESIAN_POINT ( 'NONE',  ( 5.848655634099327649, -274.8559055013023453, -330.2659502610648019 ) ) ;
#40111 = CARTESIAN_POINT ( 'NONE',  ( -18.39794291737094412, -284.6660543387716871, -342.1918443868438544 ) ) ;
#40112 = CARTESIAN_POINT ( 'NONE',  ( -109.7279446866395318, -276.8505860660528697, -284.2459637580699905 ) ) ;
#40113 = CARTESIAN_POINT ( 'NONE',  ( 35.01451377247138907, -276.7906239789874689, -282.4497198349457676 ) ) ;
#40114 = LINE ( 'NONE', #33032, #85084 ) ;
#40115 = CARTESIAN_POINT ( 'NONE',  ( -104.6570544767593276, -279.8358793108898794, -233.3097767252989740 ) ) ;
#40116 = ORIENTED_EDGE ( 'NONE', *, *, #46756, .T. ) ;
#40117 = ORIENTED_EDGE ( 'NONE', *, *, #60551, .F. ) ;
#40118 = CYLINDRICAL_SURFACE ( 'NONE', #32287, 6.154241149514405151 ) ;
#40119 = CARTESIAN_POINT ( 'NONE',  ( -69.29385972965550877, -287.4967074610819964, -201.6493469937357474 ) ) ;
#40120 = CARTESIAN_POINT ( 'NONE',  ( -9.178148466532000782, -293.8714332438996735, -337.8982013936831663 ) ) ;
#40121 = CARTESIAN_POINT ( 'NONE',  ( -109.3754374719327984, -290.2433117206783209, -243.2937418133845142 ) ) ;
#40122 = CARTESIAN_POINT ( 'NONE',  ( 35.51529902032152819, -285.9615671557526753, -283.3930668013445029 ) ) ;
#40124 = CARTESIAN_POINT ( 'NONE',  ( -110.6294709175320889, -288.6563108310282360, -280.7903528653516219 ) ) ;
#40123 = CARTESIAN_POINT ( 'NONE',  ( 32.84097504660392275, -285.8353667372550717, -248.1882171182276977 ) ) ;
#40125 = CARTESIAN_POINT ( 'NONE',  ( -61.65184179818690779, -284.5801319743679869, -339.6688627353864263 ) ) ;
#40126 = CARTESIAN_POINT ( 'NONE',  ( 36.94675294573447388, -273.4196546582299447, -260.0544993018278319 ) ) ;
#40127 = CARTESIAN_POINT ( 'NONE',  ( -0.08932612986281238121, -284.9390668879638611, -203.8729140247605756 ) ) ;
#40128 = CARTESIAN_POINT ( 'NONE',  ( -69.88487936619216612, -299.6237110299645110, -202.7893625008937022 ) ) ;
#40129 = CARTESIAN_POINT ( 'NONE',  ( 18.25075829543008155, -286.2565682532813298, -320.9718525808416416 ) ) ;
#40130 = CARTESIAN_POINT ( 'NONE',  ( 33.68083679361920701, -282.2577693448175751, -252.4438174280260228 ) ) ;
#40131 = CARTESIAN_POINT ( 'NONE',  ( -69.82321471852675643, -291.4789367081937144, -338.1615362372652385 ) ) ;
#40132 = CARTESIAN_POINT ( 'NONE',  ( -35.09237171215954021, -122.5496321078137356, 21.50000000000000000 ) ) ;
#40133 = CARTESIAN_POINT ( 'NONE',  ( 139.6925840978351516, 15.36528803885690664, -22.50000000000000000 ) ) ;
#40134 = CARTESIAN_POINT ( 'NONE',  ( -37.65794076881845598, -296.9761954410017211, -345.9332944128814233 ) ) ;
#40135 = AXIS2_PLACEMENT_3D ( 'NONE', #784, #21614, #51411 ) ;
#40136 = CARTESIAN_POINT ( 'NONE',  ( -32.81760037415347853, -278.1090144348538615, -195.4976878484475264 ) ) ;
#40137 = CARTESIAN_POINT ( 'NONE',  ( -69.54613633110318460, -290.8361624137102694, -200.5826824542176041 ) ) ;
#40138 = CARTESIAN_POINT ( 'NONE',  ( -96.25513867432701431, -294.3341962493550454, -314.8301954895704853 ) ) ;
#40139 = CARTESIAN_POINT ( 'NONE',  ( 5.868614539845057543, -281.1371222281718474, -329.8095173136823064 ) ) ;
#40140 = CARTESIAN_POINT ( 'NONE',  ( 3.744721200102505421, -272.6892301998387893, -208.2251898951031137 ) ) ;
#40141 = CARTESIAN_POINT ( 'NONE',  ( 36.11369905372555422, -294.8364704761917210, -268.0057395224523020 ) ) ;
#40142 = CARTESIAN_POINT ( 'NONE',  ( -110.4542110544635705, -286.8376638359844719, -287.0812184334320705 ) ) ;
#40143 = CARTESIAN_POINT ( 'NONE',  ( -111.3014765373895472, -294.7943154103827510, -289.1931454069718370 ) ) ;
#40144 = CARTESIAN_POINT ( 'NONE',  ( 38.59341007484657382, -291.8274801446793276, -273.1598766159764295 ) ) ;
#40145 = CARTESIAN_POINT ( 'NONE',  ( -65.56963253740221376, -293.1009461683775044, -202.3875140202095508 ) ) ;
#40146 = CARTESIAN_POINT ( 'NONE',  ( 152.4536156746142410, 275.0000000000000568, -14.50000000000000000 ) ) ;
#40147 = CARTESIAN_POINT ( 'NONE',  ( 21.11667801393515731, -293.7385796721616202, -226.3699853258602559 ) ) ;
#40148 = DIRECTION ( 'NONE',  ( -0.000000000000000000, -1.000000000000000000, -0.000000000000000000 ) ) ;
#40150 = CARTESIAN_POINT ( 'NONE',  ( -66.05313749947666224, -295.4386775450634559, -337.4778324735751767 ) ) ;
#40149 = CARTESIAN_POINT ( 'NONE',  ( -93.19729783831272130, -281.8700073868677691, -320.9624640002090246 ) ) ;
#40151 = CARTESIAN_POINT ( 'NONE',  ( 38.66784513340837748, -281.7071423286387812, -282.7540055199416429 ) ) ;
#40152 = CARTESIAN_POINT ( 'NONE',  ( -66.57215317191126758, -283.0913821453785317, -341.5885358424188780 ) ) ;
#40153 = CARTESIAN_POINT ( 'NONE',  ( -42.82300483389046519, -287.1211847448572030, -345.0453166641094072 ) ) ;
#40154 = DIRECTION ( 'NONE',  ( 0.000000000000000000, 1.000000000000000000, 0.000000000000000000 ) ) ;
#40155 = CARTESIAN_POINT ( 'NONE',  ( 31.75626198119757504, -280.4517813083118085, -302.8611370630159740 ) ) ;
#40156 = CARTESIAN_POINT ( 'NONE',  ( 36.48310307912309014, -286.7343657243646931, -291.1791992913473450 ) ) ;
#40157 = CARTESIAN_POINT ( 'NONE',  ( 207.1738322328983770, 30.51833626076158978, 15.03205023725369038 ) ) ;
#40158 = CARTESIAN_POINT ( 'NONE',  ( -47.88742736761130914, -296.7884936568450485, -343.4556035799229221 ) ) ;
#40159 = CARTESIAN_POINT ( 'NONE',  ( -73.79961244147870048, -278.9517256555167251, -337.5282702082107562 ) ) ;
#40160 = CARTESIAN_POINT ( 'NONE',  ( -62.31219064049827949, -279.3850568356900794, -201.6887835738847343 ) ) ;
#40161 = CARTESIAN_POINT ( 'NONE',  ( -37.79715997090553969, -292.2132741407780827, -193.3624650016934368 ) ) ;
#40162 = CARTESIAN_POINT ( 'NONE',  ( -6.074148943219241481, -280.7242895402707177, -339.1481403360583045 ) ) ;
#40163 = CARTESIAN_POINT ( 'NONE',  ( -12.16810478285903940, -291.4465099774787404, -201.5342592106387087 ) ) ;
#40164 = B_SPLINE_CURVE_WITH_KNOTS ( 'NONE', 3,
 ( #60924, #82216, #9298, #67561 ),
 .UNSPECIFIED., .F., .F.,
 ( 4, 4 ),
 ( 0.000000000000000000, 9.632970524405273739E-05 ),
 .UNSPECIFIED. ) ;
#40165 = CARTESIAN_POINT ( 'NONE',  ( -88.23203679673940769, -295.3398691553587696, -215.1983737472510256 ) ) ;
#40166 = VERTEX_POINT ( 'NONE', #51924 ) ;
#40167 = CARTESIAN_POINT ( 'NONE',  ( -37.00155433637099378, -294.5553988545158290, -343.4342994320877551 ) ) ;
#40168 = DIRECTION ( 'NONE',  ( 1.124465274301078034E-16, 1.000000000000000000, 0.000000000000000000 ) ) ;
#40169 = CARTESIAN_POINT ( 'NONE',  ( -102.0172624299487154, -288.4809262143061801, -239.1787733560258289 ) ) ;
#40170 = CARTESIAN_POINT ( 'NONE',  ( -35.82186107926352037, -297.1294972969841410, -193.5966463115552187 ) ) ;
#40171 = CARTESIAN_POINT ( 'NONE',  ( 26.81817931088598073, -279.1544078907135713, -229.9661576509479062 ) ) ;
#40172 = CARTESIAN_POINT ( 'NONE',  ( -3.721273210295284350, -287.8016481334057630, -201.6228523707503371 ) ) ;
#40173 = CARTESIAN_POINT ( 'NONE',  ( 21.17221221186893487, -287.9981436606121861, -314.0297462076907777 ) ) ;
#40174 = CARTESIAN_POINT ( 'NONE',  ( -91.46401832657168995, -279.3599840078262559, -320.4501432748168099 ) ) ;
#40175 = CARTESIAN_POINT ( 'NONE',  ( -60.85882815576348293, -299.5030410351093906, -200.1291356229187386 ) ) ;
#40176 = CARTESIAN_POINT ( 'NONE',  ( -99.51959407465871266, -276.8103114638750526, -309.4565968598176937 ) ) ;
#40177 = EDGE_LOOP ( 'NONE', ( #25118, #75403 ) ) ;
#40178 = CARTESIAN_POINT ( 'NONE',  ( 7.977900039700807966, -298.2717498065657082, -193.3847308610179709 ) ) ;
#40179 = CARTESIAN_POINT ( 'NONE',  ( -105.3536124538997711, -292.0713083396632328, -300.7487589939452164 ) ) ;
#40180 = CARTESIAN_POINT ( 'NONE',  ( 31.51594013473109257, -295.5762779928133455, -303.1195342151915497 ) ) ;
#40181 = CARTESIAN_POINT ( 'NONE',  ( -112.3417001281054297, -274.5519904173220311, -270.3865538441530134 ) ) ;
#40182 = CARTESIAN_POINT ( 'NONE',  ( -84.74483085874628330, -290.3770266918165248, -326.0771471112191762 ) ) ;
#40183 = CARTESIAN_POINT ( 'NONE',  ( -48.18343439338617884, -250.5775211731748016, -453.4113254038507534 ) ) ;
#40184 = EDGE_LOOP ( 'NONE', ( #87033, #73988, #57834, #60165, #59226 ) ) ;
#40185 = CARTESIAN_POINT ( 'NONE',  ( -108.2777975997807687, -296.8239053091572259, -300.1869908493025036 ) ) ;
#40186 = CARTESIAN_POINT ( 'NONE',  ( -102.7443338610062398, -288.1846738122455918, -308.7115243331081160 ) ) ;
#40187 = CARTESIAN_POINT ( 'NONE',  ( -20.51992406059540386, -298.5906499936787668, -193.3813386032300627 ) ) ;
#40188 = DIRECTION ( 'NONE',  ( 0.000000000000000000, 0.000000000000000000, -1.000000000000000000 ) ) ;
#40189 = CARTESIAN_POINT ( 'NONE',  ( 196.3765075725969211, 25.23352658328733256, 13.80344107416052957 ) ) ;
#40190 = CARTESIAN_POINT ( 'NONE',  ( -92.32605091355844706, -292.8038071451268820, -217.3762944957956904 ) ) ;
#40191 = CARTESIAN_POINT ( 'NONE',  ( -115.3288506153726871, -292.8376638359844719, -288.1938231032136741 ) ) ;
#40192 = ADVANCED_FACE ( 'NONE', ( #23046 ), #58594, .T. ) ;
#40193 = CARTESIAN_POINT ( 'NONE',  ( -112.1426021787407734, -286.5806676322059730, -268.1580574037957945 ) ) ;
#40194 = EDGE_CURVE ( 'NONE', #64758, #52349, #22824, .T. ) ;
#40195 = CARTESIAN_POINT ( 'NONE',  ( -35.31579140500846847, -272.0774514714984775, -195.5423891952795259 ) ) ;
#40196 = CARTESIAN_POINT ( 'NONE',  ( -94.02589681328788629, -275.1454823192548815, -222.0898422885150012 ) ) ;
#40197 = CARTESIAN_POINT ( 'NONE',  ( -88.91088281404442739, -289.4011311945246234, -216.6062619644874587 ) ) ;
#40198 = CARTESIAN_POINT ( 'NONE',  ( -111.5132822861773860, -280.6098023860867556, -254.8426522913349572 ) ) ;
#40199 = AXIS2_PLACEMENT_3D ( 'NONE', #37305, #29292, #80864 ) ;
#40201 = CARTESIAN_POINT ( 'NONE',  ( 13.41183382841328786, -280.1336181705341914, -217.6790537174373128 ) ) ;
#40200 = CARTESIAN_POINT ( 'NONE',  ( -32.96301398965226781, -280.1088519242433676, -197.4925574938202431 ) ) ;
#40202 = CARTESIAN_POINT ( 'NONE',  ( -1.599553540020983267, -277.6692916526148451, -338.2138369244971159 ) ) ;
#40203 = CARTESIAN_POINT ( 'NONE',  ( -36.74017999978996585, -278.8544850417941348, -193.7475722532458633 ) ) ;
#40204 = CARTESIAN_POINT ( 'NONE',  ( 24.07068301800163468, -23.09745244138832021, -342.0737546775265514 ) ) ;
#40205 = CARTESIAN_POINT ( 'NONE',  ( 11.62635313455881558, -275.6535988416750342, -211.1739514600166103 ) ) ;
#40206 = DIRECTION ( 'NONE',  ( 0.000000000000000000, 0.000000000000000000, 1.000000000000000000 ) ) ;
#40207 = CARTESIAN_POINT ( 'NONE',  ( -93.64686790491953161, -274.7792567582446281, -218.8400156709825524 ) ) ;
#40208 = CARTESIAN_POINT ( 'NONE',  ( -106.6379572354042296, -298.6233781216988632, -303.7686719486574702 ) ) ;
#40209 = ORIENTED_EDGE ( 'NONE', *, *, #49529, .F. ) ;
#40210 = DIRECTION ( 'NONE',  ( -0.6249999999999938938, -1.354168079406255383E-15, 0.7806247497998046736 ) ) ;
#40211 = CARTESIAN_POINT ( 'NONE',  ( 32.12915457211946091, -288.3221465360573461, -246.9511538494989793 ) ) ;
#40212 = CARTESIAN_POINT ( 'NONE',  ( 17.92341329464438715, -290.0339282662094433, -322.5122565315427892 ) ) ;
#40213 = CARTESIAN_POINT ( 'NONE',  ( -72.41504633432106175, -288.8780281951142115, -334.4996637586543784 ) ) ;
#40214 = CARTESIAN_POINT ( 'NONE',  ( 5.150917078162668084, -286.1174522227927355, -206.1579332821879404 ) ) ;
#40215 = CARTESIAN_POINT ( 'NONE',  ( 184.1778392089217107, 3.000000000000000888, 9.000000000000001776 ) ) ;
#40216 = CARTESIAN_POINT ( 'NONE',  ( 16.39453744152071479, -280.6730977097220716, -321.0199702973334297 ) ) ;
#40217 = CARTESIAN_POINT ( 'NONE',  ( -20.83197491482815167, -290.6984114718369483, -342.7371806746199354 ) ) ;
#40218 = CARTESIAN_POINT ( 'NONE',  ( -93.09625896302375736, -282.3517350958592260, -318.5688835727382866 ) ) ;
#40219 = CARTESIAN_POINT ( 'NONE',  ( -41.09299418832080875, -281.3191294910885176, -196.9637660435205930 ) ) ;
#40220 = CARTESIAN_POINT ( 'NONE',  ( -5.033232194831216866, -277.1073396884305566, -335.9047950491271308 ) ) ;
#40221 = CARTESIAN_POINT ( 'NONE',  ( -99.55679244840483477, -288.7514205678791654, -315.0746592334719480 ) ) ;
#40222 = CARTESIAN_POINT ( 'NONE',  ( -113.3293070806293059, -285.5023006148979903, -258.6063387006830112 ) ) ;
#40223 = CARTESIAN_POINT ( 'NONE',  ( -63.18666872767307296, -286.2166709612661180, -197.8934389715013822 ) ) ;
#40224 = CARTESIAN_POINT ( 'NONE',  ( 35.03250150065544233, -281.5880532896999284, -260.4472952927281426 ) ) ;
#40225 = ORIENTED_EDGE ( 'NONE', *, *, #17187, .T. ) ;
#40226 = CARTESIAN_POINT ( 'NONE',  ( 200.9103445561495960, 65.54396272403066348, 5.212391550061751921 ) ) ;
#40227 = CARTESIAN_POINT ( 'NONE',  ( -91.93870168046433378, -293.1440462414617514, -217.7557679270126982 ) ) ;
#40228 =( BOUNDED_CURVE ( )  B_SPLINE_CURVE ( 3, ( #93044, #28201, #16303, #15848 ),
 .UNSPECIFIED., .F., .F. ) 
 B_SPLINE_CURVE_WITH_KNOTS ( ( 4, 4 ),
 ( 4.278565243615663150, 4.712388980384691450 ),
 .UNSPECIFIED. ) 
 CURVE ( )  GEOMETRIC_REPRESENTATION_ITEM ( )  RATIONAL_B_SPLINE_CURVE ( ( 1.000000000000000000, 0.9843778111405747655, 0.9843778111405747655, 1.000000000000000000 ) ) 
 REPRESENTATION_ITEM ( '' )  );
#40229 = CARTESIAN_POINT ( 'NONE',  ( -37.77532100652363312, -290.7316599778227442, -193.8554956534819951 ) ) ;
#40230 = CARTESIAN_POINT ( 'NONE',  ( 25.48382586996844523, -274.0937351059172329, -232.6282847950508597 ) ) ;
#40231 = CARTESIAN_POINT ( 'NONE',  ( -74.56430276819779124, -294.8821865711833539, -337.7096142731411419 ) ) ;
#40232 = CARTESIAN_POINT ( 'NONE',  ( -86.37606391125603977, -289.8369702536953696, -215.2802791846533523 ) ) ;
#40233 = CARTESIAN_POINT ( 'NONE',  ( -34.28142380136883816, -293.2530057701960686, -344.3111600648140325 ) ) ;
#40234 = CARTESIAN_POINT ( 'NONE',  ( -70.13614598002813239, -290.6992528245734775, -336.0382429879452957 ) ) ;
#40235 = DIRECTION ( 'NONE',  ( 0.000000000000000000, 0.000000000000000000, 1.000000000000000000 ) ) ;
#40236 = CARTESIAN_POINT ( 'NONE',  ( -64.69327756281664676, -291.4093006799419641, -340.2507352403997629 ) ) ;
#40237 = CARTESIAN_POINT ( 'NONE',  ( 24.98730492991275653, -290.9838813684707475, -228.2561406114209888 ) ) ;
#40238 = CARTESIAN_POINT ( 'NONE',  ( -7.211395784144283283, -296.6572533313993176, -339.0974399810747855 ) ) ;
#40239 = CARTESIAN_POINT ( 'NONE',  ( -2.083597929016404837, -287.4720173169050099, -206.1148572225795874 ) ) ;
#40240 = CARTESIAN_POINT ( 'NONE',  ( -4.564827007459695274, -276.4616969223038723, -202.4935258645224394 ) ) ;
#40241 = CARTESIAN_POINT ( 'NONE',  ( -70.14498173764704347, -276.2696582441936357, -339.5994189165526222 ) ) ;
#40242 = CARTESIAN_POINT ( 'NONE',  ( -78.10811599370715896, -296.7159632423421840, -205.2284982153708199 ) ) ;
#40243 = CARTESIAN_POINT ( 'NONE',  ( 33.86674326999936113, -274.0557201147880733, -290.5899046316356475 ) ) ;
#40244 = CARTESIAN_POINT ( 'NONE',  ( -96.74641479322900750, -277.2502375335812417, -225.4802528007515434 ) ) ;
#40245 = CARTESIAN_POINT ( 'NONE',  ( -43.53082439929039538, -275.1774514536521679, -197.1744677493692848 ) ) ;
#40246 = CARTESIAN_POINT ( 'NONE',  ( -4.359748912820315958, -275.0245934224437860, -339.0677583208797614 ) ) ;
#40247 = CARTESIAN_POINT ( 'NONE',  ( 197.9445473535685380, 71.72765703694831529, 10.67027600767679019 ) ) ;
#40248 = CARTESIAN_POINT ( 'NONE',  ( -100.8103800471136680, -273.7010786471676624, -233.9878389500318008 ) ) ;
#40249 = CARTESIAN_POINT ( 'NONE',  ( 189.9243309297870610, 275.5000000000000568, 20.22542485937349355 ) ) ;
#40251 = CARTESIAN_POINT ( 'NONE',  ( 7.332587685620199913, -274.5142294574891366, -212.6271763812662527 ) ) ;
#40250 = CARTESIAN_POINT ( 'NONE',  ( -73.65725780624509866, -287.5517500862881093, -336.4030215070834515 ) ) ;
#40252 = CARTESIAN_POINT ( 'NONE',  ( -28.97717893952974322, -288.9490459424088726, -346.9589760704899390 ) ) ;
#40253 = CARTESIAN_POINT ( 'NONE',  ( -62.76067725732410452, -289.0407487716310015, -343.0784809513011169 ) ) ;
#40254 = CARTESIAN_POINT ( 'NONE',  ( -96.38909544602353208, -275.1895370155652927, -223.8483935142291443 ) ) ;
#40255 = CARTESIAN_POINT ( 'NONE',  ( -42.54192650756851890, -293.1177497468139563, -345.0135531265428881 ) ) ;
#40256 = CARTESIAN_POINT ( 'NONE',  ( 39.36726158846801837, -280.8157299222871188, -275.6599710469711226 ) ) ;
#40257 = CARTESIAN_POINT ( 'NONE',  ( 154.7659666677267580, 19.56018909072085066, 12.94946946941272437 ) ) ;
#40258 = CARTESIAN_POINT ( 'NONE',  ( -111.7861933247250050, -276.4297109563016761, -279.8844756648734347 ) ) ;
#40259 = DIRECTION ( 'NONE',  ( 0.000000000000000000, 1.000000000000000000, 0.000000000000000000 ) ) ;
#40260 = CARTESIAN_POINT ( 'NONE',  ( -98.44972449581582907, -288.7855000624626882, -311.0403685920500152 ) ) ;
#40261 = CARTESIAN_POINT ( 'NONE',  ( 186.6539576904058890, 293.9636489450775230, 0.000000000000000000 ) ) ;
#40262 = CARTESIAN_POINT ( 'NONE',  ( -105.3597193119151711, -288.9671867823670368, -238.7612807683443634 ) ) ;
#40263 = CARTESIAN_POINT ( 'NONE',  ( -2.603770651260073343, -276.0405163377008648, -205.3689337651601932 ) ) ;
#40264 = CARTESIAN_POINT ( 'NONE',  ( 37.40445599313808600, -282.7767182098007197, -254.4361061248319231 ) ) ;
#40266 = CARTESIAN_POINT ( 'NONE',  ( -58.94813133534841398, -283.3394758848206720, -340.1434654586647639 ) ) ;
#40265 = CARTESIAN_POINT ( 'NONE',  ( -37.57667570481402919, -296.0693364529760743, -195.0062800877014979 ) ) ;
#40267 = CARTESIAN_POINT ( 'NONE',  ( -36.74941432824717680, -275.4850115414347442, -196.7617556734629716 ) ) ;
#40268 = CARTESIAN_POINT ( 'NONE',  ( -8.917513416117403224, -275.2364175145195304, -202.8929433299195466 ) ) ;
#40269 = CARTESIAN_POINT ( 'NONE',  ( 36.69238179845905989, -285.8245570761948784, -285.4696888794601364 ) ) ;
#40270 = CARTESIAN_POINT ( 'NONE',  ( 25.07202786556470286, -284.1142764794475966, -311.9487027491192066 ) ) ;
#40271 = CARTESIAN_POINT ( 'NONE',  ( 9.128316012624253517, -297.7066625357991825, -197.1334806806277129 ) ) ;
#40272 = ORIENTED_EDGE ( 'NONE', *, *, #4411, .F. ) ;
#40273 = CARTESIAN_POINT ( 'NONE',  ( 208.6208076322478746, 32.98517505407394168, 10.00000000000000000 ) ) ;
#40274 = CARTESIAN_POINT ( 'NONE',  ( -16.50891973755927822, -294.6236239495773361, -344.5445855467741580 ) ) ;
#40275 = CARTESIAN_POINT ( 'NONE',  ( -103.2110607073295370, -286.0627493961774803, -305.5862152029044978 ) ) ;
#40276 = CARTESIAN_POINT ( 'NONE',  ( 143.6449502718966755, 5.787831549089307747E-16, 22.08578643762690064 ) ) ;
#40277 = CARTESIAN_POINT ( 'NONE',  ( -72.02372285203398405, -271.1237833571632905, -198.2697987213421698 ) ) ;
#40278 = CARTESIAN_POINT ( 'NONE',  ( -74.02876733551443067, -276.7239807225424215, -337.8906650403386038 ) ) ;
#40279 = CARTESIAN_POINT ( 'NONE',  ( -112.8703660387259760, -289.0844462595420623, -259.8829617893832733 ) ) ;
#40280 = CARTESIAN_POINT ( 'NONE',  ( -3.283904601745656571, -284.1140271832124427, -335.7264192126351645 ) ) ;
#40281 = CARTESIAN_POINT ( 'NONE',  ( -32.32985693659846049, -278.7483780957962267, -344.2552296789129969 ) ) ;
#40282 = CARTESIAN_POINT ( 'NONE',  ( -109.4274434302726320, -286.2995768828680525, -245.0184286087743715 ) ) ;
#40283 = CARTESIAN_POINT ( 'NONE',  ( 1.412156205598005698, -282.5696769494897467, -206.0893352650113570 ) ) ;
#40284 = CARTESIAN_POINT ( 'NONE',  ( 7.233260528640313325, -274.8074478649547245, -207.5097556160975500 ) ) ;
#40285 = CARTESIAN_POINT ( 'NONE',  ( -67.71056107890268549, -277.2731252454187825, -341.1193845601805492 ) ) ;
#40286 = CARTESIAN_POINT ( 'NONE',  ( -70.34085681697077064, -297.4107243580212412, -337.0871987860103332 ) ) ;
#40287 = FACE_OUTER_BOUND ( 'NONE', #41324, .T. ) ;
#40288 = EDGE_CURVE ( 'NONE', #85305, #55107, #44337, .T. ) ;
#40289 = CARTESIAN_POINT ( 'NONE',  ( 185.4863495377425977, 214.7658868572315498, 22.87680765314782860 ) ) ;
#40290 = CARTESIAN_POINT ( 'NONE',  ( -113.1681449034579288, -270.8640168928444609, -264.6793891393130025 ) ) ;
#40291 = CARTESIAN_POINT ( 'NONE',  ( 35.66308864001567969, -275.1120112299278162, -274.3222119941613073 ) ) ;
#40292 = CARTESIAN_POINT ( 'NONE',  ( -43.27959702465449254, -299.0586335826179720, -193.8474522296141913 ) ) ;
#40293 = CARTESIAN_POINT ( 'NONE',  ( -49.61128450112837385, -287.6538493211135119, -197.3196473749968902 ) ) ;
#40294 = CARTESIAN_POINT ( 'NONE',  ( -110.1325382354403928, -297.7814505541182939, -293.3002672883740161 ) ) ;
#40295 = CARTESIAN_POINT ( 'NONE',  ( -113.9410608491082826, -297.7665210643149294, -269.6217570473887122 ) ) ;
#40296 = ADVANCED_FACE ( 'NONE', ( #46214 ), #88831, .T. ) ;
#40297 = CARTESIAN_POINT ( 'NONE',  ( -80.61100830522308058, -293.4645102622918102, -209.2419138053886627 ) ) ;
#40298 = CARTESIAN_POINT ( 'NONE',  ( -16.38448002622649824, -278.3234877718984421, -198.5222472401431162 ) ) ;
#40299 = CARTESIAN_POINT ( 'NONE',  ( -72.83746676551753296, -281.4982014040226659, -204.9289794691087536 ) ) ;
#40300 = CARTESIAN_POINT ( 'NONE',  ( -63.56427577703370702, -295.7876930335344809, -200.6381576156095150 ) ) ;
#40301 = CARTESIAN_POINT ( 'NONE',  ( -60.82593478213906479, -285.2139741538793487, -342.4492017140225357 ) ) ;
#40302 = CARTESIAN_POINT ( 'NONE',  ( 16.20962641980324292, -285.7551229352160931, -220.2778162924574872 ) ) ;
#40303 = CARTESIAN_POINT ( 'NONE',  ( -69.43587163635656623, -197.0798774606213044, -360.0883899004672344 ) ) ;
#40304 = ORIENTED_EDGE ( 'NONE', *, *, #42665, .T. ) ;
#40305 = CARTESIAN_POINT ( 'NONE',  ( 32.29503628924079806, -286.9271816716953936, -248.3462560050296020 ) ) ;
#40306 = ORIENTED_EDGE ( 'NONE', *, *, #28382, .F. ) ;
#40307 = CARTESIAN_POINT ( 'NONE',  ( 36.68302432211552855, -282.3792019230424444, -250.2655865881534965 ) ) ;
#40308 = CARTESIAN_POINT ( 'NONE',  ( -91.14098625775427820, -273.5939946197576091, -220.9692914688024814 ) ) ;
#40309 = CARTESIAN_POINT ( 'NONE',  ( 13.99223219465214463, -285.5482619160324020, -213.4319043924199946 ) ) ;
#40310 = CARTESIAN_POINT ( 'NONE',  ( -22.62307397294971878, -281.1772391186856339, -194.9665872965468338 ) ) ;
#40311 = CARTESIAN_POINT ( 'NONE',  ( 193.9646936176702070, 19.99999999999999645, -14.99999999999999467 ) ) ;
#40312 = CARTESIAN_POINT ( 'NONE',  ( -109.8965370368623411, -280.3741776000559867, -246.5606030017572152 ) ) ;
#40313 = CARTESIAN_POINT ( 'NONE',  ( -1.149130967571978967, -280.8523583744608914, -202.4211280712816858 ) ) ;
#40314 = CARTESIAN_POINT ( 'NONE',  ( -21.33282851196157992, -283.7666405000204009, -200.3683826091710216 ) ) ;
#40315 = CARTESIAN_POINT ( 'NONE',  ( -30.68111782768947648, -124.5880914476725820, -364.4545987036558472 ) ) ;
#40316 = ORIENTED_EDGE ( 'NONE', *, *, #22793, .T. ) ;
#40317 = CARTESIAN_POINT ( 'NONE',  ( -46.42597181955041918, -275.9367614358185961, -196.0812119987735400 ) ) ;
#40318 = CARTESIAN_POINT ( 'NONE',  ( -40.31272606951220894, -139.2760872083653112, -364.4166386884767235 ) ) ;
#40319 = CARTESIAN_POINT ( 'NONE',  ( 20.61347554750452815, -280.2234616458142682, -317.4242637509498763 ) ) ;
#40320 = CARTESIAN_POINT ( 'NONE',  ( -30.80705249287348124, -293.8936763090558770, -194.6038864475353876 ) ) ;
#40321 = CARTESIAN_POINT ( 'NONE',  ( -28.89242184229226496, -294.2909349696849404, -343.0242011832186790 ) ) ;
#40322 = CARTESIAN_POINT ( 'NONE',  ( -42.04393268639119441, -291.5020270628396588, -193.5664833245303100 ) ) ;
#40323 = LINE ( 'NONE', #25214, #58155 ) ;
#40325 = CARTESIAN_POINT ( 'NONE',  ( 31.73047897364953585, -285.6072588459414305, -244.2268595623524163 ) ) ;
#40324 = CARTESIAN_POINT ( 'NONE',  ( -93.27065634060967625, -294.4115757982546597, -322.4434147832793087 ) ) ;
#40326 = CARTESIAN_POINT ( 'NONE',  ( 34.49766186445496174, -295.1696950398659283, -251.6535913892309395 ) ) ;
#40327 = CARTESIAN_POINT ( 'NONE',  ( -96.17069049695247429, -286.4814759086748950, -226.3112215992280767 ) ) ;
#40328 = ORIENTED_EDGE ( 'NONE', *, *, #7928, .T. ) ;
#40329 = CARTESIAN_POINT ( 'NONE',  ( 37.52914483312031990, -294.2801461510863987, -253.3559323539323884 ) ) ;
#40330 = CARTESIAN_POINT ( 'NONE',  ( 30.39392505035694825, -282.4108956579887035, -297.7449366204801890 ) ) ;
#40331 = CARTESIAN_POINT ( 'NONE',  ( -41.93716073505599695, -293.9036425995275863, -346.8782031763719260 ) ) ;
#40332 = CARTESIAN_POINT ( 'NONE',  ( -85.05638526987864623, -290.4942147617866226, -330.6574590484464125 ) ) ;
#40333 = CARTESIAN_POINT ( 'NONE',  ( -8.540078410623545224, -292.9115321787788275, -199.0169276814324633 ) ) ;
#40334 = CARTESIAN_POINT ( 'NONE',  ( -18.47145725416471507, -288.9690159218346253, -340.9325948489732241 ) ) ;
#40335 = ORIENTED_EDGE ( 'NONE', *, *, #25145, .T. ) ;
#40336 = DIRECTION ( 'NONE',  ( 1.000000000000000000, 0.000000000000000000, 0.000000000000000000 ) ) ;
#40337 = CARTESIAN_POINT ( 'NONE',  ( -111.0978075727358743, -298.1915749314243271, -287.7475409260036372 ) ) ;
#40338 = CARTESIAN_POINT ( 'NONE',  ( 75.49899281977172905, -298.1218452906548464, -193.8788234879655477 ) ) ;
#40339 = CARTESIAN_POINT ( 'NONE',  ( -22.13388136519051130, -279.3103712974322548, -198.6702010224383059 ) ) ;
#40340 = CARTESIAN_POINT ( 'NONE',  ( 34.12476320728853096, -275.4232427413429036, -299.0015947809164345 ) ) ;
#40341 = CARTESIAN_POINT ( 'NONE',  ( -68.32150903723427859, -296.1175592700974448, -203.4820934126534837 ) ) ;
#40342 = CARTESIAN_POINT ( 'NONE',  ( -68.53524459840360805, -279.3268666977951398, -337.7385001781133269 ) ) ;
#40343 = CARTESIAN_POINT ( 'NONE',  ( 35.36970726023576361, -273.8858488169000793, -285.3249650392575063 ) ) ;
#40344 = CARTESIAN_POINT ( 'NONE',  ( -99.05891737047200252, -297.2093039881702907, -310.1796985396794071 ) ) ;
#40345 = CARTESIAN_POINT ( 'NONE',  ( -108.1377471099350771, -297.8826929133082899, -251.2825818296008435 ) ) ;
#40346 = CARTESIAN_POINT ( 'NONE',  ( 197.4878715644970555, 25.93102243561465414, 12.00000000000000000 ) ) ;
#40347 = CARTESIAN_POINT ( 'NONE',  ( -77.79519343797886677, -299.1185368534624445, -205.7859269755718969 ) ) ;
#40348 = CARTESIAN_POINT ( 'NONE',  ( -104.1390115208792650, -271.0333383620821905, -235.3696795757728353 ) ) ;
#40349 = CARTESIAN_POINT ( 'NONE',  ( -69.06933624462200783, -292.2749678855324191, -204.4894953015212593 ) ) ;
#40350 = CARTESIAN_POINT ( 'NONE',  ( -106.2561030079704665, -289.4701729014945499, -244.4061591369993209 ) ) ;
#40351 = CARTESIAN_POINT ( 'NONE',  ( 209.3190042249899250, 30.23012903947021002, 15.12480380540110225 ) ) ;
#40352 = CARTESIAN_POINT ( 'NONE',  ( -15.80060419697402629, -274.8157711547287363, -196.4444133984104326 ) ) ;
#40353 = CARTESIAN_POINT ( 'NONE',  ( -44.57540178027967670, -298.2915238935011644, -197.6487571438956365 ) ) ;
#40354 = CARTESIAN_POINT ( 'NONE',  ( -71.77813887535351967, -281.5792859684895006, -203.3203762048489125 ) ) ;
#40355 = CARTESIAN_POINT ( 'NONE',  ( 15.40136942118950714, -281.0100184163943595, -325.7819343458215826 ) ) ;
#40356 = CARTESIAN_POINT ( 'NONE',  ( -37.13557863764886946, -276.3981907261499487, -347.2719504756964284 ) ) ;
#40357 = CARTESIAN_POINT ( 'NONE',  ( -69.08846317310552365, -282.6778941922639206, -336.2896305014791096 ) ) ;
#40358 = CARTESIAN_POINT ( 'NONE',  ( -4.976858644766549489, -280.6269117199074685, -338.2173220153252373 ) ) ;
#40359 = CARTESIAN_POINT ( 'NONE',  ( 31.67719204698937219, -273.7891802211075856, -244.8313816107037439 ) ) ;
#40360 = CARTESIAN_POINT ( 'NONE',  ( -77.09343530281887524, -279.5845995019289489, -334.0202496965131331 ) ) ;
#40361 = CARTESIAN_POINT ( 'NONE',  ( 208.6208076322478746, 32.98517505407394168, 10.50000000000000000 ) ) ;
#40362 = DIRECTION ( 'NONE',  ( 1.000000000000000000, 0.000000000000000000, 0.000000000000000000 ) ) ;
#40363 = CARTESIAN_POINT ( 'NONE',  ( -113.3811844794317523, -271.0240039671355134, -264.6655298172289577 ) ) ;
#40364 = CARTESIAN_POINT ( 'NONE',  ( -111.4864747299796903, -280.3940606598785621, -282.7134791763288604 ) ) ;
#40365 = DIRECTION ( 'NONE',  ( 0.000000000000000000, 0.000000000000000000, -1.000000000000000000 ) ) ;
#40366 = CARTESIAN_POINT ( 'NONE',  ( -87.34984184609383817, -285.6628006742843695, -327.0745821107507254 ) ) ;
#40367 = EDGE_LOOP ( 'NONE', ( #4252, #12887, #11919, #7860 ) ) ;
#40368 = CARTESIAN_POINT ( 'NONE',  ( 159.2635086430405806, 16.19322481500868705, -10.13850573484308804 ) ) ;
#40369 = CARTESIAN_POINT ( 'NONE',  ( 31.75630755827969054, -285.9345024919887237, -299.6557161273402698 ) ) ;
#40370 = CARTESIAN_POINT ( 'NONE',  ( 155.0193446949349152, 20.65816215000725720, 12.95286603764679256 ) ) ;
#40371 = CARTESIAN_POINT ( 'NONE',  ( -109.4327953167447873, -295.5288032931941871, -256.5100406723342985 ) ) ;
#40372 = CARTESIAN_POINT ( 'NONE',  ( -10.29579733056928958, -286.8351161843877435, -339.5493368639119467 ) ) ;
#40373 = CARTESIAN_POINT ( 'NONE',  ( -114.4693872376281121, -273.8646567567205921, -270.3778293100139649 ) ) ;
#40374 = CARTESIAN_POINT ( 'NONE',  ( -95.13895651526389940, -295.2117323986929023, -222.5449353558778682 ) ) ;
#40375 = CARTESIAN_POINT ( 'NONE',  ( -43.59001445993780521, -284.4545852699117177, -194.2579191291870302 ) ) ;
#40376 = CARTESIAN_POINT ( 'NONE',  ( 11.82378249062202435, -282.3489499875647084, -215.3229881791442040 ) ) ;
#40377 = CARTESIAN_POINT ( 'NONE',  ( -38.73671833641064666, -281.3092890223567224, -346.3349815211871601 ) ) ;
#40378 = CARTESIAN_POINT ( 'NONE',  ( -68.75797821553327083, -289.4770535021120850, -336.2551045908377318 ) ) ;
#40379 = CARTESIAN_POINT ( 'NONE',  ( -38.38026192130610781, -281.4641603985535880, -196.7667147504528771 ) ) ;
#40380 = CARTESIAN_POINT ( 'NONE',  ( -67.38191867309103600, -280.4506382189260876, -203.6377586362480088 ) ) ;
#40381 = CARTESIAN_POINT ( 'NONE',  ( 35.77465287620216827, -289.2989616883940016, -252.1291205649638982 ) ) ;
#40382 = ORIENTED_EDGE ( 'NONE', *, *, #56881, .F. ) ;
#40383 = CARTESIAN_POINT ( 'NONE',  ( -68.84406436175810029, -273.6493352913957438, -200.0857731646960644 ) ) ;
#40384 = CARTESIAN_POINT ( 'NONE',  ( -97.06960495634615427, -291.9171652815668949, -315.1532361103663789 ) ) ;
#40385 = DIRECTION ( 'NONE',  ( -0.000000000000000000, -1.000000000000000000, -0.000000000000000000 ) ) ;
#40386 = CARTESIAN_POINT ( 'NONE',  ( -2.659677404128715672, -294.9805209788416391, -198.2697987213421698 ) ) ;
#40387 = EDGE_LOOP ( 'NONE', ( #76359, #71253, #83430, #35479 ) ) ;
#40388 = CARTESIAN_POINT ( 'NONE',  ( 7.135258860325478736, -274.4481728422265405, -331.0211601069844960 ) ) ;
#40389 = DIRECTION ( 'NONE',  ( 0.000000000000000000, 1.000000000000000000, 0.000000000000000000 ) ) ;
#40390 = CARTESIAN_POINT ( 'NONE',  ( -4.862215199290253587, -293.0314558350275433, -339.3067306606041029 ) ) ;
#40391 = CARTESIAN_POINT ( 'NONE',  ( -33.80207301770183648, -297.6052914145107593, -197.2998848337567495 ) ) ;
#40392 = CARTESIAN_POINT ( 'NONE',  ( -48.14366626442389219, -290.7120622004322854, -343.3099846582894656 ) ) ;
#40393 = CARTESIAN_POINT ( 'NONE',  ( -71.86191250414461251, -285.2751981996870541, -335.8311794829868973 ) ) ;
#40394 = CARTESIAN_POINT ( 'NONE',  ( -42.03603457924297260, -293.4193369162962313, -194.0946802960376374 ) ) ;
#40395 = CARTESIAN_POINT ( 'NONE',  ( -94.35506148009609717, -292.5637789856312452, -219.3437199637074571 ) ) ;
#40396 = CARTESIAN_POINT ( 'NONE',  ( -55.25814271919125531, -287.8219893323475844, -197.4788053075515109 ) ) ;
#40397 = CARTESIAN_POINT ( 'NONE',  ( -77.49432812584645092, -279.6961669607036924, -204.5972872974077177 ) ) ;
#40398 = CARTESIAN_POINT ( 'NONE',  ( -111.7172948236253944, -294.8018386491282286, -257.0350115200009213 ) ) ;
#40399 = CARTESIAN_POINT ( 'NONE',  ( -92.43521982086667776, -283.6475701645995855, -324.1542782574650232 ) ) ;
#40400 = CARTESIAN_POINT ( 'NONE',  ( 3.591611365154614877, -276.4691912798503495, -208.3696578276595233 ) ) ;
#40401 = EDGE_CURVE ( 'NONE', #79261, #4223, #89676, .T. ) ;
#40402 = CARTESIAN_POINT ( 'NONE',  ( -53.28691492658256834, -279.7662352645559736, -340.3683826091709079 ) ) ;
#40403 = CARTESIAN_POINT ( 'NONE',  ( -102.5548912273075359, -276.1799505344565659, -309.0327616309972427 ) ) ;
#40404 = DIRECTION ( 'NONE',  ( -0.000000000000000000, 0.000000000000000000, -1.000000000000000000 ) ) ;
#40405 = CARTESIAN_POINT ( 'NONE',  ( 11.95359476251294062, -281.8521149855111503, -324.2866438785825380 ) ) ;
#40406 = CARTESIAN_POINT ( 'NONE',  ( -28.63086904358489804, -278.1492243804284499, -346.5204632509078806 ) ) ;
#40407 = CARTESIAN_POINT ( 'NONE',  ( -15.46898969589202544, -285.3871377557672417, -196.7232530367633956 ) ) ;
#40408 = CARTESIAN_POINT ( 'NONE',  ( -65.73616085099284589, -293.4357610129025602, -201.9973694044729768 ) ) ;
#40409 = CARTESIAN_POINT ( 'NONE',  ( 36.11986802533294849, -277.4090978106801799, -290.6542854637510800 ) ) ;
#40410 = CARTESIAN_POINT ( 'NONE',  ( 24.91578875114059244, -276.2742263817530102, -225.8718336334627566 ) ) ;
#40411 = CARTESIAN_POINT ( 'NONE',  ( 13.72981172109277637, -276.1454707944167808, -322.5918520398628857 ) ) ;
#40412 = CARTESIAN_POINT ( 'NONE',  ( -87.70549548037645593, -297.7577978277427633, -325.7101608088385660 ) ) ;
#40413 = CARTESIAN_POINT ( 'NONE',  ( -55.16900330813625430, -283.8223120519360236, -197.6286578918427495 ) ) ;
#40414 = CARTESIAN_POINT ( 'NONE',  ( 15.42676094039337009, -292.4401136461067949, -214.2412137935257306 ) ) ;
#40415 = CARTESIAN_POINT ( 'NONE',  ( 16.13915119024753508, -289.9092719680049868, -324.7137803767968194 ) ) ;
#40416 = CARTESIAN_POINT ( 'NONE',  ( 19.59452573732196967, -291.8217036909481976, -224.1623432967442682 ) ) ;
#40417 = ORIENTED_EDGE ( 'NONE', *, *, #79684, .F. ) ;
#40418 = CARTESIAN_POINT ( 'NONE',  ( 26.01459066788044794, -291.5586767992588761, -227.5528298243347649 ) ) ;
#40419 = CARTESIAN_POINT ( 'NONE',  ( -62.80412618020993420, -291.3780441841935840, -201.9231727598370298 ) ) ;
#40420 = ORIENTED_EDGE ( 'NONE', *, *, #91737, .F. ) ;
#40421 = CARTESIAN_POINT ( 'NONE',  ( -20.55063799047649908, -289.9212195765249476, -345.2457274912503635 ) ) ;
#40422 = CARTESIAN_POINT ( 'NONE',  ( -110.1891078100415484, -278.8099528611388678, -276.0847653329869331 ) ) ;
#40423 = EDGE_CURVE ( 'NONE', #55168, #33292, #65548, .T. ) ;
#40424 = CARTESIAN_POINT ( 'NONE',  ( -104.3395860969774702, -294.9854890270951842, -307.7896247565028034 ) ) ;
#40425 = CARTESIAN_POINT ( 'NONE',  ( -63.17500931435632339, -286.3757113337703117, -197.9321671207016493 ) ) ;
#40426 = CARTESIAN_POINT ( 'NONE',  ( 18.33327024772819058, -287.1575841708763051, -217.1237175531528010 ) ) ;
#40427 = CARTESIAN_POINT ( 'NONE',  ( -110.3397370399036390, -284.8421504067744650, -273.6433171318274731 ) ) ;
#40428 = CARTESIAN_POINT ( 'NONE',  ( -95.79658185062278619, -239.9132554248992335, -341.7037225620111371 ) ) ;
#40429 = CARTESIAN_POINT ( 'NONE',  ( 152.3546084807370846, 207.1652122862846852, -216.4903851229848613 ) ) ;
#40430 = CARTESIAN_POINT ( 'NONE',  ( -77.44465942105425427, -207.6981841608007358, -353.4590041244178451 ) ) ;
#40431 = CARTESIAN_POINT ( 'NONE',  ( 34.04858704456142249, -274.9606796564495426, -286.4189444767638406 ) ) ;
#40432 = CARTESIAN_POINT ( 'NONE',  ( -11.15641801993444027, -275.6229932953943376, -338.8341570170778709 ) ) ;
#40433 = CARTESIAN_POINT ( 'NONE',  ( -87.41745026599895141, -296.8833071322984551, -211.8790237016687570 ) ) ;
#40434 = CARTESIAN_POINT ( 'NONE',  ( 139.9619883129436175, 178.0088983401332712, -238.8496011978771207 ) ) ;
#40435 = CARTESIAN_POINT ( 'NONE',  ( 29.52472329102864279, -273.7507364126847165, -233.0744592506608797 ) ) ;
#40436 = CARTESIAN_POINT ( 'NONE',  ( 9.890158678931786795, -300.5099204045154693, -196.1107481965832164 ) ) ;
#40437 = ORIENTED_EDGE ( 'NONE', *, *, #45647, .F. ) ;
#40438 = CARTESIAN_POINT ( 'NONE',  ( -35.49103812266535130, -299.0160376997106937, -193.5961227232499198 ) ) ;
#40439 = CARTESIAN_POINT ( 'NONE',  ( 35.74174720458932342, -288.0173949372725701, -268.3044774032451301 ) ) ;
#40440 = CARTESIAN_POINT ( 'NONE',  ( -53.24581842444744240, -296.0537955668417567, -345.5901275544880491 ) ) ;
#40441 = CARTESIAN_POINT ( 'NONE',  ( -57.37973956247277130, -298.2927415120119576, -196.0226145762185297 ) ) ;
#40442 = CARTESIAN_POINT ( 'NONE',  ( -82.35814173241939784, -295.8527815415696409, -327.8931211605208773 ) ) ;
#40443 = ORIENTED_EDGE ( 'NONE', *, *, #53476, .F. ) ;
#40444 = CARTESIAN_POINT ( 'NONE',  ( 28.67724042790965555, -276.9855436599220297, -233.5001720378140533 ) ) ;
#40445 = VERTEX_POINT ( 'NONE', #73267 ) ;
#40446 = CARTESIAN_POINT ( 'NONE',  ( 36.11881808418307571, -280.7722616095896910, -247.4901939255047125 ) ) ;
#40447 = CARTESIAN_POINT ( 'NONE',  ( -39.15160195528284959, -278.0166744601501705, -343.5740451481016180 ) ) ;
#40448 = CARTESIAN_POINT ( 'NONE',  ( 29.66027652668425318, -277.7829697282760435, -306.3151173462351835 ) ) ;
#40449 = CARTESIAN_POINT ( 'NONE',  ( -97.50576853219169493, -275.9546294838840481, -315.7551121345023262 ) ) ;
#40450 = CARTESIAN_POINT ( 'NONE',  ( -102.0878858124889632, -273.5060980886412949, -236.4000848177502121 ) ) ;
#40451 = CARTESIAN_POINT ( 'NONE',  ( -110.3181488619163275, -295.2559180965984638, -260.4999317729956374 ) ) ;
#40452 = DIRECTION ( 'NONE',  ( -0.000000000000000000, 1.000000000000000000, -0.000000000000000000 ) ) ;
#40453 = CARTESIAN_POINT ( 'NONE',  ( -93.60467401188311953, -278.0592409012591020, -316.8939025970711896 ) ) ;
#40454 = CARTESIAN_POINT ( 'NONE',  ( 7.631008024489784880, -287.1377911744011158, -332.3195218081207258 ) ) ;
#40455 = CARTESIAN_POINT ( 'NONE',  ( -88.80940629332599201, -275.3300913463501729, -215.7367503887411431 ) ) ;
#40456 = CARTESIAN_POINT ( 'NONE',  ( 194.9499353771399512, 21.00000000000000711, -15.36943343683466168 ) ) ;
#40457 = CARTESIAN_POINT ( 'NONE',  ( -110.5290694898110786, -289.7745044645415078, -268.4473571145647952 ) ) ;
#40458 = CARTESIAN_POINT ( 'NONE',  ( -108.9305434241827868, -284.2587602294238422, -242.1387700534701253 ) ) ;
#40459 = CARTESIAN_POINT ( 'NONE',  ( 14.62036482676534277, -280.5487155508267847, -323.1392121425904520 ) ) ;
#40461 = CARTESIAN_POINT ( 'NONE',  ( -110.6060182635314817, -282.8033965623482686, -257.1117573864958672 ) ) ;
#40460 = CARTESIAN_POINT ( 'NONE',  ( 21.81336857316339817, -279.5178411778748568, -226.5671628940422977 ) ) ;
#40462 = CARTESIAN_POINT ( 'NONE',  ( -92.75689809185595891, -287.2583514653211978, -219.7476696729253831 ) ) ;
#40463 = CARTESIAN_POINT ( 'NONE',  ( -108.3606650943867038, -280.0011652209780095, -251.7796529776460375 ) ) ;
#40464 = PLANE ( 'NONE',  #30672 ) ;
#40465 = CARTESIAN_POINT ( 'NONE',  ( -58.40212359098838846, -293.7800610223805506, -198.3787645216934550 ) ) ;
#40466 = CARTESIAN_POINT ( 'NONE',  ( -84.25855566230353588, -275.9269049178594173, -330.2007504250416332 ) ) ;
#40467 = CIRCLE ( 'NONE', #51122, 1.000000000000000888 ) ;
#40468 = CARTESIAN_POINT ( 'NONE',  ( 20.10771294275045307, -276.8405362612841145, -315.5858990672146547 ) ) ;
#40469 = CARTESIAN_POINT ( 'NONE',  ( -109.7191243327464889, -286.2919024100184515, -290.6474901065458880 ) ) ;
#40470 = CARTESIAN_POINT ( 'NONE',  ( 196.0143093133015384, 73.40565171261611965, 12.00000000000000888 ) ) ;
#40471 = CARTESIAN_POINT ( 'NONE',  ( -98.68660627855595635, -291.8761455077942060, -314.4980886571906922 ) ) ;
#40472 = CARTESIAN_POINT ( 'NONE',  ( -110.3999686194082273, -294.7703480519206209, -253.3500042728492474 ) ) ;
#40473 = CARTESIAN_POINT ( 'NONE',  ( 11.98177109736971424, -285.9145420156942237, -211.3734829468599798 ) ) ;
#40474 = CARTESIAN_POINT ( 'NONE',  ( -72.99576474426503125, -289.9715889860896141, -205.6876940265083817 ) ) ;
#40475 = DIRECTION ( 'NONE',  ( 0.000000000000000000, 0.000000000000000000, -1.000000000000000000 ) ) ;
#40476 = CARTESIAN_POINT ( 'NONE',  ( -29.67854612603656506, -275.6380597814648468, -343.5049080530640140 ) ) ;
#40477 = CARTESIAN_POINT ( 'NONE',  ( 31.72622290130566114, -292.0512403567969386, -297.7135479350594096 ) ) ;
#40478 =( NAMED_UNIT ( * ) SI_UNIT ( $, .STERADIAN. ) SOLID_ANGLE_UNIT ( ) );
#40479 = FACE_OUTER_BOUND ( 'NONE', #67946, .T. ) ;
#40480 = CARTESIAN_POINT ( 'NONE',  ( -74.32575318812952503, -290.0494452150384177, -203.6161738099156651 ) ) ;
#40481 = CARTESIAN_POINT ( 'NONE',  ( -97.23588749016070665, -286.7489214668028694, -227.2219598302695829 ) ) ;
#40482 = CARTESIAN_POINT ( 'NONE',  ( 18.85946758155182934, -286.4965487575751695, -321.5215008779105688 ) ) ;
#40483 = EDGE_CURVE ( 'NONE', #68325, #33225, #29218, .T. ) ;
#40484 = CARTESIAN_POINT ( 'NONE',  ( -95.43329365003492626, -286.6090191479946725, -225.1660816910496976 ) ) ;
#40485 = CARTESIAN_POINT ( 'NONE',  ( 152.0194914954574870, 20.99319818809533089, -6.266237208439005890 ) ) ;
#40486 = CARTESIAN_POINT ( 'NONE',  ( -72.46048734633099286, -286.3775635797292125, -206.1653101529586252 ) ) ;
#40487 = CARTESIAN_POINT ( 'NONE',  ( 28.03584519350161486, -295.0345271441481714, -232.8886832041147272 ) ) ;
#40488 = CARTESIAN_POINT ( 'NONE',  ( -81.72064975485658067, -275.7311126363377412, -331.5152104494140417 ) ) ;
#40489 = CARTESIAN_POINT ( 'NONE',  ( 1.040175331164154837, -276.8881083073920877, -337.1492061974268495 ) ) ;
#40490 = CARTESIAN_POINT ( 'NONE',  ( 28.23820088301792808, -291.1351089485606849, -232.8299205701479480 ) ) ;
#40491 = CARTESIAN_POINT ( 'NONE',  ( -113.7171041604738235, -278.6796328718843370, -260.1678642953070266 ) ) ;
#40492 = CARTESIAN_POINT ( 'NONE',  ( -110.9009413954952947, -298.6956820249556017, -257.6770796488139581 ) ) ;
#40493 = FACE_OUTER_BOUND ( 'NONE', #80313, .T. ) ;
#40494 = DIRECTION ( 'NONE',  ( -1.000000000000000000, 0.000000000000000000, 0.000000000000000000 ) ) ;
#40495 = CARTESIAN_POINT ( 'NONE',  ( 26.80594827739740182, -285.7484557002154588, -234.3916127602344375 ) ) ;
#40496 = CARTESIAN_POINT ( 'NONE',  ( -93.67924623238455695, -276.0149791513286459, -318.7030912706692334 ) ) ;
#40497 = CARTESIAN_POINT ( 'NONE',  ( 7.979459066525541822, -280.4325612937215055, -330.1189055501071152 ) ) ;
#40498 = CARTESIAN_POINT ( 'NONE',  ( 195.8725848201698341, 20.33787691583836121, -12.24547402278110475 ) ) ;
#40499 = CARTESIAN_POINT ( 'NONE',  ( 35.92565659406344025, -273.7601160794806106, -248.8549011955632011 ) ) ;
#40500 = CARTESIAN_POINT ( 'NONE',  ( 36.40189667974279075, -295.0772904531303311, -270.7443910423835973 ) ) ;
#40501 = CARTESIAN_POINT ( 'NONE',  ( 10.64036638886969399, -279.6174766508252105, -210.4665103505161881 ) ) ;
#40502 = CARTESIAN_POINT ( 'NONE',  ( -0.6296499342777925889, -295.4931339881433701, -333.7880307336682790 ) ) ;
#40503 = CARTESIAN_POINT ( 'NONE',  ( -43.26837292597443962, -299.2940981986686211, -194.0313000994881918 ) ) ;
#40504 = CARTESIAN_POINT ( 'NONE',  ( -49.95183219354460391, -297.7200718570109075, -198.4585132051433050 ) ) ;
#40505 = CARTESIAN_POINT ( 'NONE',  ( -96.71282231959645515, -293.1802604351744321, -224.5345917946154657 ) ) ;
#40506 = CARTESIAN_POINT ( 'NONE',  ( -114.2082025277494495, -284.6518129132633135, -275.7198953307047873 ) ) ;
#40507 = CARTESIAN_POINT ( 'NONE',  ( 31.88146062820246840, -274.0912307523720415, -301.1581875313318619 ) ) ;
#40508 = CARTESIAN_POINT ( 'NONE',  ( 22.40379876867637066, -288.0373573276025354, -318.9562992615146300 ) ) ;
#40509 = CARTESIAN_POINT ( 'NONE',  ( -109.5704045308657300, -280.7758564129747469, -251.4730877253806227 ) ) ;
#40510 = EDGE_CURVE ( 'NONE', #56465, #48629, #80814, .T. ) ;
#40511 = CARTESIAN_POINT ( 'NONE',  ( 33.25927934050767476, -286.3545114275828496, -250.8955035135419394 ) ) ;
#40512 = AXIS2_PLACEMENT_3D ( 'NONE', #12870, #4801, #78192 ) ;
#40513 = CARTESIAN_POINT ( 'NONE',  ( -70.00311722843157725, -289.6217537687813319, -202.8464344932358756 ) ) ;
#40514 = ORIENTED_EDGE ( 'NONE', *, *, #50161, .F. ) ;
#40515 = CARTESIAN_POINT ( 'NONE',  ( 202.9737475146022803, 296.4636489462809550, -68.70538243550777224 ) ) ;
#40516 = CARTESIAN_POINT ( 'NONE',  ( -63.84906443871414439, -288.9148660919514668, -338.4987413868928456 ) ) ;
#40517 = CARTESIAN_POINT ( 'NONE',  ( 175.2296996224750103, 275.5000000000000568, 0.000000000000000000 ) ) ;
#40518 = CARTESIAN_POINT ( 'NONE',  ( -113.3646300933064310, -285.3551472233727964, -281.3820153497404704 ) ) ;
#40519 = CARTESIAN_POINT ( 'NONE',  ( 38.12372545427202652, -292.7882204973093963, -284.4958596535534525 ) ) ;
#40520 = CARTESIAN_POINT ( 'NONE',  ( -2.771482224829393548, -282.1015196705236576, -202.4396936741175068 ) ) ;
#40521 = CARTESIAN_POINT ( 'NONE',  ( 3.544184392830691088, -281.9045571321730108, -205.6329256421611831 ) ) ;
#40522 = CARTESIAN_POINT ( 'NONE',  ( -99.03217298471201957, -283.8449955845227919, -309.4850459206065239 ) ) ;
#40523 = CARTESIAN_POINT ( 'NONE',  ( 33.95532903960647531, -277.2497541240009014, -246.9190415777997032 ) ) ;
#40524 = CARTESIAN_POINT ( 'NONE',  ( -111.5920180545969487, -296.2966965220631437, -290.7545063182770946 ) ) ;
#40525 = CARTESIAN_POINT ( 'NONE',  ( -111.2551153722055943, -288.4365953186446632, -280.8767514242893526 ) ) ;
#40526 = UNCERTAINTY_MEASURE_WITH_UNIT (LENGTH_MEASURE( 1.000000000000000082E-05 ), #42925, 'distance_accuracy_value', 'NONE');
#40527 = CARTESIAN_POINT ( 'NONE',  ( -55.35637588449080937, -296.7353487853002321, -199.2473648627412786 ) ) ;
#40528 = ORIENTED_EDGE ( 'NONE', *, *, #72819, .T. ) ;
#40529 = ORIENTED_EDGE ( 'NONE', *, *, #84969, .T. ) ;
#40530 = DIRECTION ( 'NONE',  ( 0.000000000000000000, 0.000000000000000000, -1.000000000000000000 ) ) ;
#40531 = CARTESIAN_POINT ( 'NONE',  ( -101.6327459194991008, -285.9672571081932233, -307.8841192875752313 ) ) ;
#40532 = CARTESIAN_POINT ( 'NONE',  ( 35.19854032246905717, -294.9485850551409953, -295.4118100418284598 ) ) ;
#40533 = CARTESIAN_POINT ( 'NONE',  ( -24.03881859366369866, -283.5291427728764688, -342.2424508217943639 ) ) ;
#40534 = EDGE_CURVE ( 'NONE', #26246, #60290, #68553, .T. ) ;
#40535 = CARTESIAN_POINT ( 'NONE',  ( -14.67065778551407007, -275.8242278882383971, -343.7573731311840675 ) ) ;
#40536 = CARTESIAN_POINT ( 'NONE',  ( -61.66421543717697773, -292.3957656360024657, -197.3548582175833133 ) ) ;
#40537 = CARTESIAN_POINT ( 'NONE',  ( -109.7385879705670959, -282.9788843252323431, -247.8464965693437136 ) ) ;
#40538 = CARTESIAN_POINT ( 'NONE',  ( 34.44157193075682954, -293.5314807704896225, -242.4126424116990961 ) ) ;
#40539 = CARTESIAN_POINT ( 'NONE',  ( -110.3581415829500685, -290.8745066167260802, -271.1898302038484871 ) ) ;
#40540 = DIRECTION ( 'NONE',  ( 0.000000000000000000, 0.000000000000000000, 1.000000000000000000 ) ) ;
#40541 = CARTESIAN_POINT ( 'NONE',  ( 144.2857639756989272, -299.5541904835127980, -195.3611179825600175 ) ) ;
#40542 = CARTESIAN_POINT ( 'NONE',  ( -110.7270578385798956, -271.3603141859142625, -270.3459430301334123 ) ) ;
#40543 = CARTESIAN_POINT ( 'NONE',  ( -66.29508407243339718, -284.9444860100746268, -340.9755235858550577 ) ) ;
#40544 = CARTESIAN_POINT ( 'NONE',  ( 10.64812456238590777, -290.1952119285920162, -210.2361428286349110 ) ) ;
#40545 = ORIENTED_EDGE ( 'NONE', *, *, #93286, .F. ) ;
#40546 = CARTESIAN_POINT ( 'NONE',  ( 34.78712304438143121, -280.6455069174771211, -283.5332544925073535 ) ) ;
#40547 = CARTESIAN_POINT ( 'NONE',  ( 37.88410771017887413, -275.4239870848458622, -286.7573799586867267 ) ) ;
#40548 = CARTESIAN_POINT ( 'NONE',  ( -80.12332178592984633, -281.4716564351134593, -208.9627363069155308 ) ) ;
#40549 = CARTESIAN_POINT ( 'NONE',  ( 186.8753510093225998, 261.0767047533620371, -152.2190506625686908 ) ) ;
#40550 = CARTESIAN_POINT ( 'NONE',  ( 18.74012657635215717, -279.4145279068767422, -218.4628038820436586 ) ) ;
#40551 = CARTESIAN_POINT ( 'NONE',  ( -111.2370329669978304, -282.7083774618300822, -259.8099764580837814 ) ) ;
#40552 = CARTESIAN_POINT ( 'NONE',  ( -111.2437865561877146, -274.6247840391680484, -253.6641989065475684 ) ) ;
#40553 = PRODUCT_DEFINITION_SHAPE ( 'NONE', 'NONE',  #21587 ) ;
#40554 = CARTESIAN_POINT ( 'NONE',  ( -108.6505628435897535, -296.8348368039759748, -286.2681774248567308 ) ) ;
#40555 = VERTEX_POINT ( 'NONE', #68008 ) ;
#40556 = CARTESIAN_POINT ( 'NONE',  ( -75.21951289112031702, -290.2210918988385515, -207.3214384937482180 ) ) ;
#40557 = CARTESIAN_POINT ( 'NONE',  ( -59.62753349954910220, -277.9848474905833200, -343.9590419836419528 ) ) ;
#40558 = CARTESIAN_POINT ( 'NONE',  ( 15.44679013974579718, -274.8241358229439015, -219.8659723707438616 ) ) ;
#40559 = CARTESIAN_POINT ( 'NONE',  ( 36.58396856470844227, -274.7297310031748907, -290.8180893102337450 ) ) ;
#40560 = CARTESIAN_POINT ( 'NONE',  ( 185.2169494693457921, 214.5000000000000568, 22.91843887563416615 ) ) ;
#40561 = CARTESIAN_POINT ( 'NONE',  ( -36.25426203478412646, -272.0655934628214254, -195.3563857614199435 ) ) ;
#40562 = EDGE_CURVE ( 'NONE', #2640, #11817, #24924, .T. ) ;
#40563 = DIRECTION ( 'NONE',  ( 0.000000000000000000, 1.000000000000000000, 0.000000000000000000 ) ) ;
#40564 = CARTESIAN_POINT ( 'NONE',  ( 197.0359635097987336, 71.72764050496320465, 10.24344765925977185 ) ) ;
#40565 = CARTESIAN_POINT ( 'NONE',  ( -26.68430800845607109, -283.9932177593421443, -342.9429474339771104 ) ) ;
#40566 = CARTESIAN_POINT ( 'NONE',  ( 8.614004824853640940, -284.1922577934084870, -330.8759689996251723 ) ) ;
#40567 = CARTESIAN_POINT ( 'NONE',  ( -109.0811241229871911, -283.7156780926910642, -284.4091681444114670 ) ) ;
#40568 = CARTESIAN_POINT ( 'NONE',  ( -39.19808882758704982, -275.4757051602846900, -344.1377690184856988 ) ) ;
#40569 = CARTESIAN_POINT ( 'NONE',  ( 21.16892235343681250, -284.0457944349898298, -316.0488903129968321 ) ) ;
#40570 = CARTESIAN_POINT ( 'NONE',  ( -101.1931572631044105, -276.5310926147301416, -307.2563026382189832 ) ) ;
#40571 = CARTESIAN_POINT ( 'NONE',  ( 165.2494399300530290, 8.542400036368780647, 9.000000000000001776 ) ) ;
#40572 = CARTESIAN_POINT ( 'NONE',  ( 20.91885401849723536, -276.0084445527244270, -225.8440116718224999 ) ) ;
#40573 = CARTESIAN_POINT ( 'NONE',  ( 194.7497628521415152, 41.36675632506837985, 13.96383658842646014 ) ) ;
#40574 = CARTESIAN_POINT ( 'NONE',  ( -72.44218635038427578, -280.4024167310073494, -201.9936276683974086 ) ) ;
#40575 = ORIENTED_EDGE ( 'NONE', *, *, #49238, .F. ) ;
#40576 = ORIENTED_EDGE ( 'NONE', *, *, #53799, .T. ) ;
#40577 = CARTESIAN_POINT ( 'NONE',  ( 200.1633050441426747, 15.87263057655181520, 10.05743975622734787 ) ) ;
#40578 = CARTESIAN_POINT ( 'NONE',  ( -104.3508886181872271, -286.8777724704187335, -234.8923316433779291 ) ) ;
#40579 = CARTESIAN_POINT ( 'NONE',  ( -72.21052236660966628, -294.7230507547126308, -334.6931227954037240 ) ) ;
#40580 = CARTESIAN_POINT ( 'NONE',  ( -96.31822571377115594, -289.2355750275310129, -319.7280971465426660 ) ) ;
#40581 = CARTESIAN_POINT ( 'NONE',  ( 36.66826209343179244, -285.8011989209114745, -271.0678731423714680 ) ) ;
#40583 = CARTESIAN_POINT ( 'NONE',  ( -60.55582111289538005, -289.9868797404074030, -200.0287696616872779 ) ) ;
#40582 = CARTESIAN_POINT ( 'NONE',  ( -44.06024607761280976, -284.5402646378329337, -197.0792235106676173 ) ) ;
#40584 = CIRCLE ( 'NONE', #20957, 25.00000000000000355 ) ;
#40585 = CARTESIAN_POINT ( 'NONE',  ( -100.7364163632577743, -285.2522939534815123, -307.3508524710385359 ) ) ;
#40586 = CARTESIAN_POINT ( 'NONE',  ( 36.75576178132580907, -273.4019796768719175, -258.6778656054111138 ) ) ;
#40587 = CARTESIAN_POINT ( 'NONE',  ( 38.55977574400233010, -285.8596861223417136, -263.0544528729133731 ) ) ;
#40588 = CARTESIAN_POINT ( 'NONE',  ( -72.36982823571389645, -299.5891824997087838, -203.9861367232120983 ) ) ;
#40589 = CARTESIAN_POINT ( 'NONE',  ( 20.07181748108543573, -286.2215906927706897, -318.8762334154830000 ) ) ;
#40590 = CARTESIAN_POINT ( 'NONE',  ( 20.69506519269020117, -281.8665436756331815, -225.6737248417511807 ) ) ;
#40591 = CARTESIAN_POINT ( 'NONE',  ( -88.23111489452762157, -291.7630158040153674, -325.6810591336947596 ) ) ;
#40592 = DIRECTION ( 'NONE',  ( 0.000000000000000000, -1.000000000000000000, 0.000000000000000000 ) ) ;
#40593 = CARTESIAN_POINT ( 'NONE',  ( 195.5719271795211682, 40.32756825300102577, 13.76475510248965684 ) ) ;
#40594 = CARTESIAN_POINT ( 'NONE',  ( -71.40261072835853895, -297.4185974406583455, -337.8086425525673917 ) ) ;
#40595 = CARTESIAN_POINT ( 'NONE',  ( -99.64110039250881812, -277.1176352738476680, -228.5102880108437660 ) ) ;
#40596 = CARTESIAN_POINT ( 'NONE',  ( 20.26442346843702680, -292.0591352435089902, -219.4915230163975082 ) ) ;
#40597 = CARTESIAN_POINT ( 'NONE',  ( -77.93519425016025082, -295.8969572855212391, -208.6668662079475780 ) ) ;
#40598 = CARTESIAN_POINT ( 'NONE',  ( 12.23711621012914996, -281.0294206572767735, -324.6122419106225152 ) ) ;
#40599 = CARTESIAN_POINT ( 'NONE',  ( 14.51702123860494531, -272.8686128865963951, -216.9571179955988214 ) ) ;
#40600 = CARTESIAN_POINT ( 'NONE',  ( 29.17779792781686510, -294.4466323721616163, -238.9936709406285331 ) ) ;
#40601 = CARTESIAN_POINT ( 'NONE',  ( -54.49178911615188525, -294.3376638359845288, -195.3683826091709363 ) ) ;
#40602 = CARTESIAN_POINT ( 'NONE',  ( -109.6945093321504459, -294.7239762540878587, -294.6052668116122391 ) ) ;
#40603 = CARTESIAN_POINT ( 'NONE',  ( 37.33360845913221482, -291.6138812920016221, -256.3050764695099133 ) ) ;
#40604 = CARTESIAN_POINT ( 'NONE',  ( -99.32839922685357692, -291.4331961887654074, -310.0224852261586648 ) ) ;
#40605 = DIRECTION ( 'NONE',  ( -1.000000000000000000, 0.000000000000000000, 0.000000000000000000 ) ) ;
#40606 = CARTESIAN_POINT ( 'NONE',  ( -17.39837761794011683, -293.1188738049671088, -199.9176053912980819 ) ) ;
#40608 = CARTESIAN_POINT ( 'NONE',  ( -36.20613000907598433, -292.0667459473677354, -197.3574743847684942 ) ) ;
#40607 = CARTESIAN_POINT ( 'NONE',  ( -2.419275701860534422, -280.6125310240805106, -337.1355972223573758 ) ) ;
#40609 = CARTESIAN_POINT ( 'NONE',  ( 35.32768634397170615, -281.2292449773694898, -244.7428761329562690 ) ) ;
#40610 = CARTESIAN_POINT ( 'NONE',  ( -95.32160518925131498, -283.5338528613874587, -320.9978131815226448 ) ) ;
#40611 = CARTESIAN_POINT ( 'NONE',  ( -15.33625967234313592, -286.7665914083011671, -341.9400072225873828 ) ) ;
#40612 = CARTESIAN_POINT ( 'NONE',  ( -15.79625802500858534, -280.9100225573880607, -341.4009617520089819 ) ) ;
#40613 = CARTESIAN_POINT ( 'NONE',  ( -38.14302996174868099, -278.5221656627724087, -194.0586565157570078 ) ) ;
#40614 = CARTESIAN_POINT ( 'NONE',  ( 3.005770047155969404, -287.4446158750764084, -335.6428392101049099 ) ) ;
#40615 = CARTESIAN_POINT ( 'NONE',  ( 195.8990914565195567, 41.11444846156542354, 14.40741235656477848 ) ) ;
#40616 = CARTESIAN_POINT ( 'NONE',  ( 20.80070679906746989, -294.5182937766302871, -224.8884830366427252 ) ) ;
#40617 = CARTESIAN_POINT ( 'NONE',  ( -35.70578721796089638, -278.4573057941085494, -346.7674003240754246 ) ) ;
#40618 = CARTESIAN_POINT ( 'NONE',  ( -37.81415524445844767, -276.7249124765496617, -343.3931900727663447 ) ) ;
#40619 = CARTESIAN_POINT ( 'NONE',  ( 39.50230333779012426, -293.7898169480481556, -276.0370319631380198 ) ) ;
#40620 = CARTESIAN_POINT ( 'NONE',  ( -76.04178007673230866, -281.6443055688143886, -335.3187718231940266 ) ) ;
#40621 = CARTESIAN_POINT ( 'NONE',  ( 34.00192346484114836, -292.8290136197932156, -286.9540339595770888 ) ) ;
#40622 = EDGE_CURVE ( 'NONE', #10254, #11793, #5017, .T. ) ;
#40623 = CARTESIAN_POINT ( 'NONE',  ( -111.4102552849610959, -294.7043319699102994, -258.4964773301505829 ) ) ;
#40624 = VERTEX_POINT ( 'NONE', #65352 ) ;
#40625 = FACE_OUTER_BOUND ( 'NONE', #64878, .T. ) ;
#40626 = CARTESIAN_POINT ( 'NONE',  ( 35.68303615358379943, -293.0292401754815614, -268.0424260105511962 ) ) ;
#40627 = CARTESIAN_POINT ( 'NONE',  ( -102.0172624299487154, -282.4809262143061233, -239.1787733560258289 ) ) ;
#40628 = CARTESIAN_POINT ( 'NONE',  ( -57.31690184651372988, -296.8593730560855306, -196.1857602132345733 ) ) ;
#40629 = CARTESIAN_POINT ( 'NONE',  ( 37.04651610637017001, -279.5090048715456987, -255.9840957467037299 ) ) ;
#40630 = CARTESIAN_POINT ( 'NONE',  ( 4.893391828027300328, -287.9246822947409328, -206.5054303329810637 ) ) ;
#40631 = CARTESIAN_POINT ( 'NONE',  ( -82.54792958280471282, -289.5231336466910079, -327.6794991789068945 ) ) ;
#40632 = CARTESIAN_POINT ( 'NONE',  ( -110.6579623673950294, -280.1759807848645778, -262.4254115385907085 ) ) ;
#40633 = CARTESIAN_POINT ( 'NONE',  ( -76.54284540983506702, -293.5990747032025183, -333.9439604949582758 ) ) ;
#40634 = CARTESIAN_POINT ( 'NONE',  ( 53.20184915273028281, -300.9609013388575249, -196.3202096819806002 ) ) ;
#40635 = CARTESIAN_POINT ( 'NONE',  ( -108.8767090927624679, -277.1308054369759475, -286.8446781887727184 ) ) ;
#40636 = ORIENTED_EDGE ( 'NONE', *, *, #47942, .T. ) ;
#40637 = CARTESIAN_POINT ( 'NONE',  ( -31.90712548919840685, -297.7851723854034276, -193.3825591744275982 ) ) ;
#40638 = CARTESIAN_POINT ( 'NONE',  ( -107.0678953280349219, -292.8150604373320220, -244.1461216927069700 ) ) ;
#40639 = CARTESIAN_POINT ( 'NONE',  ( 21.68005793977844320, -295.8061720122201450, -318.5777965286123958 ) ) ;
#40640 = CARTESIAN_POINT ( 'NONE',  ( 197.5461146820061060, 68.31320778629316237, -9.184551779179372488 ) ) ;
#40641 = CARTESIAN_POINT ( 'NONE',  ( -109.5184244067401664, -291.0498052471228903, -282.0334650613423264 ) ) ;
#40642 = CARTESIAN_POINT ( 'NONE',  ( -48.18343439339133027, -254.4585890652104467, -456.4660217814370071 ) ) ;
#40643 = ORIENTED_EDGE ( 'NONE', *, *, #4507, .F. ) ;
#40644 = CARTESIAN_POINT ( 'NONE',  ( -89.54520047544303907, -297.9910159113310897, -213.8256508201602344 ) ) ;
#40645 = CARTESIAN_POINT ( 'NONE',  ( -100.6387728551556080, -289.2491460361017630, -228.6282578355832129 ) ) ;
#40646 = CIRCLE ( 'NONE', #5897, 25.00000000000000355 ) ;
#40647 = CARTESIAN_POINT ( 'NONE',  ( -100.7356617306175082, -297.4623617054941178, -226.6693137411275529 ) ) ;
#40648 = FACE_OUTER_BOUND ( 'NONE', #20665, .T. ) ;
#40649 = CARTESIAN_POINT ( 'NONE',  ( 197.1513938986460062, -142.7221692137691775, 1.978481845683761620 ) ) ;
#40650 = CARTESIAN_POINT ( 'NONE',  ( 0.3934302980274854145, -290.0794218272779403, -336.7440416135048622 ) ) ;
#40651 = CARTESIAN_POINT ( 'NONE',  ( -2.602324593224680793, -285.1233781216987495, -342.4248175857292154 ) ) ;
#40652 = CARTESIAN_POINT ( 'NONE',  ( -111.8216786182747029, -286.6523929862374871, -262.5842240417235871 ) ) ;
#40653 = CARTESIAN_POINT ( 'NONE',  ( 38.39367995880343187, -285.9991284681446473, -260.2241314648887283 ) ) ;
#40654 = CARTESIAN_POINT ( 'NONE',  ( -27.01254004751618609, -272.1834772602756516, -196.1918913530755333 ) ) ;
#40655 = CARTESIAN_POINT ( 'NONE',  ( -105.7117979925263143, -274.8618111726309508, -240.7881760963864792 ) ) ;
#40656 = CARTESIAN_POINT ( 'NONE',  ( -104.8521996805456382, -289.0471803197867757, -238.9979764772720330 ) ) ;
#40657 = CARTESIAN_POINT ( 'NONE',  ( -97.80316935413354429, -279.7943165631121474, -316.0410954951530584 ) ) ;
#40658 = EDGE_LOOP ( 'NONE', ( #93690, #70994, #37524, #38730 ) ) ;
#40660 = CARTESIAN_POINT ( 'NONE',  ( 30.11874429890719185, -280.5235231508592619, -242.2011977837823622 ) ) ;
#40659 = CARTESIAN_POINT ( 'NONE',  ( -54.49278902472478592, -279.8257284137872034, -199.3523133290802889 ) ) ;
#40661 = CARTESIAN_POINT ( 'NONE',  ( 30.27703999937892121, -277.1026094226147052, -306.6561325203267643 ) ) ;
#40662 = CARTESIAN_POINT ( 'NONE',  ( -1.308577264840212084, -279.3142500762873510, -202.7621329596578619 ) ) ;
#40663 = CARTESIAN_POINT ( 'NONE',  ( 200.9738562182569694, 293.9636489450776367, -53.99999999999825917 ) ) ;
#40664 = CARTESIAN_POINT ( 'NONE',  ( 33.97014131456837305, -276.8566111095771589, -298.9200024418319117 ) ) ;
#40665 = EDGE_CURVE ( 'NONE', #75656, #93680, #36437, .T. ) ;
#40666 = ITEM_DEFINED_TRANSFORMATION ( 'NONE', 'NONE', #70334,  #18940 ) ;
#40667 = CARTESIAN_POINT ( 'NONE',  ( -1.643150907947507955, -276.0366957834737036, -202.9198743873436115 ) ) ;
#40668 = CARTESIAN_POINT ( 'NONE',  ( -54.49178911615187815, -294.3376638359846424, -195.3683826091709363 ) ) ;
#40669 = EDGE_LOOP ( 'NONE', ( #62976, #23068, #88765, #8866 ) ) ;
#40670 = CARTESIAN_POINT ( 'NONE',  ( 179.1465552314772083, 8.542400036368780647, 9.000000000000001776 ) ) ;
#40671 = CARTESIAN_POINT ( 'NONE',  ( -3.210252635886408079, -289.6702356716222653, -335.2962361339669428 ) ) ;
#40672 = CARTESIAN_POINT ( 'NONE',  ( 36.84063434880250298, -289.5216498450827771, -286.8813165054038450 ) ) ;
#40673 = CARTESIAN_POINT ( 'NONE',  ( -95.03612878912406359, -289.2689279304526622, -315.2728316886317543 ) ) ;
#40674 = CARTESIAN_POINT ( 'NONE',  ( -67.15941828578772288, -285.1792073163438204, -199.4355895234700142 ) ) ;
#40675 = CARTESIAN_POINT ( 'NONE',  ( 200.5254236182467764, 215.0000000000001705, -2.961736701814141171 ) ) ;
#40676 = CARTESIAN_POINT ( 'NONE',  ( 33.72437283331294822, -280.2122097568085337, -290.2622156956471144 ) ) ;
#40677 = CARTESIAN_POINT ( 'NONE',  ( 20.49042084099458805, -290.0596203061363667, -316.9047670461927737 ) ) ;
#40678 = CARTESIAN_POINT ( 'NONE',  ( 10.34273089995996919, -280.8603152822681182, -326.6145316231485936 ) ) ;
#40679 = CARTESIAN_POINT ( 'NONE',  ( -77.10264685039649635, -280.8225987254154461, -208.4917825281967794 ) ) ;
#40680 = CARTESIAN_POINT ( 'NONE',  ( -66.82174787274989569, -277.9415405047414538, -337.2110635830526348 ) ) ;
#40681 = CARTESIAN_POINT ( 'NONE',  ( -113.7178966205537449, -289.2648225317471429, -276.9043214449955030 ) ) ;
#40682 = CARTESIAN_POINT ( 'NONE',  ( -112.3652097174486073, -285.1469110143468697, -286.9632814028813641 ) ) ;
#40683 = CARTESIAN_POINT ( 'NONE',  ( -67.85118003366478945, -283.9343592434242964, -340.9918374979868076 ) ) ;
#40684 = CARTESIAN_POINT ( 'NONE',  ( 29.31532614387689151, -282.1211010912938377, -300.2483198753235456 ) ) ;
#40685 = EDGE_LOOP ( 'NONE', ( #91567, #82011, #82294, #69445 ) ) ;
#40686 = CARTESIAN_POINT ( 'NONE',  ( 180.5131398354828320, 276.0000000000000568, -23.92352941176473635 ) ) ;
#40687 = CARTESIAN_POINT ( 'NONE',  ( -110.0535167177606155, -292.6839593943728346, -249.0703404102804654 ) ) ;
#40688 = CARTESIAN_POINT ( 'NONE',  ( 24.42627313287446000, -291.6337850748248570, -225.2167301482050163 ) ) ;
#40689 = CARTESIAN_POINT ( 'NONE',  ( -0.4173147049840161826, -273.6147202248304211, -207.1009397883750296 ) ) ;
#40690 = CARTESIAN_POINT ( 'NONE',  ( -33.44830585809430801, -294.3529690140140929, -347.1736618969711685 ) ) ;
#40691 = CARTESIAN_POINT ( 'NONE',  ( -93.96021457574521207, -289.6952014970873392, -223.1709725755519855 ) ) ;
#40692 = CARTESIAN_POINT ( 'NONE',  ( -10.13811898126777145, -292.9319344913764667, -339.1938077947906436 ) ) ;
#40693 = CARTESIAN_POINT ( 'NONE',  ( -37.25221129623628258, -290.2560850006350393, -343.7581376632795696 ) ) ;
#40694 = DIRECTION ( 'NONE',  ( -1.000000000000000000, -0.000000000000000000, -0.000000000000000000 ) ) ;
#40695 = CARTESIAN_POINT ( 'NONE',  ( -98.23125718123426964, -291.9561389976308874, -314.1719512147217301 ) ) ;
#40696 = CARTESIAN_POINT ( 'NONE',  ( -6.612550951882577799, -290.4544925747460979, -201.7487136718380611 ) ) ;
#40697 = CARTESIAN_POINT ( 'NONE',  ( 35.89474624726534557, -295.7605949643664189, -286.5878766716460859 ) ) ;
#40698 = CARTESIAN_POINT ( 'NONE',  ( -94.31261987028145199, -286.1423031798886996, -224.3225163270527958 ) ) ;
#40699 = CARTESIAN_POINT ( 'NONE',  ( 24.22794957966838680, -296.1366013379931132, -313.5021101504153194 ) ) ;
#40700 = CARTESIAN_POINT ( 'NONE',  ( -46.70221885926734728, -275.9137635942802262, -195.5895492525627049 ) ) ;
#40701 = CARTESIAN_POINT ( 'NONE',  ( 20.51024390910566098, -275.0293340262962829, -320.5921328273016115 ) ) ;
#40702 = CARTESIAN_POINT ( 'NONE',  ( -35.82182847936549308, -297.2678989818052742, -193.5227940414692682 ) ) ;
#40703 = CARTESIAN_POINT ( 'NONE',  ( -54.20631320576049461, -275.5114118493416981, -342.4803362891933034 ) ) ;
#40704 = CARTESIAN_POINT ( 'NONE',  ( -72.79440827390649815, -277.6585137550201807, -204.9056393367679902 ) ) ;
#40705 = CARTESIAN_POINT ( 'NONE',  ( -81.32113580075613868, -274.6444572359360450, -211.5356136496031922 ) ) ;
#40706 = CARTESIAN_POINT ( 'NONE',  ( -18.67620321177383502, -272.8625595547588887, -196.2105848871857461 ) ) ;
#40707 = CARTESIAN_POINT ( 'NONE',  ( -109.6278670026663491, -298.1587260822187773, -256.5067882255931409 ) ) ;
#40708 = CARTESIAN_POINT ( 'NONE',  ( 196.8409580319986674, 73.46773880466290052, 12.56795567929779622 ) ) ;
#40709 = CARTESIAN_POINT ( 'NONE',  ( -69.33736392543778493, -298.4228197239996234, -204.5668991960239964 ) ) ;
#40710 = VECTOR ( 'NONE', #64231, 1000.000000000000000 ) ;
#40711 = DIRECTION ( 'NONE',  ( 0.000000000000000000, 1.000000000000000000, 0.000000000000000000 ) ) ;
#40713 = CARTESIAN_POINT ( 'NONE',  ( -100.7167115039422214, -272.8831171082964602, -234.0295411440080500 ) ) ;
#40712 = CARTESIAN_POINT ( 'NONE',  ( -71.19072634182349191, -287.5168853751376332, -337.6860779236608323 ) ) ;
#40714 = CARTESIAN_POINT ( 'NONE',  ( 20.28674988660977263, -286.8596702667462068, -219.2142027799276889 ) ) ;
#40715 = AXIS2_PLACEMENT_3D ( 'NONE', #59394, #8709, #45610 ) ;
#40716 = CARTESIAN_POINT ( 'NONE',  ( -26.15182502095681727, -288.5801221705755779, -346.5223350588607900 ) ) ;
#40717 = CARTESIAN_POINT ( 'NONE',  ( -112.3043731446424545, -298.4338816474951841, -278.0425537548256330 ) ) ;
#40718 = CARTESIAN_POINT ( 'NONE',  ( -34.25032877576914103, -293.0130252935406361, -345.1305759983741837 ) ) ;
#40719 = ADVANCED_FACE ( 'NONE', ( #64436 ), #24675, .T. ) ;
#40720 = CARTESIAN_POINT ( 'NONE',  ( 19.65684331992298794, -281.4512309075841472, -321.9687939641002572 ) ) ;
#40721 = EDGE_CURVE ( 'NONE', #53411, #14181, #41284, .T. ) ;
#40722 = CARTESIAN_POINT ( 'NONE',  ( 156.1760182705776288, 20.00000000000000000, 14.66829968254666738 ) ) ;
#40723 = CARTESIAN_POINT ( 'NONE',  ( -112.3830721958973413, -276.5362639220081746, -271.5856794472763909 ) ) ;
#40724 = CARTESIAN_POINT ( 'NONE',  ( 202.1676623822758359, 287.7243935111420683, -5.007149546673600682 ) ) ;
#40725 = CARTESIAN_POINT ( 'NONE',  ( -48.13445022982620713, -287.9873033114513419, -343.0116405947665612 ) ) ;
#40726 = DIRECTION ( 'NONE',  ( 1.000000000000000000, -0.000000000000000000, -0.000000000000000000 ) ) ;
#40727 = CARTESIAN_POINT ( 'NONE',  ( -95.67549732217206326, -287.9030632420486882, -317.5010029872674409 ) ) ;
#40728 = CARTESIAN_POINT ( 'NONE',  ( -80.20910950928154648, -299.0608441273629978, -210.2876161177727568 ) ) ;
#40729 = CARTESIAN_POINT ( 'NONE',  ( 34.76556382236587694, -282.6542875849948473, -244.9218044263096488 ) ) ;
#40731 = CARTESIAN_POINT ( 'NONE',  ( -95.92174313203582869, -283.9411625859445962, -313.9200270788040257 ) ) ;
#40730 = CARTESIAN_POINT ( 'NONE',  ( -43.13754190542001510, -295.9995636395456131, -195.1770607610970103 ) ) ;
#40732 = CARTESIAN_POINT ( 'NONE',  ( -31.30935756776330336, -275.5550739934492412, -197.0067972287041869 ) ) ;
#40733 = CARTESIAN_POINT ( 'NONE',  ( 36.02281967335061807, -283.3515133523521285, -254.7226156802384480 ) ) ;
#40734 = CARTESIAN_POINT ( 'NONE',  ( -60.57923519024238601, -296.8020830102483956, -200.8565948379476822 ) ) ;
#40735 = ORIENTED_EDGE ( 'NONE', *, *, #59920, .F. ) ;
#40736 = CARTESIAN_POINT ( 'NONE',  ( 204.8722290845309431, 293.3206796832986925, -54.00000000000338929 ) ) ;
#40737 = CARTESIAN_POINT ( 'NONE',  ( -8.390006710344874108, -294.5169032120475094, -341.7674372384428807 ) ) ;
#40738 = CARTESIAN_POINT ( 'NONE',  ( -96.27075699170869427, -287.1635492943576082, -224.5231848368011924 ) ) ;
#40739 = DIRECTION ( 'NONE',  ( 0.2456588035076220367, -0.9693563597868450898, 0.000000000000000000 ) ) ;
#40740 = CARTESIAN_POINT ( 'NONE',  ( -115.3288506153726871, -282.2666405000203440, -252.5284128619063608 ) ) ;
#40741 = CARTESIAN_POINT ( 'NONE',  ( -108.5107275564088098, -277.3806568782591171, -299.3288302666456957 ) ) ;
#40742 = CARTESIAN_POINT ( 'NONE',  ( -107.0083240628469525, -288.5524772779304499, -301.3617035926965855 ) ) ;
#40743 = CARTESIAN_POINT ( 'NONE',  ( -103.6279268527864588, -285.6390550488317217, -302.6783089496187813 ) ) ;
#40744 = CARTESIAN_POINT ( 'NONE',  ( -59.47699923191905214, -279.1028905083606446, -340.9869103347682540 ) ) ;
#40745 = CARTESIAN_POINT ( 'NONE',  ( -113.7516335173012436, -285.9819387223919875, -270.0028293630546727 ) ) ;
#40746 = CARTESIAN_POINT ( 'NONE',  ( -34.84834122616985042, -281.8150925183938966, -343.7283336771308200 ) ) ;
#40747 = CARTESIAN_POINT ( 'NONE',  ( -46.73143214481503804, -281.9332393483321084, -195.8987116322781503 ) ) ;
#40748 = CARTESIAN_POINT ( 'NONE',  ( -31.26218179661070806, -274.2935900508747977, -193.5882153225365698 ) ) ;
#40749 = CARTESIAN_POINT ( 'NONE',  ( -25.77206355675157923, -276.7419733318878912, -346.4869579719969011 ) ) ;
#40750 = CARTESIAN_POINT ( 'NONE',  ( -97.55916704965966346, -297.8714093582178748, -314.1455308458188824 ) ) ;
#40751 = DIRECTION ( 'NONE',  ( 1.000000000000000000, 0.000000000000000000, -0.000000000000000000 ) ) ;
#40752 = FACE_BOUND ( 'NONE', #56347, .T. ) ;
#40753 = CARTESIAN_POINT ( 'NONE',  ( -110.4072122214023040, -294.4365812169259584, -290.4044815935360475 ) ) ;
#40754 = CARTESIAN_POINT ( 'NONE',  ( 34.76685974822430580, -275.2188592174068731, -282.4286251204140399 ) ) ;
#40755 = CARTESIAN_POINT ( 'NONE',  ( -82.79846264992411875, -298.5267956779829319, -208.5280224608817150 ) ) ;
#40756 = CARTESIAN_POINT ( 'NONE',  ( -1.718066948587068987, -288.2907742959700386, -205.4273493023209767 ) ) ;
#40757 = CARTESIAN_POINT ( 'NONE',  ( 30.29679852815585406, -295.5321171716436197, -305.6844990564229647 ) ) ;
#40758 = CARTESIAN_POINT ( 'NONE',  ( 38.84386646662502329, -294.8637600141316284, -278.8356150261316202 ) ) ;
#40759 = CARTESIAN_POINT ( 'NONE',  ( -107.4366345674533676, -292.8950539676741300, -244.0084363771255767 ) ) ;
#40760 = CARTESIAN_POINT ( 'NONE',  ( -69.28327963476367302, -277.6307593934475904, -202.6871648721881058 ) ) ;
#40761 = CARTESIAN_POINT ( 'NONE',  ( -94.20572702861829839, -281.1419522914044364, -222.3019699944966021 ) ) ;
#40762 = CARTESIAN_POINT ( 'NONE',  ( -97.58796398658721216, -294.0317217691893461, -314.1058973431291861 ) ) ;
#40763 = CARTESIAN_POINT ( 'NONE',  ( -97.05603242901973715, -285.7792979252941450, -316.9926952909643205 ) ) ;
#40764 = CARTESIAN_POINT ( 'NONE',  ( -14.45651033147271391, -285.2761118086507395, -200.6623818813432081 ) ) ;
#40765 = CARTESIAN_POINT ( 'NONE',  ( 155.5252760472149873, 205.5130994547002388, -216.6222576925314343 ) ) ;
#40766 = EDGE_LOOP ( 'NONE', ( #48982, #2246, #36979, #28598 ) ) ;
#40767 = CARTESIAN_POINT ( 'NONE',  ( -98.12231486432158079, -284.7805100993483052, -229.8913223435700672 ) ) ;
#40768 = ORIENTED_EDGE ( 'NONE', *, *, #86200, .F. ) ;
#40769 = CARTESIAN_POINT ( 'NONE',  ( 28.04866328337839576, -283.1585939237264711, -310.5316349792955180 ) ) ;
#40770 = CARTESIAN_POINT ( 'NONE',  ( -71.92148776104070862, -273.9153231682902856, -205.9905027090790668 ) ) ;
#40771 = CARTESIAN_POINT ( 'NONE',  ( 24.39242218744337976, -285.7415533311229296, -225.0079829049096816 ) ) ;
#40772 = CARTESIAN_POINT ( 'NONE',  ( -39.59240733921521382, -280.9658174499913912, -193.6164024688690972 ) ) ;
#40773 = DIRECTION ( 'NONE',  ( 0.000000000000000000, 0.000000000000000000, 1.000000000000000000 ) ) ;
#40774 = CARTESIAN_POINT ( 'NONE',  ( -79.54359671755467787, -281.0137518218346031, -206.7232973948598556 ) ) ;
#40775 = CARTESIAN_POINT ( 'NONE',  ( 20.04707733962005278, -281.5085053594997930, -219.1569386987120538 ) ) ;
#40776 = CARTESIAN_POINT ( 'NONE',  ( 17.40634833298269157, -284.4094976428775112, -226.7417163044926838 ) ) ;
#40777 = ORIENTED_EDGE ( 'NONE', *, *, #69768, .T. ) ;
#40778 = CARTESIAN_POINT ( 'NONE',  ( -70.32131025625263021, -275.6166088378918744, -203.1869135081190620 ) ) ;
#40779 = CARTESIAN_POINT ( 'NONE',  ( -114.2130631985986611, -273.1142508670334337, -284.1207669014788166 ) ) ;
#40780 = AXIS2_PLACEMENT_3D ( 'NONE', #65321, #13710, #6610 ) ;
#40781 = CARTESIAN_POINT ( 'NONE',  ( -27.31297884136561294, -278.2001842557492068, -196.3407276125316230 ) ) ;
#40782 = CARTESIAN_POINT ( 'NONE',  ( 37.32528725606848496, -295.1335947456945519, -256.2609403032764703 ) ) ;
#40783 = CARTESIAN_POINT ( 'NONE',  ( -72.18045306765381497, -294.8744456583661986, -334.6416815503314979 ) ) ;
#40784 = CARTESIAN_POINT ( 'NONE',  ( -97.41158513264095120, -290.7042885283434543, -222.2868439980655921 ) ) ;
#40785 = CARTESIAN_POINT ( 'NONE',  ( 115.2448031289451222, -299.5541904835127980, -195.3611179825600175 ) ) ;
#40787 = CARTESIAN_POINT ( 'NONE',  ( 35.74988827704921590, -286.0863260417717129, -280.6539328188176228 ) ) ;
#40786 = CARTESIAN_POINT ( 'NONE',  ( -79.16970383640156683, -294.1794160040460611, -334.3065978670253457 ) ) ;
#40788 = CARTESIAN_POINT ( 'NONE',  ( 21.96659234642915237, -294.7959920027644216, -225.7137000664298796 ) ) ;
#40789 = CARTESIAN_POINT ( 'NONE',  ( 35.94225504082317713, -286.3179257838690432, -276.5393517682699098 ) ) ;
#40790 = CARTESIAN_POINT ( 'NONE',  ( -110.4869636751025865, -285.9675168945678365, -262.7152819765586287 ) ) ;
#40791 = ORIENTED_EDGE ( 'NONE', *, *, #29697, .F. ) ;
#40792 = CARTESIAN_POINT ( 'NONE',  ( -30.72952027957549959, -293.0749191594383660, -193.8291165596032783 ) ) ;
#40793 = CARTESIAN_POINT ( 'NONE',  ( -42.93137296007004267, -283.6168105322291240, -343.2586489960274889 ) ) ;
#40794 = CARTESIAN_POINT ( 'NONE',  ( -113.9120860140077696, -295.3926165118751328, -266.7386726728709050 ) ) ;
#40795 = CARTESIAN_POINT ( 'NONE',  ( -80.44156562110758557, -290.4225811138954896, -334.0379702815916971 ) ) ;
#40796 = CARTESIAN_POINT ( 'NONE',  ( -16.64919588928149352, -292.8048955457495595, -196.2574934328994516 ) ) ;
#40797 = CARTESIAN_POINT ( 'NONE',  ( 32.27295258127616506, -287.4270622252837484, -248.3465597118683377 ) ) ;
#40798 = ORIENTED_EDGE ( 'NONE', *, *, #13973, .T. ) ;
#40799 = CARTESIAN_POINT ( 'NONE',  ( 164.2231345125756263, 296.7472757692770529, -7.499999999999996447 ) ) ;
#40800 = CARTESIAN_POINT ( 'NONE',  ( -102.0481672979126273, -297.8894987306101143, -309.7740420733584301 ) ) ;
#40801 = CARTESIAN_POINT ( 'NONE',  ( -75.51919720547898862, -296.2392189133624925, -203.9996681549014284 ) ) ;
#40802 = CARTESIAN_POINT ( 'NONE',  ( 32.20381646552353061, -280.3052812333497172, -247.2484346923745591 ) ) ;
#40803 = EDGE_LOOP ( 'NONE', ( #39713, #46805, #79734, #85419 ) ) ;
#40804 = CARTESIAN_POINT ( 'NONE',  ( 34.66636598366659427, -274.7166918549107777, -243.2619423870185926 ) ) ;
#40805 = CARTESIAN_POINT ( 'NONE',  ( -110.7919826542591863, -294.9460210298589118, -276.9424819505929349 ) ) ;
#40806 = CARTESIAN_POINT ( 'NONE',  ( -36.42758969182520445, -278.9010281178919968, -344.6033714018661271 ) ) ;
#40807 = CARTESIAN_POINT ( 'NONE',  ( -31.21453646993573727, -272.2699158702042155, -196.3663419807342336 ) ) ;
#40808 = CARTESIAN_POINT ( 'NONE',  ( -72.30025978504744444, -296.7306346518647047, -334.9125038239262722 ) ) ;
#40809 = CARTESIAN_POINT ( 'NONE',  ( -109.3518920008327626, -297.8131810571256324, -256.5552608076564525 ) ) ;
#40810 = CARTESIAN_POINT ( 'NONE',  ( 175.2296996224749250, 215.0000000000000568, -24.99999999999999289 ) ) ;
#40811 = CARTESIAN_POINT ( 'NONE',  ( -113.1452920391883197, -298.0541790381083160, -278.1235832924380702 ) ) ;
#40812 = CARTESIAN_POINT ( 'NONE',  ( -43.12272060284060871, -295.9792986173570739, -195.3651410756511666 ) ) ;
#40813 = CARTESIAN_POINT ( 'NONE',  ( -67.85128520249233475, -292.2922183153227138, -203.9165132173930886 ) ) ;
#40814 = CARTESIAN_POINT ( 'NONE',  ( -100.8213516803394896, -288.6186554914600606, -307.6866326828009051 ) ) ;
#40815 = CARTESIAN_POINT ( 'NONE',  ( 208.8036087770903748, 29.39224792112960927, 14.71645718445160966 ) ) ;
#40816 = CARTESIAN_POINT ( 'NONE',  ( -27.01099509605257509, -274.6723510927560596, -194.0659876162978321 ) ) ;
#40817 = CARTESIAN_POINT ( 'NONE',  ( -91.86350586436429921, -297.5798225096255578, -221.7868430412704015 ) ) ;
#40818 = CARTESIAN_POINT ( 'NONE',  ( -20.15636797866193675, -282.2516531660892269, -196.9381063469822948 ) ) ;
#40819 = CARTESIAN_POINT ( 'NONE',  ( -34.51407401549179355, -281.7021378490764505, -346.8156979919957053 ) ) ;
#40820 = CARTESIAN_POINT ( 'NONE',  ( -80.17629944680187748, -276.9638439778925090, -334.2884352067326859 ) ) ;
#40821 = CARTESIAN_POINT ( 'NONE',  ( -29.43734602465698558, -282.1467764117663819, -343.1449642762883059 ) ) ;
#40822 = CARTESIAN_POINT ( 'NONE',  ( 24.40931763100144281, -280.1322721915568081, -313.2421186560339379 ) ) ;
#40823 = CARTESIAN_POINT ( 'NONE',  ( -94.22234407881526863, -271.7832063693932128, -223.6513004685467934 ) ) ;
#40824 = CARTESIAN_POINT ( 'NONE',  ( -103.3349993597024081, -280.0779075713660404, -306.1041723858960495 ) ) ;
#40825 = CARTESIAN_POINT ( 'NONE',  ( 187.8995604928813918, 43.86402690510830382, 12.00000000000000000 ) ) ;
#40826 = DIRECTION ( 'NONE',  ( -0.2456588035076248677, 0.9693563597868444237, 0.000000000000000000 ) ) ;
#40827 = CARTESIAN_POINT ( 'NONE',  ( -57.10427690919379273, -296.0406156110562392, -196.9348153049176631 ) ) ;
#40828 = CARTESIAN_POINT ( 'NONE',  ( -39.87502861699211110, -279.0840375963972519, -345.4978420900201286 ) ) ;
#40829 = CARTESIAN_POINT ( 'NONE',  ( 27.00448396442096310, -273.0349971886321896, -231.7303622426582024 ) ) ;
#40830 = ADVANCED_FACE ( 'NONE', ( #72435 ), #14221, .F. ) ;
#40831 = CARTESIAN_POINT ( 'NONE',  ( -83.63170945779074827, -373.0521521680024648, -525.1711561948568487 ) ) ;
#40832 = CARTESIAN_POINT ( 'NONE',  ( -110.0981731642692978, -286.2119089200976987, -290.7525336038329442 ) ) ;
#40833 = ORIENTED_EDGE ( 'NONE', *, *, #17917, .F. ) ;
#40834 = CARTESIAN_POINT ( 'NONE',  ( -83.63170945779077670, -373.0521521680024648, -417.1172536214571096 ) ) ;
#40835 = CARTESIAN_POINT ( 'NONE',  ( 29.40140730054798723, -286.0057912162362186, -304.6840805177163247 ) ) ;
#40836 = CARTESIAN_POINT ( 'NONE',  ( 154.7659666677267865, 20.47222690886501439, 12.53936336329526391 ) ) ;
#40837 = CARTESIAN_POINT ( 'NONE',  ( 14.58641805611695474, -293.0964505981641537, -322.3035668874909447 ) ) ;
#40838 = CARTESIAN_POINT ( 'NONE',  ( 36.22344169838126504, -285.5577553103556738, -260.0331182147264144 ) ) ;
#40839 = CARTESIAN_POINT ( 'NONE',  ( -114.4693268140674434, -273.6886850827510216, -284.2063049943780015 ) ) ;
#40840 = CARTESIAN_POINT ( 'NONE',  ( -91.87860149268118448, -293.8295572229975505, -321.9211512346975610 ) ) ;
#40841 = CARTESIAN_POINT ( 'NONE',  ( -100.4124057866275876, -283.6046788040872570, -227.3167484595732617 ) ) ;
#40842 = CARTESIAN_POINT ( 'NONE',  ( 24.34008617122410101, -282.5954890819425600, -229.7498932956006001 ) ) ;
#40843 = CARTESIAN_POINT ( 'NONE',  ( 39.30540471429771543, -288.7719187111901533, -271.5298351959435763 ) ) ;
#40844 = CARTESIAN_POINT ( 'NONE',  ( 7.960616284745397842, -278.9011784544928219, -209.2901720496602991 ) ) ;
#40845 = CARTESIAN_POINT ( 'NONE',  ( -84.68502914533901560, -289.7257183005926322, -325.9940982908404976 ) ) ;
#40846 = CARTESIAN_POINT ( 'NONE',  ( -32.94580629236323688, -281.5338940558859804, -196.9032999153979802 ) ) ;
#40847 = CARTESIAN_POINT ( 'NONE',  ( -30.25690234391162292, -280.9467639918202053, -197.4930206804950501 ) ) ;
#40848 = CARTESIAN_POINT ( 'NONE',  ( 36.22481430127140101, -289.7413652231179526, -286.7411050212907071 ) ) ;
#40849 = CIRCLE ( 'NONE', #21218, 0.5000000000000004441 ) ;
#40850 = EDGE_LOOP ( 'NONE', ( #90964, #79228, #20707, #15453 ) ) ;
#40851 = CARTESIAN_POINT ( 'NONE',  ( -114.1810291951405389, -272.6238746950663199, -264.6262428901742965 ) ) ;
#40853 = CARTESIAN_POINT ( 'NONE',  ( -101.1299814222145983, -293.0541704589147116, -231.5938383425343545 ) ) ;
#40852 = AXIS2_PLACEMENT_3D ( 'NONE', #90572, #40385, #62207 ) ;
#40854 = DIRECTION ( 'NONE',  ( 0.9693563597868444237, 0.2456588035076248677, -0.000000000000000000 ) ) ;
#40855 = CARTESIAN_POINT ( 'NONE',  ( -55.63300648810263738, -300.3376638359844719, -190.3683826091709363 ) ) ;
#40856 = ORIENTED_EDGE ( 'NONE', *, *, #38609, .T. ) ;
#40857 = CARTESIAN_POINT ( 'NONE',  ( 33.99823975984501345, -273.2447717856712757, -246.5190087516483857 ) ) ;
#40858 = LINE ( 'NONE', #75475, #59487 ) ;
#40859 = CARTESIAN_POINT ( 'NONE',  ( -97.65388681535674209, -294.3239000025851624, -316.9323597000637278 ) ) ;
#40860 = CARTESIAN_POINT ( 'NONE',  ( -101.2653793693434920, -296.5429530137053007, -234.9810151879597129 ) ) ;
#40861 = CARTESIAN_POINT ( 'NONE',  ( -26.35256064096607531, -290.4300345296048249, -343.2820336454902872 ) ) ;
#40862 = CARTESIAN_POINT ( 'NONE',  ( -18.45572455530352940, -284.5657957651918082, -341.9774706403745199 ) ) ;
#40863 = CARTESIAN_POINT ( 'NONE',  ( -101.7944090981691119, -291.4341600051653813, -311.5005594390137844 ) ) ;
#40864 = CARTESIAN_POINT ( 'NONE',  ( -62.58503126303945407, -290.6889382953436325, -342.6395187608372339 ) ) ;
#40865 = CARTESIAN_POINT ( 'NONE',  ( -7.481455919679338429, -288.4438165826724116, -201.5616523811309264 ) ) ;
#40866 = CARTESIAN_POINT ( 'NONE',  ( -100.2502106458468347, -279.3063546934228611, -225.9593239990914242 ) ) ;
#40867 = CARTESIAN_POINT ( 'NONE',  ( -108.0978744198313137, -294.2885667870677935, -297.0207124331947171 ) ) ;
#40868 = CARTESIAN_POINT ( 'NONE',  ( -50.09559852093136101, -283.0437884431527777, -346.3514014124780260 ) ) ;
#40869 = CARTESIAN_POINT ( 'NONE',  ( 36.24179311842240025, -277.2852502986532954, -260.5460784150674272 ) ) ;
#40870 = CARTESIAN_POINT ( 'NONE',  ( 99.44099354567467230, -302.2645883696979467, -195.3030568020281521 ) ) ;
#40871 = CARTESIAN_POINT ( 'NONE',  ( 5.284070706827503017, -274.7238545970356540, -333.2659482633400785 ) ) ;
#40872 = LINE ( 'NONE', #76895, #33371 ) ;
#40873 = CARTESIAN_POINT ( 'NONE',  ( -6.737924298192999650, -279.9727170801672855, -204.0044325830203320 ) ) ;
#40874 = CARTESIAN_POINT ( 'NONE',  ( -93.03470374325408443, -279.0346222545300634, -323.0328254285655589 ) ) ;
#40875 = CARTESIAN_POINT ( 'NONE',  ( -26.64200715918355655, -285.2437042387158499, -194.2924098185255275 ) ) ;
#40876 = CARTESIAN_POINT ( 'NONE',  ( -1.974665632540484772, -294.2873757498284704, -205.3302152267432632 ) ) ;
#40877 = CARTESIAN_POINT ( 'NONE',  ( 21.22280191546856898, -276.4896502891693899, -221.6103280585869015 ) ) ;
#40878 = CARTESIAN_POINT ( 'NONE',  ( -32.72917726941999206, -275.4242773834973264, -193.9803691665565566 ) ) ;
#40879 = DIRECTION ( 'NONE',  ( 1.000000000000000000, 0.000000000000000000, 0.000000000000000000 ) ) ;
#40880 = CARTESIAN_POINT ( 'NONE',  ( -16.38289931662955823, -276.6070554962078631, -340.3407213445818229 ) ) ;
#40881 = CARTESIAN_POINT ( 'NONE',  ( -95.34786471575526434, -297.8992183611205178, -317.6603497505437304 ) ) ;
#40882 = CARTESIAN_POINT ( 'NONE',  ( -46.93527959788583104, -283.9300092129055315, -196.0932234165706802 ) ) ;
#40883 = CARTESIAN_POINT ( 'NONE',  ( -27.84748908710411186, -291.8361515741199241, -193.9163312745061205 ) ) ;
#40884 = CARTESIAN_POINT ( 'NONE',  ( 36.65426344356991706, -273.4455615773345016, -260.5405183295529241 ) ) ;
#40885 = CARTESIAN_POINT ( 'NONE',  ( 9.749716255935902964, -290.0166980007785469, -330.3351778715236833 ) ) ;
#40886 = CARTESIAN_POINT ( 'NONE',  ( -34.83299178285379583, -291.0047313505910438, -197.0949425890030113 ) ) ;
#40887 = EDGE_LOOP ( 'NONE', ( #55953, #30515, #41522 ) ) ;
#40888 = CARTESIAN_POINT ( 'NONE',  ( -19.50655331740970055, -290.8517849429848638, -196.0065514991878786 ) ) ;
#40889 = CARTESIAN_POINT ( 'NONE',  ( -109.9934992487361285, -290.3156030965975560, -263.0260262131951094 ) ) ;
#40890 = VERTEX_POINT ( 'NONE', #35038 ) ;
#40891 = CARTESIAN_POINT ( 'NONE',  ( 25.28470490797628401, -288.0434057776815280, -226.0730789246693178 ) ) ;
#40892 = CARTESIAN_POINT ( 'NONE',  ( -108.7845816817346787, -278.6863013625263079, -285.4608584497309494 ) ) ;
#40893 = CARTESIAN_POINT ( 'NONE',  ( -64.17097843709920824, -294.3144674217803640, -342.2059670324316585 ) ) ;
#40894 = CARTESIAN_POINT ( 'NONE',  ( -91.83661099625958002, -285.9507757439558304, -216.1060032382476379 ) ) ;
#40895 = CARTESIAN_POINT ( 'NONE',  ( -0.9832920331938328484, -286.8546714922085243, -202.5097329386007630 ) ) ;
#40896 = CARTESIAN_POINT ( 'NONE',  ( 11.93408240144392529, -282.6776104189459602, -324.2497507617106294 ) ) ;
#40897 = CARTESIAN_POINT ( 'NONE',  ( 153.7078430325209126, 207.1860052592516013, -217.3454689461144653 ) ) ;
#40898 = CARTESIAN_POINT ( 'NONE',  ( 183.8342670656734015, 263.4819769339147797, -152.6844725691555595 ) ) ;
#40899 = CARTESIAN_POINT ( 'NONE',  ( 183.6787524270977485, 261.1293638455505857, -151.0742354505036360 ) ) ;
#40900 = CARTESIAN_POINT ( 'NONE',  ( 0.7051506998533149106, -273.7708687721664091, -207.8708077817659614 ) ) ;
#40901 = CARTESIAN_POINT ( 'NONE',  ( 32.38797661390856319, -274.7714208734319072, -292.9884964230134869 ) ) ;
#40902 = CARTESIAN_POINT ( 'NONE',  ( -107.7142036935486402, -296.4584093970260597, -239.1289756098501016 ) ) ;
#40903 = CARTESIAN_POINT ( 'NONE',  ( 66.18494971993401066, 45.90398865963478414, -315.9893126914129766 ) ) ;
#40904 = CARTESIAN_POINT ( 'NONE',  ( 39.06291576992948222, -274.1756417347864954, -265.4879876495817257 ) ) ;
#40905 = CARTESIAN_POINT ( 'NONE',  ( -54.46746588770982100, -275.5892481486159795, -198.3563809298433682 ) ) ;
#40906 = ORIENTED_EDGE ( 'NONE', *, *, #34635, .F. ) ;
#40907 = CARTESIAN_POINT ( 'NONE',  ( -34.07149460053084056, -299.0334027112224362, -193.5959021688697135 ) ) ;
#40908 = CARTESIAN_POINT ( 'NONE',  ( -21.10957504857951506, -289.3305628936617495, -341.5966888503347150 ) ) ;
#40909 = CARTESIAN_POINT ( 'NONE',  ( -96.38077122379498007, -296.6918863268394944, -319.5602973641422295 ) ) ;
#40910 = CARTESIAN_POINT ( 'NONE',  ( -108.8337426737351450, -297.4070671079502404, -241.7852827642537079 ) ) ;
#40911 = CARTESIAN_POINT ( 'NONE',  ( 34.71360014120221393, -293.5633785683979795, -258.5768258089188976 ) ) ;
#40912 = ORIENTED_EDGE ( 'NONE', *, *, #71404, .T. ) ;
#40913 = CARTESIAN_POINT ( 'NONE',  ( 26.44655563262336884, -278.0143258023581438, -310.9599378445709590 ) ) ;
#40914 = ORIENTED_EDGE ( 'NONE', *, *, #41255, .T. ) ;
#40915 = CARTESIAN_POINT ( 'NONE',  ( 36.92725390009606912, -280.8074373718260972, -250.2201139663033302 ) ) ;
#40916 = CARTESIAN_POINT ( 'NONE',  ( -37.79923683419279001, -277.9992392846198754, -343.6074770607820597 ) ) ;
#40917 = CARTESIAN_POINT ( 'NONE',  ( 20.96763879468937830, -277.9766797861123564, -319.0847776445557997 ) ) ;
#40918 = CIRCLE ( 'NONE', #56109, 7.999911143031724237 ) ;
#40919 = CARTESIAN_POINT ( 'NONE',  ( -98.33364197106298832, -275.9720951254918759, -314.6367673584895783 ) ) ;
#40920 = CARTESIAN_POINT ( 'NONE',  ( -104.8595255667243720, -297.5788169953463012, -242.3390567462739966 ) ) ;
#40921 = CARTESIAN_POINT ( 'NONE',  ( -109.8533898197255212, -295.2910675836055816, -257.8140156865094355 ) ) ;
#40922 = CARTESIAN_POINT ( 'NONE',  ( 153.6987871352711466, 19.48326534539917887, -11.45812909362559928 ) ) ;
#40923 = CARTESIAN_POINT ( 'NONE',  ( 19.11074369088685287, -281.3318379090331973, -218.0863775229832697 ) ) ;
#40924 = CARTESIAN_POINT ( 'NONE',  ( -109.9663383702328900, -278.8227569530467349, -262.4831275639624550 ) ) ;
#40925 = CARTESIAN_POINT ( 'NONE',  ( -4.559655801269173914, -287.3140747464676679, -339.5031807684796945 ) ) ;
#40926 = CARTESIAN_POINT ( 'NONE',  ( 72.99834851041279649, -301.4305609889117932, -195.1569263972049271 ) ) ;
#40927 = DIRECTION ( 'NONE',  ( 0.000000000000000000, 0.000000000000000000, 1.000000000000000000 ) ) ;
#40928 = CARTESIAN_POINT ( 'NONE',  ( -31.86945840514198736, -288.1786415660986904, -343.3683901364825601 ) ) ;
#40929 = EDGE_CURVE ( 'NONE', #35152, #81908, #51903, .T. ) ;
#40930 = CARTESIAN_POINT ( 'NONE',  ( -41.08026103079195934, -278.2443110747364017, -196.4422626262946494 ) ) ;
#40932 = CARTESIAN_POINT ( 'NONE',  ( -13.08274929604248982, -280.8144953876131922, -340.7920297080265186 ) ) ;
#40931 = CARTESIAN_POINT ( 'NONE',  ( -57.25536489884444080, -278.3648203012128874, -199.5174812106892546 ) ) ;
#40933 = CARTESIAN_POINT ( 'NONE',  ( -95.42566117404476245, -287.2063707370795100, -222.8938104063183516 ) ) ;
#40934 = CARTESIAN_POINT ( 'NONE',  ( -100.9191528787679175, -279.2558515195320865, -307.1379167346669874 ) ) ;
#40935 = CARTESIAN_POINT ( 'NONE',  ( 152.4536156746142410, 276.0000000000000568, 14.50000000000000000 ) ) ;
#40936 = CARTESIAN_POINT ( 'NONE',  ( -61.08034301192003568, -293.7442956298834247, -199.1623514990029662 ) ) ;
#40937 = CARTESIAN_POINT ( 'NONE',  ( -110.8529042008521373, -276.5474198098099805, -289.6496863254466234 ) ) ;
#40938 = CARTESIAN_POINT ( 'NONE',  ( -6.225714457559289983, -277.2836039704966424, -336.5238907322673185 ) ) ;
#40939 = CARTESIAN_POINT ( 'NONE',  ( -38.67389111183416617, -285.0689823418150013, -345.5159827458489872 ) ) ;
#40940 = CARTESIAN_POINT ( 'NONE',  ( 115.2940338803257703, -299.5541904835127980, -197.7520877843884080 ) ) ;
#40941 = CARTESIAN_POINT ( 'NONE',  ( -81.98185092125250151, -291.5755395712980089, -331.3248049816650678 ) ) ;
#40942 = CARTESIAN_POINT ( 'NONE',  ( -25.84630414365701867, -292.9057046909653650, -344.5266118690907433 ) ) ;
#40943 = CARTESIAN_POINT ( 'NONE',  ( 34.91711868069736369, -287.0817747895744674, -296.6467246737050800 ) ) ;
#40944 = CARTESIAN_POINT ( 'NONE',  ( -32.64288430324890555, -272.7974008908149699, -197.0057187629735722 ) ) ;
#40945 = CARTESIAN_POINT ( 'NONE',  ( -6.269110277569869716, -292.7790882332398041, -337.7804004123926802 ) ) ;
#40946 =( NAMED_UNIT ( * ) PLANE_ANGLE_UNIT ( ) SI_UNIT ( $, .RADIAN. ) );
#40947 = CARTESIAN_POINT ( 'NONE',  ( -110.5613795317854198, -289.3039673646861161, -248.8765583812391640 ) ) ;
#40948 = CARTESIAN_POINT ( 'NONE',  ( -67.89732362602889282, -287.2443398007634414, -203.1837833389752461 ) ) ;
#40949 = CARTESIAN_POINT ( 'NONE',  ( 23.06963481109530534, -285.1691033680874625, -224.2480786117171192 ) ) ;
#40950 = ADVANCED_FACE ( 'NONE', ( #71035 ), #13181, .F. ) ;
#40951 = CARTESIAN_POINT ( 'NONE',  ( -67.80807798851924417, -287.0695119959246995, -203.3747407199194868 ) ) ;
#40952 = DIRECTION ( 'NONE',  ( 0.000000000000000000, 0.000000000000000000, 1.000000000000000000 ) ) ;
#40953 = CARTESIAN_POINT ( 'NONE',  ( -99.75239657253662529, -285.8810234999037903, -232.0872675049267855 ) ) ;
#40954 = CARTESIAN_POINT ( 'NONE',  ( 35.81886551686887543, -295.3012588055818242, -252.3073526920058782 ) ) ;
#40955 = CARTESIAN_POINT ( 'NONE',  ( 20.61017094222211909, -274.2969797833857797, -318.8471452555712631 ) ) ;
#40956 = CARTESIAN_POINT ( 'NONE',  ( -7.888799347717783128, -277.0099541260258320, -341.4969213389408083 ) ) ;
#40957 = CARTESIAN_POINT ( 'NONE',  ( -55.81265611667642190, -289.8961427098901140, -197.0396244884203725 ) ) ;
#40958 = CARTESIAN_POINT ( 'NONE',  ( -112.4017312731608058, -278.7669533499513932, -253.1857948560594025 ) ) ;
#40959 = CARTESIAN_POINT ( 'NONE',  ( -45.24026552476296104, -297.1324474610444213, -344.6384646975732835 ) ) ;
#40960 = CARTESIAN_POINT ( 'NONE',  ( 164.6329196456214277, 275.0000000000000568, 23.09031830825856701 ) ) ;
#40961 = CARTESIAN_POINT ( 'NONE',  ( 208.3303265509962330, 36.67066202700165434, 13.52119360038354401 ) ) ;
#40962 = CARTESIAN_POINT ( 'NONE',  ( 19.90984047221398967, -285.5896422434225315, -224.2596743818670575 ) ) ;
#40963 = CARTESIAN_POINT ( 'NONE',  ( 20.95224922324841188, -280.2018833336271086, -317.5705241888700243 ) ) ;
#40964 = CARTESIAN_POINT ( 'NONE',  ( 183.0442525570908288, 300.2961574867697436, -7.500000000000000000 ) ) ;
#40965 = CARTESIAN_POINT ( 'NONE',  ( -7.939669693597882549, -272.9101739149491550, -199.8903344400839899 ) ) ;
#40966 = CARTESIAN_POINT ( 'NONE',  ( -87.17106446520546115, -277.1174833406175253, -323.8487531678294431 ) ) ;
#40967 = CARTESIAN_POINT ( 'NONE',  ( -8.946001522705490316, -296.1940125716217835, -338.3777375388956443 ) ) ;
#40968 = CARTESIAN_POINT ( 'NONE',  ( -2.518167510610716420, -279.4221533293300013, -202.0177275191922774 ) ) ;
#40969 = CARTESIAN_POINT ( 'NONE',  ( -69.81766495532748706, -296.4319807206471182, -336.0019601270143994 ) ) ;
#40970 = EDGE_CURVE ( 'NONE', #92001, #49115, #93363, .T. ) ;
#40971 = CARTESIAN_POINT ( 'NONE',  ( -106.7121327851724573, -297.4517027104175781, -302.6262902956850667 ) ) ;
#40972 = CARTESIAN_POINT ( 'NONE',  ( -106.3249697826862672, -272.5372377173292193, -246.4154295500165688 ) ) ;
#40973 = CARTESIAN_POINT ( 'NONE',  ( -27.87857319862299477, -294.1723383268938505, -195.9083763871365989 ) ) ;
#40974 = CARTESIAN_POINT ( 'NONE',  ( -36.56756391987610755, -286.2282954959094354, -193.3519706163582441 ) ) ;
#40975 = CARTESIAN_POINT ( 'NONE',  ( 38.14775023160404288, -273.7737627613824429, -276.8146722799290274 ) ) ;
#40976 = CARTESIAN_POINT ( 'NONE',  ( 36.38478081270785935, -287.6647871430372447, -292.6196524667047356 ) ) ;
#40977 = CARTESIAN_POINT ( 'NONE',  ( -111.8011020342518833, -280.5998799454968093, -265.1033363045849569 ) ) ;
#40978 = CARTESIAN_POINT ( 'NONE',  ( 26.57858354566873871, -286.1223175304125448, -234.5137189545126262 ) ) ;
#40979 = CARTESIAN_POINT ( 'NONE',  ( -107.5913298006977215, -288.8947816867756728, -243.9455879633486006 ) ) ;
#40980 = CARTESIAN_POINT ( 'NONE',  ( -33.93809357080956346, -124.0300793293349244, -358.8670080828285336 ) ) ;
#40981 = CARTESIAN_POINT ( 'NONE',  ( 28.86836508021439940, -286.6430427303849342, -239.4707358779378694 ) ) ;
#40982 = CARTESIAN_POINT ( 'NONE',  ( 204.6539576904058606, 300.0210572133868823, -5.225551010890672643 ) ) ;
#40983 = TOROIDAL_SURFACE ( 'NONE', #31964, 3.342139515347635204, 0.5000000000000000000 ) ;
#40984 = CARTESIAN_POINT ( 'NONE',  ( 26.53277250174978619, -283.0555388229089999, -312.9389521118226298 ) ) ;
#40985 = CARTESIAN_POINT ( 'NONE',  ( -70.78434638461257578, -290.6804907733452410, -201.2640151084531226 ) ) ;
#40986 = CARTESIAN_POINT ( 'NONE',  ( -6.572284064420578886, -282.0495870283688760, -200.6355662389266854 ) ) ;
#40987 = CARTESIAN_POINT ( 'NONE',  ( 38.69071129616798999, -282.7544173024307952, -261.3910481009908722 ) ) ;
#40988 = CARTESIAN_POINT ( 'NONE',  ( 35.68742566989009646, -281.3620502239274401, -268.5856944877209571 ) ) ;
#40989 = CARTESIAN_POINT ( 'NONE',  ( -84.18520332195230083, -295.6759877703877919, -331.5404225690522253 ) ) ;
#40990 = CARTESIAN_POINT ( 'NONE',  ( -111.0471424113618042, -288.4189246737976191, -282.2465348646594521 ) ) ;
#40991 = CARTESIAN_POINT ( 'NONE',  ( -35.12226306307413637, -297.0009042531316368, -197.0524225634412403 ) ) ;
#40992 = VERTEX_POINT ( 'NONE', #22232 ) ;
#40993 = ORIENTED_EDGE ( 'NONE', *, *, #6032, .F. ) ;
#40994 = CARTESIAN_POINT ( 'NONE',  ( -111.5289138776900302, -286.3930167990264977, -276.4906784917459390 ) ) ;
#40995 = CARTESIAN_POINT ( 'NONE',  ( 38.93116929254586722, -294.7383758919842194, -278.8469501064081442 ) ) ;
#40996 = CARTESIAN_POINT ( 'NONE',  ( 3.453974984907793200, -283.1392718720291555, -331.0821056064041272 ) ) ;
#40997 = CARTESIAN_POINT ( 'NONE',  ( -66.12783175073917619, -272.7432462658574082, -199.1839481271519503 ) ) ;
#40998 = CARTESIAN_POINT ( 'NONE',  ( -77.12364163750277157, -292.1855127121544911, -204.4915740136052875 ) ) ;
#40999 = CARTESIAN_POINT ( 'NONE',  ( -98.33552481205525453, -283.2996234009774525, -225.3297643827825141 ) ) ;
#41000 = CARTESIAN_POINT ( 'NONE',  ( 20.36002676216346075, -293.1950654803507632, -219.3877453523765837 ) ) ;
#41001 = CARTESIAN_POINT ( 'NONE',  ( 25.71645034331005419, -288.3918729451954732, -307.2816975188655420 ) ) ;
#41002 = DIRECTION ( 'NONE',  ( 0.000000000000000000, 1.000000000000000000, 0.000000000000000000 ) ) ;
#41003 = DIRECTION ( 'NONE',  ( 1.000000000000000000, -0.000000000000000000, -0.000000000000000000 ) ) ;
#41004 = CARTESIAN_POINT ( 'NONE',  ( -111.0017296283295707, -270.8980037439225157, -283.6562794664417879 ) ) ;
#41005 = CARTESIAN_POINT ( 'NONE',  ( -58.27776522270531956, -284.8379308715856837, -343.7945080851740158 ) ) ;
#41006 = CARTESIAN_POINT ( 'NONE',  ( -95.95921662488163406, -282.6952119285918457, -223.5744983911110353 ) ) ;
#41007 = ORIENTED_EDGE ( 'NONE', *, *, #5504, .T. ) ;
#41008 = CARTESIAN_POINT ( 'NONE',  ( 35.87395248041093510, -280.5210855256756304, -274.0616971121617098 ) ) ;
#41009 = CARTESIAN_POINT ( 'NONE',  ( -38.54888472703695612, -276.7336221989515366, -347.3305079826367887 ) ) ;
#41010 = CARTESIAN_POINT ( 'NONE',  ( -109.3901680170536252, -280.8136479791787110, -250.0886624119323471 ) ) ;
#41011 = CARTESIAN_POINT ( 'NONE',  ( 204.5909265758118067, 292.7456558654929495, -53.99999999999697309 ) ) ;
#41012 = CARTESIAN_POINT ( 'NONE',  ( -11.68993548917152658, -278.9543417305906701, -198.3292203697543812 ) ) ;
#41013 = CARTESIAN_POINT ( 'NONE',  ( -109.3544814497171558, -282.3178547304559629, -290.0564759326584863 ) ) ;
#41014 = CARTESIAN_POINT ( 'NONE',  ( -62.53055105828439508, -299.4889568815985399, -198.6708410858421132 ) ) ;
#41015 = CARTESIAN_POINT ( 'NONE',  ( 23.38891612813890220, -293.4808946815847435, -229.7436255584644300 ) ) ;
#41016 = ORIENTED_EDGE ( 'NONE', *, *, #82386, .F. ) ;
#41017 = CARTESIAN_POINT ( 'NONE',  ( -49.75565389035584474, -290.5754591043964865, -197.8723210307584850 ) ) ;
#41018 = CARTESIAN_POINT ( 'NONE',  ( 14.82013526042823592, -276.9917270619812939, -326.9354187106717404 ) ) ;
#41019 = CARTESIAN_POINT ( 'NONE',  ( -36.73606981722915776, -274.0599701988010111, -197.3512152546650213 ) ) ;
#41020 = CARTESIAN_POINT ( 'NONE',  ( -76.26393811409228363, -272.4653375313710626, -204.2198718604255419 ) ) ;
#41021 = PLANE ( 'NONE',  #8391 ) ;
#41022 = CARTESIAN_POINT ( 'NONE',  ( 17.83788013527916050, -272.8415312382531397, -219.4908323982217269 ) ) ;
#41023 = CARTESIAN_POINT ( 'NONE',  ( -43.54160339317391504, -248.0334966641272842, -474.9578934535559824 ) ) ;
#41024 = CARTESIAN_POINT ( 'NONE',  ( -5.887893459300612697, -283.7083868166416778, -336.5933850397269680 ) ) ;
#41025 = CARTESIAN_POINT ( 'NONE',  ( 34.36389418194562495, -282.9891025477809308, -245.0588858332488655 ) ) ;
#41026 = CARTESIAN_POINT ( 'NONE',  ( -109.2918805855209712, -284.0719324168400135, -257.3654096347033260 ) ) ;
#41027 = CARTESIAN_POINT ( 'NONE',  ( 27.34747739560153690, -273.4708344689531714, -234.7334258174505237 ) ) ;
#41028 = CARTESIAN_POINT ( 'NONE',  ( -19.25618201513518102, -282.1476046482051174, -198.3094791408386754 ) ) ;
#41029 = CARTESIAN_POINT ( 'NONE',  ( 34.18677836911302137, -273.8002544740293729, -252.6302263465097724 ) ) ;
#41030 = DIRECTION ( 'NONE',  ( 0.000000000000000000, 0.000000000000000000, 1.000000000000000000 ) ) ;
#41031 = CARTESIAN_POINT ( 'NONE',  ( 35.89498921751919625, -276.5759526496502758, -266.1073878607876964 ) ) ;
#41032 = FACE_OUTER_BOUND ( 'NONE', #68034, .T. ) ;
#41033 = CARTESIAN_POINT ( 'NONE',  ( -74.93786875106941636, -280.3673766076088327, -203.3485301688253344 ) ) ;
#41034 = ORIENTED_EDGE ( 'NONE', *, *, #90146, .T. ) ;
#41035 = EDGE_LOOP ( 'NONE', ( #85380, #47066, #42042, #16919 ) ) ;
#41036 = CARTESIAN_POINT ( 'NONE',  ( 196.2760846862221058, 19.11198087481172081, 12.12215979492540896 ) ) ;
#41037 = CARTESIAN_POINT ( 'NONE',  ( -112.2695581055860004, -286.5597132902533417, -258.7840618111244453 ) ) ;
#41038 = CARTESIAN_POINT ( 'NONE',  ( -18.18804956194439626, -293.9960510009242967, -340.9708864035305282 ) ) ;
#41039 = CARTESIAN_POINT ( 'NONE',  ( -89.42853896968865968, -289.1118691119034452, -326.9320823178122168 ) ) ;
#41040 = EDGE_CURVE ( 'NONE', #13153, #6020, #32245, .T. ) ;
#41041 = CARTESIAN_POINT ( 'NONE',  ( -27.68241467193774596, -284.4163637195857746, -196.9807921682487972 ) ) ;
#41043 = CARTESIAN_POINT ( 'NONE',  ( -20.92609229013621785, -287.0784369559788161, -342.5310690022453741 ) ) ;
#41042 = CARTESIAN_POINT ( 'NONE',  ( 17.34052456815976129, -285.4272333429417472, -221.0956838386867105 ) ) ;
#41044 = CARTESIAN_POINT ( 'NONE',  ( -87.18730424682998148, -284.9701123275049781, -324.3059212820268158 ) ) ;
#41045 = CARTESIAN_POINT ( 'NONE',  ( 34.56841783194239781, -273.8269462204076490, -291.7121402763479523 ) ) ;
#41046 = AXIS2_PLACEMENT_3D ( 'NONE', #71142, #11497, #26644 ) ;
#41047 = CARTESIAN_POINT ( 'NONE',  ( 37.24469658391227966, -285.7541029660586105, -254.6994679130625343 ) ) ;
#41048 = CARTESIAN_POINT ( 'NONE',  ( -95.80380541415016182, -299.1986782225042703, -223.3804528207505768 ) ) ;
#41049 = CARTESIAN_POINT ( 'NONE',  ( 37.51923030184178032, -285.6387572784083204, -277.1338220136053678 ) ) ;
#41050 = AXIS2_PLACEMENT_3D ( 'NONE', #14805, #78274, #41792 ) ;
#41051 = CARTESIAN_POINT ( 'NONE',  ( -32.96087733198928049, -281.0499519129303394, -197.2569673476132266 ) ) ;
#41052 = CARTESIAN_POINT ( 'NONE',  ( -74.72914985887028649, -291.5487809407809436, -335.5700669834781706 ) ) ;
#41053 = DIRECTION ( 'NONE',  ( 0.000000000000000000, 0.000000000000000000, -1.000000000000000000 ) ) ;
#41054 = CARTESIAN_POINT ( 'NONE',  ( 154.1415209985679269, 20.37991841447901464, 11.45812909362557441 ) ) ;
#41055 = CARTESIAN_POINT ( 'NONE',  ( -70.15990221002310534, -297.4012268675285213, -338.4362087182920504 ) ) ;
#41056 = CIRCLE ( 'NONE', #7835, 2.842139515347646750 ) ;
#41057 = CARTESIAN_POINT ( 'NONE',  ( -4.664704406898105837, -278.4824537590569093, -202.8539731433333770 ) ) ;
#41058 = CARTESIAN_POINT ( 'NONE',  ( 32.04455791834918443, -292.3239142321250483, -237.2267358849973675 ) ) ;
#41059 = CARTESIAN_POINT ( 'NONE',  ( -100.5718153847858787, -295.4711962084401762, -232.2040246678462267 ) ) ;
#41060 = CARTESIAN_POINT ( 'NONE',  ( 13.68950125206323243, -279.4699642856195396, -217.4029444286035471 ) ) ;
#41061 = CARTESIAN_POINT ( 'NONE',  ( -51.81801856788109006, -271.9454752426740924, -197.2894743900849619 ) ) ;
#41062 = CARTESIAN_POINT ( 'NONE',  ( 18.35705956718997101, -295.5457357073779576, -318.3270702093866475 ) ) ;
#41063 = CARTESIAN_POINT ( 'NONE',  ( 10.59707575819634329, -289.1948066931273615, -210.1954327657594490 ) ) ;
#41064 = CARTESIAN_POINT ( 'NONE',  ( -86.99628088328472586, -295.8556977659026757, -212.3507284482672048 ) ) ;
#41065 = CARTESIAN_POINT ( 'NONE',  ( -55.91906201822835953, -290.0561298046563934, -196.6261291310442800 ) ) ;
#41066 = ADVANCED_FACE ( 'NONE', ( #15126 ), #43989, .F. ) ;
#41067 = CARTESIAN_POINT ( 'NONE',  ( -77.59249977129567810, -292.9254054567558683, -208.7555334598870900 ) ) ;
#41068 = DIRECTION ( 'NONE',  ( 0.000000000000000000, 0.000000000000000000, -1.000000000000000000 ) ) ;
#41069 = CARTESIAN_POINT ( 'NONE',  ( -108.2675357336823794, -291.5919497537067286, -252.3622252116168170 ) ) ;
#41070 = CARTESIAN_POINT ( 'NONE',  ( 139.6925840978351516, 15.36528803885690664, 22.50000000000000000 ) ) ;
#41071 = CARTESIAN_POINT ( 'NONE',  ( -89.21128656762166997, -290.9680590858306459, -326.7309212488149228 ) ) ;
#41073 = CARTESIAN_POINT ( 'NONE',  ( 34.83797523761040082, -293.7004506830211881, -281.6029558478151671 ) ) ;
#41072 = CARTESIAN_POINT ( 'NONE',  ( 21.22856885401114013, -280.2221483384781209, -317.7938120302768539 ) ) ;
#41074 = CARTESIAN_POINT ( 'NONE',  ( -4.943987858190243223, -280.4670622808420717, -200.5084999952766509 ) ) ;
#41075 = CARTESIAN_POINT ( 'NONE',  ( -90.42663185398420467, -283.4455469431989059, -326.1812675011128704 ) ) ;
#41076 = CARTESIAN_POINT ( 'NONE',  ( -96.41308611418976682, -287.9203992113521622, -316.3230952909382836 ) ) ;
#41077 = CARTESIAN_POINT ( 'NONE',  ( -109.9328245700958604, -282.4894047668310009, -285.9584448127796463 ) ) ;
#41078 = CARTESIAN_POINT ( 'NONE',  ( 157.7277585059063938, 1.242640687119286103, -10.00000000000000355 ) ) ;
#41079 = CARTESIAN_POINT ( 'NONE',  ( 18.66455657022052605, -279.3196935458660164, -218.5344167227259504 ) ) ;
#41080 = CARTESIAN_POINT ( 'NONE',  ( 0.1447540201736723098, -285.4594398357559726, -203.4412846360525577 ) ) ;
#41081 = CARTESIAN_POINT ( 'NONE',  ( 195.5826719941578347, 41.40013651751736745, 14.51828210624160675 ) ) ;
#41082 = CARTESIAN_POINT ( 'NONE',  ( 22.44092148809162168, -294.5531993029314322, -227.0674906946891269 ) ) ;
#41083 = CARTESIAN_POINT ( 'NONE',  ( -59.47684553821569864, -278.7585819558410662, -343.4955259535610708 ) ) ;
#41084 = CARTESIAN_POINT ( 'NONE',  ( -72.85600040899018381, -277.2031654759853723, -334.1784976719630436 ) ) ;
#41085 = CARTESIAN_POINT ( 'NONE',  ( -114.1122943306870496, -290.6363573704136343, -276.9557053438076650 ) ) ;
#41086 = CARTESIAN_POINT ( 'NONE',  ( -44.31121230131459043, -281.2193612437335446, -345.6513683574550555 ) ) ;
#41087 = CARTESIAN_POINT ( 'NONE',  ( 21.50841941490298126, -293.2201259787927938, -313.9509319124732656 ) ) ;
#41088 = CARTESIAN_POINT ( 'NONE',  ( -110.3221715027138998, -294.7739764965101017, -253.0737974500453902 ) ) ;
#41089 = CARTESIAN_POINT ( 'NONE',  ( 153.1687287787850948, 19.71439303874801752, 10.22517819559350727 ) ) ;
#41090 = CARTESIAN_POINT ( 'NONE',  ( 28.44723814067911505, -293.4908881261306419, -302.2551843027393943 ) ) ;
#41091 = CARTESIAN_POINT ( 'NONE',  ( 189.9243309297870610, 275.0000000000000568, 15.22542485937351664 ) ) ;
#41092 = CARTESIAN_POINT ( 'NONE',  ( -105.5937364680635966, -281.8380690714489560, -285.9065529553535612 ) ) ;
#41093 = CARTESIAN_POINT ( 'NONE',  ( -106.9580446188182918, -295.1956398645567106, -302.7089895049489314 ) ) ;
#41094 = CARTESIAN_POINT ( 'NONE',  ( 33.18347853754416832, -279.3334083564326988, -242.5319898106522487 ) ) ;
#41095 = CARTESIAN_POINT ( 'NONE',  ( -37.99514509914298799, -287.3592933896689487, -193.8570574067196048 ) ) ;
#41096 = CARTESIAN_POINT ( 'NONE',  ( -14.56398944898162995, -286.1889561105984967, -200.9526672256791642 ) ) ;
#41097 = CARTESIAN_POINT ( 'NONE',  ( -87.55393819312332937, -279.2886687997292370, -324.3003328419721356 ) ) ;
#41098 = CARTESIAN_POINT ( 'NONE',  ( -96.08307975919393584, -293.9371522448985843, -316.4186594490874995 ) ) ;
#41099 = CARTESIAN_POINT ( 'NONE',  ( -109.8733455967555983, -298.1197511453075322, -285.1596232922974536 ) ) ;
#41100 = CARTESIAN_POINT ( 'NONE',  ( -74.22601906662013960, -276.3491885353718089, -333.8172250289101157 ) ) ;
#41101 = VERTEX_POINT ( 'NONE', #8475 ) ;
#41102 = CARTESIAN_POINT ( 'NONE',  ( -102.2962767623809981, -296.7605036603702047, -229.0495304344446765 ) ) ;
#41103 = CARTESIAN_POINT ( 'NONE',  ( -76.60797044999216610, -291.5022224941862987, -333.6025143307660414 ) ) ;
#41104 = CARTESIAN_POINT ( 'NONE',  ( 20.77089707463454360, -295.8236021285290462, -319.6497217736782090 ) ) ;
#41105 = CARTESIAN_POINT ( 'NONE',  ( 201.7545824283169225, 292.3729076405792284, -53.99999999997594813 ) ) ;
#41106 = CARTESIAN_POINT ( 'NONE',  ( 27.12426616765833032, -288.6740425020491898, -304.9367141524379008 ) ) ;
#41107 = CARTESIAN_POINT ( 'NONE',  ( -48.18343439339133027, -248.3668650814815066, -463.3519808654870076 ) ) ;
#41108 = CARTESIAN_POINT ( 'NONE',  ( 24.05966901727094864, -281.2260032550470328, -316.4338005692189881 ) ) ;
#41109 = CARTESIAN_POINT ( 'NONE',  ( -111.8678020810175013, -296.9654994036794733, -289.3661116125622925 ) ) ;
#41110 = CARTESIAN_POINT ( 'NONE',  ( -110.0401751519187883, -288.9637283464268762, -249.0248293968679718 ) ) ;
#41111 = CARTESIAN_POINT ( 'NONE',  ( -70.72371292266220166, -297.9571016812775497, -200.9969664814844066 ) ) ;
#41112 = CIRCLE ( 'NONE', #50270, 24.50000000000000000 ) ;
#41113 = DIRECTION ( 'NONE',  ( 0.000000000000000000, 1.000000000000000000, 0.000000000000000000 ) ) ;
#41114 = CARTESIAN_POINT ( 'NONE',  ( 0.000000000000000000, 0.000000000000000000, -9.000000000000001776 ) ) ;
#41115 = CARTESIAN_POINT ( 'NONE',  ( 195.4637550158223576, 27.11842685737634184, 15.00000000000008704 ) ) ;
#41116 = CARTESIAN_POINT ( 'NONE',  ( 16.21326865916951476, -289.8292784396544448, -324.7905985224219876 ) ) ;
#41117 = CARTESIAN_POINT ( 'NONE',  ( -115.3288506153726871, -294.2666405000204009, -252.5284128619063608 ) ) ;
#41118 = VERTEX_POINT ( 'NONE', #66715 ) ;
#41119 = CARTESIAN_POINT ( 'NONE',  ( 34.23259412519036715, -280.5422164157160410, -242.1010992490742808 ) ) ;
#41120 = CARTESIAN_POINT ( 'NONE',  ( -110.4615939364114183, -286.7579729771636607, -254.3792174287803789 ) ) ;
#41121 = CARTESIAN_POINT ( 'NONE',  ( 37.52728857025744702, -286.3193587878362223, -285.6333419849396478 ) ) ;
#41122 = CARTESIAN_POINT ( 'NONE',  ( 1.587401756308150835, -272.5737339517414171, -206.4506066993375271 ) ) ;
#41123 = CARTESIAN_POINT ( 'NONE',  ( -107.6747952551809817, -274.7903097030651338, -245.9773133815993447 ) ) ;
#41125 = CARTESIAN_POINT ( 'NONE',  ( -103.6820029439865749, -289.0831070532123590, -236.4790781022847739 ) ) ;
#41124 = VECTOR ( 'NONE', #12343, 1000.000000000000000 ) ;
#41126 = CARTESIAN_POINT ( 'NONE',  ( -113.1486265574077947, -280.3966697992362924, -271.6120325674877449 ) ) ;
#41128 = CARTESIAN_POINT ( 'NONE',  ( 34.03815350793523464, -281.1085283059636026, -286.1348037747450803 ) ) ;
#41127 = CARTESIAN_POINT ( 'NONE',  ( -7.999445884722894640, -280.4475527640443602, -203.5041054592432488 ) ) ;
#41129 = CARTESIAN_POINT ( 'NONE',  ( -28.62247023842397553, -278.0238402580508250, -346.6080977672831409 ) ) ;
#41130 = CARTESIAN_POINT ( 'NONE',  ( -45.21720561371426328, -278.7495688390453665, -194.1113859238821249 ) ) ;
#41131 = CARTESIAN_POINT ( 'NONE',  ( 159.2613953296296643, 219.3517484348739401, -203.0981120538807545 ) ) ;
#41132 = CARTESIAN_POINT ( 'NONE',  ( -94.91796165021136744, -274.1829569011866852, -219.5891343453561433 ) ) ;
#41133 = EDGE_CURVE ( 'NONE', #25769, #81416, #14413, .T. ) ;
#41134 = CARTESIAN_POINT ( 'NONE',  ( -109.4530370487537283, -274.3897128112149062, -245.4079049736626246 ) ) ;
#41135 = CARTESIAN_POINT ( 'NONE',  ( 31.98288692825981272, -290.4805209788416391, -303.7098442033569654 ) ) ;
#41136 = VERTEX_POINT ( 'NONE', #9872 ) ;
#41137 = CARTESIAN_POINT ( 'NONE',  ( 156.4947056272797852, 21.00000000000000000, -15.00000000000000000 ) ) ;
#41138 = CARTESIAN_POINT ( 'NONE',  ( 35.98918607386463719, -288.6046246368758261, -268.2900672227270320 ) ) ;
#41139 = CARTESIAN_POINT ( 'NONE',  ( 32.91385123181829186, -288.9379057052419171, -241.2732564096131682 ) ) ;
#41140 = CARTESIAN_POINT ( 'NONE',  ( -50.77832957252943658, -288.5768004351575655, -342.2693218052381212 ) ) ;
#41141 = CARTESIAN_POINT ( 'NONE',  ( -104.3664900499624082, -283.5679844076287281, -308.2473987396795678 ) ) ;
#41142 = CARTESIAN_POINT ( 'NONE',  ( 19.46480550931818954, -279.2909681565450910, -223.2303382217800163 ) ) ;
#41143 = CARTESIAN_POINT ( 'NONE',  ( -71.77179245318097855, -287.4524536214564137, -204.5930845234890967 ) ) ;
#41144 = CARTESIAN_POINT ( 'NONE',  ( 36.39632857189117487, -280.0448416946348971, -271.3421247772542984 ) ) ;
#41145 = CARTESIAN_POINT ( 'NONE',  ( -98.41268100256962725, -280.4324349415506390, -229.3857787574259817 ) ) ;
#41146 = CARTESIAN_POINT ( 'NONE',  ( -35.10947924728646541, -277.5157167606794815, -343.3885486628410604 ) ) ;
#41147 = CARTESIAN_POINT ( 'NONE',  ( -89.23382792912653372, -288.5582957521842786, -326.7101711242518718 ) ) ;
#41148 = CARTESIAN_POINT ( 'NONE',  ( -102.7752060292336296, -284.8273778980123438, -310.6428151376581468 ) ) ;
#41149 = CARTESIAN_POINT ( 'NONE',  ( -74.24095428152287468, -284.0211171267319514, -337.9333141188182026 ) ) ;
#41150 = CARTESIAN_POINT ( 'NONE',  ( -29.44254347037384179, -283.1161327696497665, -342.9829888053851050 ) ) ;
#41151 = VERTEX_POINT ( 'NONE', #87532 ) ;
#41152 = DIRECTION ( 'NONE',  ( 0.000000000000000000, -1.000000000000000000, 0.000000000000000000 ) ) ;
#41153 = CARTESIAN_POINT ( 'NONE',  ( -97.16941640809957903, -291.7815902524616831, -316.8471357616768955 ) ) ;
#41154 = CARTESIAN_POINT ( 'NONE',  ( 20.94568398526683595, -291.5643690565316888, -220.7842708659962625 ) ) ;
#41155 = CARTESIAN_POINT ( 'NONE',  ( -3.986854391651197371, -273.5620172079876511, -205.1483984843130770 ) ) ;
#41156 = CARTESIAN_POINT ( 'NONE',  ( -97.33313446893353671, -295.2551120485818501, -318.4895539335668673 ) ) ;
#41157 = CARTESIAN_POINT ( 'NONE',  ( -17.22490996144808406, -290.7962931388438506, -199.4135753120056336 ) ) ;
#41158 = CARTESIAN_POINT ( 'NONE',  ( -5.120342306461822091, -292.8619564273380433, -337.0066277221436621 ) ) ;
#41159 = CARTESIAN_POINT ( 'NONE',  ( -99.16802386047204720, -291.2130351277514251, -309.9166005146893212 ) ) ;
#41160 = CARTESIAN_POINT ( 'NONE',  ( 202.8019728163925492, 61.40723988820079171, -7.000000000000000888 ) ) ;
#41161 = CARTESIAN_POINT ( 'NONE',  ( -110.3107676467127050, -292.3290191752894884, -287.7513845534626284 ) ) ;
#41162 = CARTESIAN_POINT ( 'NONE',  ( -34.99159093599732984, -290.0814155835148540, -195.2183576876095970 ) ) ;
#41163 = CARTESIAN_POINT ( 'NONE',  ( -71.42834417707278760, -297.5024156777060398, -337.1817468121076899 ) ) ;
#41164 = CARTESIAN_POINT ( 'NONE',  ( 18.83455950827622161, -287.8284171611957731, -223.3560945960349784 ) ) ;
#41165 = CARTESIAN_POINT ( 'NONE',  ( -11.65908633609343426, -296.7187942262509637, -341.0593362159445405 ) ) ;
#41166 = CARTESIAN_POINT ( 'NONE',  ( 10.71689283427927819, -276.6920719183102619, -212.2521525024003779 ) ) ;
#41167 = CARTESIAN_POINT ( 'NONE',  ( 98.84066493780467511, -298.9135927194789701, -193.5404977642008930 ) ) ;
#41168 = CARTESIAN_POINT ( 'NONE',  ( 5.971903607451601204, -274.6959184177126758, -330.4402727933716619 ) ) ;
#41169 = CARTESIAN_POINT ( 'NONE',  ( -62.77847166040100291, -277.7984397897478175, -200.3475505220830541 ) ) ;
#41170 = CARTESIAN_POINT ( 'NONE',  ( -35.14592078867098479, -299.3953797982574088, -196.8674597293335466 ) ) ;
#41171 = CARTESIAN_POINT ( 'NONE',  ( 23.17736608043865587, -273.4993226203873746, -223.6916750528299076 ) ) ;
#41172 = CARTESIAN_POINT ( 'NONE',  ( -68.75248953991011547, -296.8985641019899049, -336.9237171196394911 ) ) ;
#41173 = CARTESIAN_POINT ( 'NONE',  ( -35.09237171215954021, -122.5496321078137356, -21.49999999999998579 ) ) ;
#41174 = CARTESIAN_POINT ( 'NONE',  ( -107.7554486521644037, -297.0930039502329123, -290.2232866971413046 ) ) ;
#41175 = DIRECTION ( 'NONE',  ( 0.000000000000000000, 0.000000000000000000, -1.000000000000000000 ) ) ;
#41176 = AXIS2_PLACEMENT_3D ( 'NONE', #73245, #8356, #22559 ) ;
#41178 = CARTESIAN_POINT ( 'NONE',  ( -92.01675149714054669, -273.0765498590686775, -221.9913054719793877 ) ) ;
#41177 = CARTESIAN_POINT ( 'NONE',  ( -26.40864434976349884, -286.9337763603784879, -344.9189820346633724 ) ) ;
#41179 = VECTOR ( 'NONE', #51072, 1000.000000000000000 ) ;
#41180 = CARTESIAN_POINT ( 'NONE',  ( -49.34472809488563882, -285.9033314182544814, -194.2486724588901836 ) ) ;
#41181 = CARTESIAN_POINT ( 'NONE',  ( -82.84356402013463594, -289.3224670658993318, -332.4523788313267687 ) ) ;
#41182 = CARTESIAN_POINT ( 'NONE',  ( -111.9762840897595595, -298.6660994108328282, -259.8711284591287267 ) ) ;
#41183 = CARTESIAN_POINT ( 'NONE',  ( -8.548441092542681474, -292.6742987303485961, -339.4473200087999771 ) ) ;
#41184 = CIRCLE ( 'NONE', #74465, 4.000000000000003553 ) ;
#41185 = CARTESIAN_POINT ( 'NONE',  ( 39.45808755723345485, -280.7798951619258787, -272.8006735779704854 ) ) ;
#41186 = CARTESIAN_POINT ( 'NONE',  ( -20.19161114001082069, -289.7666405000204577, -195.3683826091709363 ) ) ;
#41187 = AXIS2_PLACEMENT_3D ( 'NONE', #30126, #8341, #37223 ) ;
#41188 = CARTESIAN_POINT ( 'NONE',  ( 4.254320565826858136, -278.6123115460059125, -207.8917537791145946 ) ) ;
#41189 = CARTESIAN_POINT ( 'NONE',  ( 228.6245981097501101, -141.7221692137691775, -21.50000000000000000 ) ) ;
#41190 = CARTESIAN_POINT ( 'NONE',  ( 12.41376360154817604, -287.1357938658919693, -324.3887089515143316 ) ) ;
#41191 = ADVANCED_FACE ( 'NONE', ( #37808 ), #60550, .T. ) ;
#41192 = CARTESIAN_POINT ( 'NONE',  ( 160.5350683151633291, 275.5000000000000568, 20.22542485937379908 ) ) ;
#41193 = CARTESIAN_POINT ( 'NONE',  ( -73.34061479046752652, -287.5294987980494739, -336.1568533582429836 ) ) ;
#41194 = CARTESIAN_POINT ( 'NONE',  ( -94.24330054535435863, -298.8114375956258186, -223.3451945514177623 ) ) ;
#41195 = CARTESIAN_POINT ( 'NONE',  ( 1.807949475871903688, -283.9644313694084303, -335.9805604405766530 ) ) ;
#41197 = CARTESIAN_POINT ( 'NONE',  ( 27.78139285383101154, -281.1029593220091556, -237.2644502935618505 ) ) ;
#41196 = CARTESIAN_POINT ( 'NONE',  ( -64.91613223996833426, -295.7140085549717128, -200.1764909488042861 ) ) ;
#41198 = CARTESIAN_POINT ( 'NONE',  ( -111.2147876921270182, -296.4458546349878247, -292.1278166581992082 ) ) ;
#41199 = CARTESIAN_POINT ( 'NONE',  ( -3.852615762558396550, -275.9281586949315965, -204.8194512522468074 ) ) ;
#41200 = EDGE_CURVE ( 'NONE', #77986, #65497, #37355, .T. ) ;
#41201 = CARTESIAN_POINT ( 'NONE',  ( -12.20431818888519793, -282.3792223700725685, -199.6446373813822959 ) ) ;
#41202 = CARTESIAN_POINT ( 'NONE',  ( -110.6508120073928012, -271.4726545095895744, -270.3474032455676479 ) ) ;
#41203 = ORIENTED_EDGE ( 'NONE', *, *, #12372, .F. ) ;
#41204 = CARTESIAN_POINT ( 'NONE',  ( 204.7706911773244087, 294.8516371035053680, -54.00000000003474554 ) ) ;
#41205 = CARTESIAN_POINT ( 'NONE',  ( -63.15481001598478628, -287.6943202866786464, -200.2664975874406537 ) ) ;
#41206 = CARTESIAN_POINT ( 'NONE',  ( 133.0872704186301405, -299.5541904835127980, -195.3611179825600175 ) ) ;
#41207 = CARTESIAN_POINT ( 'NONE',  ( 40.65961533371913106, -272.8380690714490129, -252.5904736702033802 ) ) ;
#41208 = CARTESIAN_POINT ( 'NONE',  ( -112.6374533610341331, -277.5565052924652605, -285.7463783904381671 ) ) ;
#41209 = CARTESIAN_POINT ( 'NONE',  ( -113.2082757868019627, -289.0488828482635881, -262.6969488846294780 ) ) ;
#41210 = CARTESIAN_POINT ( 'NONE',  ( -26.62297940217047554, -284.4335973981821439, -343.3225546131592978 ) ) ;
#41211 = CARTESIAN_POINT ( 'NONE',  ( 28.56669927013647836, -276.7065000514105009, -237.1568516633402623 ) ) ;
#41212 = AXIS2_PLACEMENT_3D ( 'NONE', #57452, #36120, #37049 ) ;
#41213 = CARTESIAN_POINT ( 'NONE',  ( -99.29996126232215659, -285.3788704107144554, -315.1684156594441788 ) ) ;
#41214 = CARTESIAN_POINT ( 'NONE',  ( -103.3765806782274552, -282.9142958194165658, -302.5173212792527124 ) ) ;
#41215 = CARTESIAN_POINT ( 'NONE',  ( -37.02475649072119523, -282.0562785229693645, -195.3617833173209704 ) ) ;
#41216 = CARTESIAN_POINT ( 'NONE',  ( -49.72133113237252644, -274.0652513636412095, -194.3089917652966392 ) ) ;
#41217 = CARTESIAN_POINT ( 'NONE',  ( -91.33054965403859171, -277.6275420282493087, -325.3375551474478584 ) ) ;
#41218 = CARTESIAN_POINT ( 'NONE',  ( -28.70510105053843120, -296.8620878543105732, -344.3504327012894919 ) ) ;
#41219 = CYLINDRICAL_SURFACE ( 'NONE', #49024, 24.99999999999999645 ) ;
#41220 = DIRECTION ( 'NONE',  ( -1.124465274301078034E-16, -1.000000000000000000, 0.000000000000000000 ) ) ;
#41221 = CARTESIAN_POINT ( 'NONE',  ( -113.0018702431286641, -294.6297757981480459, -275.2359043707697310 ) ) ;
#41222 = CARTESIAN_POINT ( 'NONE',  ( 30.33266191769419962, -275.4299375486892245, -298.0305782652033599 ) ) ;
#41223 = CARTESIAN_POINT ( 'NONE',  ( -31.95041609189772913, -299.1978304314974366, -193.6692652193777633 ) ) ;
#41224 = CARTESIAN_POINT ( 'NONE',  ( -38.66520113531282021, -287.7955088978765161, -196.3469609180639566 ) ) ;
#41225 = CARTESIAN_POINT ( 'NONE',  ( -32.04117046317639961, -296.5065739624205889, -346.4966029843527622 ) ) ;
#41226 = CARTESIAN_POINT ( 'NONE',  ( 34.08698560629319019, -294.4031349381732525, -242.5387764450289012 ) ) ;
#41227 = CARTESIAN_POINT ( 'NONE',  ( -111.2252005397637191, -292.3983347650163864, -282.3266985220449214 ) ) ;
#41228 = CARTESIAN_POINT ( 'NONE',  ( 8.279669297338815070, -278.6773768291982947, -210.9767458494015102 ) ) ;
#41229 = CARTESIAN_POINT ( 'NONE',  ( -104.6827629162619360, -280.8940871006320208, -238.5145631335620351 ) ) ;
#41230 = CARTESIAN_POINT ( 'NONE',  ( -111.1610214454702401, -294.7611161423004091, -260.3798860915666751 ) ) ;
#41231 = CARTESIAN_POINT ( 'NONE',  ( -55.38469703066005678, -285.1423157109778685, -343.9461418704025277 ) ) ;
#41232 = CARTESIAN_POINT ( 'NONE',  ( -110.6284198035847481, -283.4294252206301508, -273.6383000622860209 ) ) ;
#41233 = CARTESIAN_POINT ( 'NONE',  ( 204.9738707124548966, 293.6304025755547968, -68.53118252596463833 ) ) ;
#41234 = EDGE_LOOP ( 'NONE', ( #54153, #22267, #58546, #87067 ) ) ;
#41235 = CARTESIAN_POINT ( 'NONE',  ( -62.56619406408992035, -285.3815198943786982, -201.7811976918543166 ) ) ;
#41236 = ORIENTED_EDGE ( 'NONE', *, *, #32846, .T. ) ;
#41237 = CARTESIAN_POINT ( 'NONE',  ( 11.30717336774200632, -283.4760513993695668, -329.7154246927971144 ) ) ;
#41238 = CARTESIAN_POINT ( 'NONE',  ( -99.30066256563158333, -273.4186113689000308, -231.7195023278788426 ) ) ;
#41239 = CARTESIAN_POINT ( 'NONE',  ( 38.96063145376592729, -286.2546751330123129, -263.0107060427403667 ) ) ;
#41240 = CARTESIAN_POINT ( 'NONE',  ( 39.40489128974311939, -282.4519348231373215, -267.0555165994222762 ) ) ;
#41241 = CARTESIAN_POINT ( 'NONE',  ( -48.37443537269673755, -278.7101166351053507, -345.9194027389390271 ) ) ;
#41242 = CARTESIAN_POINT ( 'NONE',  ( -3.709690086294829214, -281.1357149427943227, -201.1931624113720716 ) ) ;
#41243 = CARTESIAN_POINT ( 'NONE',  ( -109.1418805571601069, -276.0523547857346784, -270.3284710469131937 ) ) ;
#41244 = CARTESIAN_POINT ( 'NONE',  ( 201.0027984253578666, 288.7662968377554193, -97.50545772727659255 ) ) ;
#41245 = ORIENTED_EDGE ( 'NONE', *, *, #44575, .T. ) ;
#41246 = CIRCLE ( 'NONE', #474, 4.000000000000003553 ) ;
#41247 = CARTESIAN_POINT ( 'NONE',  ( -93.40821220137200953, -275.2430403368559837, -220.7972737791770328 ) ) ;
#41248 = CARTESIAN_POINT ( 'NONE',  ( 4.936003717816790370, -58.01961007492668898, -354.3995137328890905 ) ) ;
#41249 = AXIS2_PLACEMENT_3D ( 'NONE', #48863, #69716, #75879 ) ;
#41250 = CARTESIAN_POINT ( 'NONE',  ( -109.8822779568667727, -276.7993404582289827, -252.7624994333112056 ) ) ;
#41251 = CARTESIAN_POINT ( 'NONE',  ( 36.76795595612152567, -295.0989027623976995, -253.5179565413668854 ) ) ;
#41252 = CARTESIAN_POINT ( 'NONE',  ( -42.40505393370229825, -294.4662792987087983, -343.2874857553237007 ) ) ;
#41253 = CARTESIAN_POINT ( 'NONE',  ( -0.8275322185403718445, -292.0314911855879245, -202.6393161368531821 ) ) ;
#41254 = DIRECTION ( 'NONE',  ( -3.330669073875469227E-15, 0.000000000000000000, 1.000000000000000000 ) ) ;
#41255 = EDGE_CURVE ( 'NONE', #61775, #70776, #54948, .T. ) ;
#41256 = VECTOR ( 'NONE', #56510, 1000.000000000000000 ) ;
#41258 = CARTESIAN_POINT ( 'NONE',  ( 24.16509862317047919, -286.5121115119811179, -311.1684298047982793 ) ) ;
#41257 = CARTESIAN_POINT ( 'NONE',  ( -107.8384937025143415, -294.7475540741158397, -299.9736937379801702 ) ) ;
#41259 = CARTESIAN_POINT ( 'NONE',  ( 19.40575695475984475, -294.7438685615165923, -222.5009926431640110 ) ) ;
#41260 = EDGE_CURVE ( 'NONE', #1135, #27540, #89389, .T. ) ;
#41261 = CARTESIAN_POINT ( 'NONE',  ( -103.4489830572864548, -285.4341400746934028, -302.5882270590924463 ) ) ;
#41262 = ORIENTED_EDGE ( 'NONE', *, *, #6894, .F. ) ;
#41263 = CARTESIAN_POINT ( 'NONE',  ( -114.1337742174287229, -291.5183455598047431, -268.3728042826384126 ) ) ;
#41264 = CIRCLE ( 'NONE', #4999, 0.4999999999999923395 ) ;
#41265 = CARTESIAN_POINT ( 'NONE',  ( 31.41463957922851336, -282.3750754717723908, -295.2201340125697584 ) ) ;
#41266 = CARTESIAN_POINT ( 'NONE',  ( -61.48106938854082415, -294.1536938479402465, -343.1166396591279408 ) ) ;
#41267 = CARTESIAN_POINT ( 'NONE',  ( -73.08965571483332724, -290.3165170562892285, -338.3923295689095880 ) ) ;
#41268 = CARTESIAN_POINT ( 'NONE',  ( -78.09848545163190181, -290.0764527527808809, -335.6797670342228912 ) ) ;
#41269 = CARTESIAN_POINT ( 'NONE',  ( 4.723633750092860240, -286.8043202912064658, -210.6376514534353817 ) ) ;
#41270 = ORIENTED_EDGE ( 'NONE', *, *, #14110, .T. ) ;
#41271 = CARTESIAN_POINT ( 'NONE',  ( 221.8344101925596306, -0.9999999999999991118, 22.50000000000000000 ) ) ;
#41272 = CARTESIAN_POINT ( 'NONE',  ( -91.79255679770795950, -297.6790261288470560, -323.0432751886407345 ) ) ;
#41273 = VECTOR ( 'NONE', #1347, 1000.000000000000000 ) ;
#41274 = CARTESIAN_POINT ( 'NONE',  ( -29.10869328681776835, -296.8380300421357560, -193.8560607233932274 ) ) ;
#41275 = CARTESIAN_POINT ( 'NONE',  ( -67.39191009270089694, -278.7068357384384854, -203.5612929295071467 ) ) ;
#41276 = CARTESIAN_POINT ( 'NONE',  ( -21.36144848974205601, -273.7594791896040647, -195.1005143400768702 ) ) ;
#41277 = CARTESIAN_POINT ( 'NONE',  ( -107.3595220539818911, -295.3360999246783081, -247.2166030724141592 ) ) ;
#41278 = CARTESIAN_POINT ( 'NONE',  ( -93.64831600126241540, -279.7352095245564101, -318.7391139244425631 ) ) ;
#41279 = CARTESIAN_POINT ( 'NONE',  ( 36.06660057890775306, -273.5472873996151861, -259.2261164537891318 ) ) ;
#41280 = CARTESIAN_POINT ( 'NONE',  ( -75.85340846279034110, -296.7835291980024408, -332.9021927488255983 ) ) ;
#41281 = CARTESIAN_POINT ( 'NONE',  ( -94.70174383783722760, -298.2737644288790761, -224.7097055140803832 ) ) ;
#41282 = CARTESIAN_POINT ( 'NONE',  ( -23.40286736638519471, -122.5496321078137356, 21.50000000000000000 ) ) ;
#41283 = CARTESIAN_POINT ( 'NONE',  ( -85.86999987757030794, -297.3117120165575784, -329.1101140322011247 ) ) ;
#41284 = CIRCLE ( 'NONE', #74562, 7.500000000000012434 ) ;
#41285 = CARTESIAN_POINT ( 'NONE',  ( -37.23011418868981792, -296.0533920953740221, -195.1937350554261172 ) ) ;
#41286 = CARTESIAN_POINT ( 'NONE',  ( -90.83943233965777608, -291.9190547891043366, -220.5240839346854216 ) ) ;
#41287 = CARTESIAN_POINT ( 'NONE',  ( -94.97215231731705387, -274.0445598521916395, -219.5389790939195223 ) ) ;
#41288 = CARTESIAN_POINT ( 'NONE',  ( -92.86818249434146821, -288.4431866215342097, -318.7299902590988268 ) ) ;
#41289 = DIRECTION ( 'NONE',  ( 0.000000000000000000, 0.000000000000000000, -1.000000000000000000 ) ) ;
#41290 = CARTESIAN_POINT ( 'NONE',  ( 24.42671822047764252, -275.4340821579542080, -224.4896737266387845 ) ) ;
#41291 = CARTESIAN_POINT ( 'NONE',  ( -110.4052107008391204, -296.8708425278252321, -271.4676713260424776 ) ) ;
#41292 = CARTESIAN_POINT ( 'NONE',  ( 2.921368067043745853, -282.5691681888419566, -206.6026171118178922 ) ) ;
#41293 = CARTESIAN_POINT ( 'NONE',  ( 37.38024129389184225, -280.4445437357587139, -286.8510985108100044 ) ) ;
#41294 = CARTESIAN_POINT ( 'NONE',  ( -109.6437641215550514, -277.5678098567039456, -296.7032733476090129 ) ) ;
#41295 = CARTESIAN_POINT ( 'NONE',  ( 38.07653713332280887, -280.0896152924329385, -281.2482619475419483 ) ) ;
#41296 = CARTESIAN_POINT ( 'NONE',  ( 37.05303910510736642, -279.6896477433839436, -281.1059400452538171 ) ) ;
#41297 = CARTESIAN_POINT ( 'NONE',  ( -62.21189748978583367, -272.2969730615606068, -201.1018355722397075 ) ) ;
#41298 = CARTESIAN_POINT ( 'NONE',  ( -26.75690723031630824, -278.9178193966616846, -344.6622788111404816 ) ) ;
#41299 = CARTESIAN_POINT ( 'NONE',  ( 222.4306832106270804, -134.2391364535880882, 21.50000000000000000 ) ) ;
#41300 = CARTESIAN_POINT ( 'NONE',  ( -36.09237171215955442, -122.5496321078137356, 21.50000000000000000 ) ) ;
#41301 = CARTESIAN_POINT ( 'NONE',  ( -20.76251538403682417, -296.4968702432226451, -194.3793322445775118 ) ) ;
#41302 = CARTESIAN_POINT ( 'NONE',  ( -2.055838212670591858, -292.5062544488460503, -201.9072583069217046 ) ) ;
#41303 = CARTESIAN_POINT ( 'NONE',  ( -23.25684604428048630, -278.8727487948989392, -344.2492734776062093 ) ) ;
#41304 = CARTESIAN_POINT ( 'NONE',  ( -51.92610362168312577, -271.8654817042391301, -196.7396059933332424 ) ) ;
#41305 = CARTESIAN_POINT ( 'NONE',  ( 132.9888089158688445, -299.5541904835127980, -195.3611179825600175 ) ) ;
#41306 = CARTESIAN_POINT ( 'NONE',  ( -109.3064616375037303, -286.1767439981734924, -293.4338811728729297 ) ) ;
#41307 = CARTESIAN_POINT ( 'NONE',  ( 159.0442047513576824, 16.65459343288188165, -10.27557066714188139 ) ) ;
#41308 = CARTESIAN_POINT ( 'NONE',  ( -16.22858399576231037, -286.7791815031728788, -342.3815504752983543 ) ) ;
#41309 = DIRECTION ( 'NONE',  ( 0.000000000000000000, -1.000000000000000000, -0.000000000000000000 ) ) ;
#41310 = CARTESIAN_POINT ( 'NONE',  ( -31.58644725277014231, -293.7729414118836644, -343.5825881740855721 ) ) ;
#41311 = CARTESIAN_POINT ( 'NONE',  ( 5.456503627177974991, -284.7775506207781859, -209.6419621142031247 ) ) ;
#41312 = CARTESIAN_POINT ( 'NONE',  ( 154.9307753191121435, 19.94580804509866567, -10.40578999956973405 ) ) ;
#41313 = CARTESIAN_POINT ( 'NONE',  ( 31.31084012750758561, -291.9474178873009009, -300.5576304016474296 ) ) ;
#41314 = CARTESIAN_POINT ( 'NONE',  ( -37.95725395690548254, -284.5244563489983420, -194.0569316687667367 ) ) ;
#41315 = CARTESIAN_POINT ( 'NONE',  ( -111.1519674929121209, -280.1843802921181918, -267.9017107689502382 ) ) ;
#41316 = CARTESIAN_POINT ( 'NONE',  ( 23.53648252730269519, -288.1338406805382419, -223.8438576788823298 ) ) ;
#41317 = CARTESIAN_POINT ( 'NONE',  ( 35.50075884867473519, -280.0691117090692046, -292.1741021061494621 ) ) ;
#41318 = CARTESIAN_POINT ( 'NONE',  ( 20.35746322284307652, -288.1821815778940277, -315.1005538123423548 ) ) ;
#41319 = CIRCLE ( 'NONE', #53440, 4.000000000000003553 ) ;
#41320 = CARTESIAN_POINT ( 'NONE',  ( -108.8666207872145151, -280.2039538355605828, -253.0532976802600160 ) ) ;
#41321 = CARTESIAN_POINT ( 'NONE',  ( -24.85886971923855171, -281.0183180349987992, -198.2724179561660947 ) ) ;
#41322 = CARTESIAN_POINT ( 'NONE',  ( -57.34413665464356313, -287.7753045629299891, -197.6549696322861678 ) ) ;
#41323 = MECHANICAL_DESIGN_GEOMETRIC_PRESENTATION_REPRESENTATION (  '', ( #17149 ), #48918 ) ;
#41324 = EDGE_LOOP ( 'NONE', ( #83660, #79692, #31644, #80954 ) ) ;
#41325 = AXIS2_PLACEMENT_3D ( 'NONE', #72421, #35506, #50157 ) ;
#41326 = CARTESIAN_POINT ( 'NONE',  ( -37.25145703024865895, -297.8865755847954233, -193.3603567442300459 ) ) ;
#41327 = CARTESIAN_POINT ( 'NONE',  ( -79.07355589496947346, -291.5975144955892233, -332.3127405254086284 ) ) ;
#41328 = DIRECTION ( 'NONE',  ( -0.000000000000000000, 1.000000000000000000, -0.000000000000000000 ) ) ;
#41329 = CARTESIAN_POINT ( 'NONE',  ( -37.30987171927208124, -291.5519495502701375, -350.3611179825600175 ) ) ;
#41330 = ORIENTED_EDGE ( 'NONE', *, *, #51459, .T. ) ;
#41331 = CARTESIAN_POINT ( 'NONE',  ( 22.19667473073898378, -272.9245274682088507, -224.4575875660702877 ) ) ;
#41332 = CYLINDRICAL_SURFACE ( 'NONE', #35281, 8.000000000000000000 ) ;
#41333 = CARTESIAN_POINT ( 'NONE',  ( -95.90974742083152194, -294.2893140455722119, -319.1279444767243376 ) ) ;
#41334 = CARTESIAN_POINT ( 'NONE',  ( -81.97676093716518153, -296.9328507611767236, -212.4549782014388200 ) ) ;
#41335 = AXIS2_PLACEMENT_3D ( 'NONE', #41667, #25589, #54473 ) ;
#41336 = CARTESIAN_POINT ( 'NONE',  ( -64.05433036862241636, -290.9270105524314545, -339.0972726322552262 ) ) ;
#41338 = EDGE_CURVE ( 'NONE', #88799, #63820, #45818, .T. ) ;
#41337 = CARTESIAN_POINT ( 'NONE',  ( 36.52989528231221783, -283.2527311973069573, -265.7827555074986776 ) ) ;
#41339 = CARTESIAN_POINT ( 'NONE',  ( -110.2143621876788302, -291.6844106967669177, -293.5160393329211388 ) ) ;
#41340 = CARTESIAN_POINT ( 'NONE',  ( -70.41065345981498069, -290.7940611967126188, -339.3663976293753990 ) ) ;
#41341 = CARTESIAN_POINT ( 'NONE',  ( -41.45747046174550121, -288.0005051087389916, -195.4612886322359202 ) ) ;
#41342 = CARTESIAN_POINT ( 'NONE',  ( -11.51135464438669409, -280.5460374620005837, -197.7669172733149026 ) ) ;
#41343 = CARTESIAN_POINT ( 'NONE',  ( -78.70941993553368832, -293.6846139679248608, -333.5910630584564274 ) ) ;
#41344 = CARTESIAN_POINT ( 'NONE',  ( -38.73467545788268040, -282.9024924014703970, -347.3485171090485437 ) ) ;
#41345 = AXIS2_PLACEMENT_3D ( 'NONE', #78615, #14235, #13759 ) ;
#41346 = CARTESIAN_POINT ( 'NONE',  ( 34.44256959712029698, -277.6582121440334845, -289.2789429787712265 ) ) ;
#41347 = CARTESIAN_POINT ( 'NONE',  ( -67.74223827176244583, -282.1233781216987495, -207.3071070584150277 ) ) ;
#41348 = CARTESIAN_POINT ( 'NONE',  ( 35.08984844880483678, -274.0845875652014456, -293.3316378803804696 ) ) ;
#41349 = DIRECTION ( 'NONE',  ( 0.000000000000000000, 1.000000000000000000, 0.000000000000000000 ) ) ;
#41350 = CARTESIAN_POINT ( 'NONE',  ( 34.62879086799097195, -280.8940019097055938, -257.7818943358235515 ) ) ;
#41351 = CIRCLE ( 'NONE', #2110, 3.000000000000000888 ) ;
#41352 = CARTESIAN_POINT ( 'NONE',  ( -94.90223437500507941, -279.0696455736311350, -320.9060842645401976 ) ) ;
#41353 = CARTESIAN_POINT ( 'NONE',  ( -10.06631755336795564, -285.4583106441060636, -198.5488340660893982 ) ) ;
#41354 = CARTESIAN_POINT ( 'NONE',  ( 11.58409444775172936, -294.5017767363566463, -214.7568083912356087 ) ) ;
#41355 = CARTESIAN_POINT ( 'NONE',  ( -63.30387613299685512, -275.3195813716937437, -198.7203067652910704 ) ) ;
#41356 = CARTESIAN_POINT ( 'NONE',  ( -110.5700346080669760, -274.1492930871249314, -248.0234173299515419 ) ) ;
#41357 = CARTESIAN_POINT ( 'NONE',  ( -55.80257052418233599, -229.5268262511776527, 25.50000000000000000 ) ) ;
#41358 = CARTESIAN_POINT ( 'NONE',  ( 34.70680804688093701, -275.5444737867629783, -282.4143692279272386 ) ) ;
#41359 = CARTESIAN_POINT ( 'NONE',  ( -53.52155392867422279, -297.2602238345237993, -343.4776699596290541 ) ) ;
#41360 = CARTESIAN_POINT ( 'NONE',  ( -22.06119998568924245, -284.2480557287098009, -197.0512943070299912 ) ) ;
#41361 = CARTESIAN_POINT ( 'NONE',  ( -33.53616458209059914, -291.7655474367319925, -193.4763848375828843 ) ) ;
#41362 = CARTESIAN_POINT ( 'NONE',  ( 36.25144443124563765, -273.4101979276783823, -257.7992226760327981 ) ) ;
#41363 = CARTESIAN_POINT ( 'NONE',  ( 33.30834032176397130, -289.5201148833864409, -299.0501748027612052 ) ) ;
#41364 = CARTESIAN_POINT ( 'NONE',  ( -103.8309236640189397, -289.8875277130449604, -239.4837925441728714 ) ) ;
#41365 = ORIENTED_EDGE ( 'NONE', *, *, #12942, .F. ) ;
#41366 = CARTESIAN_POINT ( 'NONE',  ( 18.99360916416825518, -291.4191886706000787, -218.7380686725811074 ) ) ;
#41367 = CARTESIAN_POINT ( 'NONE',  ( -94.30473399079460251, -290.8645809552307355, -224.6542686835606730 ) ) ;
#41368 = ORIENTED_EDGE ( 'NONE', *, *, #74810, .T. ) ;
#41369 = CARTESIAN_POINT ( 'NONE',  ( 33.56834547272224967, -288.2575454174322545, -241.0118656208562129 ) ) ;
#41370 = CARTESIAN_POINT ( 'NONE',  ( -108.1915638814336802, -278.6516486110755864, -288.0870483253908674 ) ) ;
#41371 = CARTESIAN_POINT ( 'NONE',  ( 22.03853054096587627, -293.1268058947201780, -318.9150237479514090 ) ) ;
#41372 = CARTESIAN_POINT ( 'NONE',  ( -114.0508273546338103, -285.2799104626408848, -264.2645916975442333 ) ) ;
#41373 = CARTESIAN_POINT ( 'NONE',  ( -109.2816787757773227, -284.5369166733178758, -297.9027642643281979 ) ) ;
#41374 = CARTESIAN_POINT ( 'NONE',  ( 35.58725195009324693, -281.9338106551800820, -274.0292831194072392 ) ) ;
#41375 = CARTESIAN_POINT ( 'NONE',  ( 5.511235791697614239, -58.25811859054644515, -354.7422047037252355 ) ) ;
#41376 = CARTESIAN_POINT ( 'NONE',  ( -72.21123258206935702, -195.3303827311551402, -359.1388006984578283 ) ) ;
#41377 = CARTESIAN_POINT ( 'NONE',  ( 197.7106711174764655, 286.7663448939923114, -96.38273171682746465 ) ) ;
#41378 = CARTESIAN_POINT ( 'NONE',  ( 25.50907715839022671, -275.2630468307652336, -307.8095027429330912 ) ) ;
#41379 = CARTESIAN_POINT ( 'NONE',  ( -32.41345497286733490, -275.9090238474583998, -343.5545697824167632 ) ) ;
#41380 = CARTESIAN_POINT ( 'NONE',  ( -101.4949129165882198, -296.6192087254643184, -227.8648787276140126 ) ) ;
#41381 = CARTESIAN_POINT ( 'NONE',  ( -104.7359985975682974, -260.9361277188981489, -315.7277192616979846 ) ) ;
#41382 = EDGE_CURVE ( 'NONE', #14856, #66468, #80639, .T. ) ;
#41383 = CARTESIAN_POINT ( 'NONE',  ( 22.24629620678343045, -274.8844703966639713, -318.3669252183344156 ) ) ;
#41384 = CARTESIAN_POINT ( 'NONE',  ( -46.32367503924465524, -275.6967808600020930, -196.8948118342178759 ) ) ;
#41385 = VERTEX_POINT ( 'NONE', #9394 ) ;
#41386 = CARTESIAN_POINT ( 'NONE',  ( -109.6333203565924919, -297.8203368701824161, -244.5397729879170754 ) ) ;
#41387 = CARTESIAN_POINT ( 'NONE',  ( 3.654318923425740273, -288.9766697818042189, -330.8978636715258403 ) ) ;
#41388 = CARTESIAN_POINT ( 'NONE',  ( -108.2221221050199631, -296.9753003042635555, -300.1656769617289910 ) ) ;
#41389 = CARTESIAN_POINT ( 'NONE',  ( -66.89500004176926495, -295.9215229857758800, -341.4114208345997099 ) ) ;
#41390 = CARTESIAN_POINT ( 'NONE',  ( 28.39547615711503425, -294.1498093294815703, -302.2207882684590459 ) ) ;
#41391 = ORIENTED_EDGE ( 'NONE', *, *, #29603, .T. ) ;
#41392 = CARTESIAN_POINT ( 'NONE',  ( 25.71512263424697409, -276.9143873373876659, -228.7299841902427318 ) ) ;
#41393 = ORIENTED_EDGE ( 'NONE', *, *, #19155, .T. ) ;
#41394 = CARTESIAN_POINT ( 'NONE',  ( -31.07251517508866101, -279.6368727734683830, -193.6258493168994335 ) ) ;
#41395 = AXIS2_PLACEMENT_3D ( 'NONE', #10315, #4622, #33495 ) ;
#41396 = CARTESIAN_POINT ( 'NONE',  ( -45.92381204645155890, -278.1047561628644758, -343.1426139705459946 ) ) ;
#41397 = CARTESIAN_POINT ( 'NONE',  ( 21.05749831130191296, -276.6496372410165350, -221.7451983856155664 ) ) ;
#41398 = CARTESIAN_POINT ( 'NONE',  ( -94.90932168836425831, -275.9027043147746667, -319.0058896495945078 ) ) ;
#41399 = CARTESIAN_POINT ( 'NONE',  ( -95.37504497151657290, -297.8282749759426338, -225.8882324612126524 ) ) ;
#41400 = CARTESIAN_POINT ( 'NONE',  ( -110.6354344245422254, -295.2202618890138410, -263.2246067501200173 ) ) ;
#41401 = CARTESIAN_POINT ( 'NONE',  ( 175.2296996224750103, 250.0000000000000568, 0.000000000000000000 ) ) ;
#41402 = CARTESIAN_POINT ( 'NONE',  ( -50.93492052454265462, -280.3752551515775622, -194.6329774909152377 ) ) ;
#41403 = CARTESIAN_POINT ( 'NONE',  ( 23.98553936077475512, -276.2681252530847473, -310.0519248803364576 ) ) ;
#41404 = VECTOR ( 'NONE', #79552, 1000.000000000000000 ) ;
#41405 = CARTESIAN_POINT ( 'NONE',  ( 15.96764387764321569, -285.4737880948593443, -215.4847832503679399 ) ) ;
#41406 = CARTESIAN_POINT ( 'NONE',  ( -32.09572632087548527, -300.1178316423048500, -195.1926590726061193 ) ) ;
#41407 = CARTESIAN_POINT ( 'NONE',  ( 82.62739761238445624, -301.2431227241796137, -197.2117082864666600 ) ) ;
#41408 = TOROIDAL_SURFACE ( 'NONE', #626, 4.499999999999993783, 0.5000000000000000000 ) ;
#41409 = CARTESIAN_POINT ( 'NONE',  ( 30.63142610091495754, -287.1122188855687227, -297.5579312345154790 ) ) ;
#41410 = AXIS2_PLACEMENT_3D ( 'NONE', #61892, #60964, #24491 ) ;
#41411 = CARTESIAN_POINT ( 'NONE',  ( -70.16984558620852397, -277.8534006830432190, -204.0124247109837370 ) ) ;
#41413 = CARTESIAN_POINT ( 'NONE',  ( -105.4402984434636323, -282.2352360419093884, -300.4259662696737223 ) ) ;
#41412 = CARTESIAN_POINT ( 'NONE',  ( -59.89711201537725316, -278.3289551617787652, -200.2600583664776934 ) ) ;
#41414 = CARTESIAN_POINT ( 'NONE',  ( -65.75662015852823572, -287.6807968292244482, -200.8978323062794971 ) ) ;
#41415 = CARTESIAN_POINT ( 'NONE',  ( -95.93797296480778414, -280.3749618890283273, -226.1406204970063527 ) ) ;
#41416 = FACE_BOUND ( 'NONE', #43459, .T. ) ;
#41417 = CARTESIAN_POINT ( 'NONE',  ( -36.42897949586679829, -294.0637537311178562, -195.3539741908275573 ) ) ;
#41419 = CARTESIAN_POINT ( 'NONE',  ( -102.7451726378532868, -276.2802090978213982, -309.1471627736226537 ) ) ;
#41418 = CIRCLE ( 'NONE', #73225, 3.491568894204821749 ) ;
#41420 = CARTESIAN_POINT ( 'NONE',  ( 29.25053169632317918, -276.6094312538228337, -300.5168359889639191 ) ) ;
#41421 = CARTESIAN_POINT ( 'NONE',  ( 36.18586380700367755, -283.3515133553473220, -254.6879192266613359 ) ) ;
#41422 = DIRECTION ( 'NONE',  ( -1.000000000000000000, -0.000000000000000000, -0.000000000000000000 ) ) ;
#41423 = CARTESIAN_POINT ( 'NONE',  ( -62.26515384258541985, -291.2938208454318669, -341.7476097961869641 ) ) ;
#41424 = CARTESIAN_POINT ( 'NONE',  ( -87.43994764063363334, -293.7503938971767070, -326.2434960983061387 ) ) ;
#41425 = CARTESIAN_POINT ( 'NONE',  ( -113.9899638730542932, -283.8258988624224912, -264.2508779054703609 ) ) ;
#41426 = CARTESIAN_POINT ( 'NONE',  ( 161.2244399300530233, 8.542400036368780647, 10.00000000000000000 ) ) ;
#41427 = CARTESIAN_POINT ( 'NONE',  ( 13.85209836054729315, -273.4734954537382805, -217.6312547771131563 ) ) ;
#41428 = CARTESIAN_POINT ( 'NONE',  ( -38.90015348860767830, -290.1719784934156223, -196.1422746456413222 ) ) ;
#41429 = CARTESIAN_POINT ( 'NONE',  ( 202.9738562182569694, 296.4636489450776367, -53.99999999999997868 ) ) ;
#41430 = CARTESIAN_POINT ( 'NONE',  ( 159.4851178187871312, 15.00000000000000000, 6.999999999999998224 ) ) ;
#41431 = CARTESIAN_POINT ( 'NONE',  ( -101.0939488831900519, -289.5893851261556620, -228.3335476889303379 ) ) ;
#41432 = CARTESIAN_POINT ( 'NONE',  ( -101.0819459649954410, -285.6472829774787101, -307.5581806947480459 ) ) ;
#41433 = CARTESIAN_POINT ( 'NONE',  ( 37.78711643400389164, -285.6466208005097656, -258.8885846512430930 ) ) ;
#41434 = CARTESIAN_POINT ( 'NONE',  ( -102.7705054953186590, -286.4316196384670548, -236.6795749106795768 ) ) ;
#41435 = CARTESIAN_POINT ( 'NONE',  ( -4.531289960885949597, -287.2988412736495434, -204.9693852317697917 ) ) ;
#41436 = CARTESIAN_POINT ( 'NONE',  ( -78.71292160567136875, -293.4781675314818017, -207.3159641016412138 ) ) ;
#41437 = CARTESIAN_POINT ( 'NONE',  ( 36.76519531547990738, -273.8199522145540072, -285.1083973468112163 ) ) ;
#41438 = CARTESIAN_POINT ( 'NONE',  ( 39.60961237824037795, -275.8596739927569956, -268.3020417353718585 ) ) ;
#41439 = CARTESIAN_POINT ( 'NONE',  ( -41.94140849047675346, -290.0744507505808656, -194.9412473780233768 ) ) ;
#41440 = CARTESIAN_POINT ( 'NONE',  ( -110.6666676216834588, -278.2546883081078022, -294.0370261877187090 ) ) ;
#41441 = CARTESIAN_POINT ( 'NONE',  ( -39.71666763639395015, -297.0619874879278655, -344.9808414646738015 ) ) ;
#41442 = CARTESIAN_POINT ( 'NONE',  ( -48.18343439339133027, -253.7029054207625052, -479.0169286797143968 ) ) ;
#41443 = CARTESIAN_POINT ( 'NONE',  ( 208.0393982316568326, 37.47427918878998554, 12.98477611641282614 ) ) ;
#41444 = CARTESIAN_POINT ( 'NONE',  ( -105.6786303335850192, -282.8760221689911987, -297.5424248709305175 ) ) ;
#41445 = CARTESIAN_POINT ( 'NONE',  ( -104.3762601446401703, -276.9975555546783994, -236.6097080058894448 ) ) ;
#41446 = DIRECTION ( 'NONE',  ( -0.000000000000000000, -1.000000000000000000, -0.000000000000000000 ) ) ;
#41447 = CARTESIAN_POINT ( 'NONE',  ( -31.29552210731097261, -272.6070602186015890, -194.2811993839129627 ) ) ;
#41448 = CARTESIAN_POINT ( 'NONE',  ( -35.12284158092999320, -276.3721413132199700, -343.4293691948372498 ) ) ;
#41449 = CARTESIAN_POINT ( 'NONE',  ( 33.79098080276330762, -295.3248334093859171, -289.6665972240092515 ) ) ;
#41450 = CARTESIAN_POINT ( 'NONE',  ( 38.56335310471677502, -280.6099883000420618, -281.3117071650368644 ) ) ;
#41451 = CARTESIAN_POINT ( 'NONE',  ( -73.40787444732877987, -296.4844850177152011, -334.0999563649610309 ) ) ;
#41452 = CARTESIAN_POINT ( 'NONE',  ( -64.07806012873268742, -296.7089265687841930, -342.0442075254208021 ) ) ;
#41453 = CARTESIAN_POINT ( 'NONE',  ( -36.48127492339978772, -297.8965383374562066, -197.3611431048962856 ) ) ;
#41454 = CARTESIAN_POINT ( 'NONE',  ( -92.24004992895380894, -293.2675844134609520, -219.2424956665714433 ) ) ;
#41455 = CARTESIAN_POINT ( 'NONE',  ( -112.3602088651110051, -284.9358911517914521, -253.0053307226875461 ) ) ;
#41456 = CARTESIAN_POINT ( 'NONE',  ( 30.16071396225005330, -273.2414297244706631, -235.9557467476845716 ) ) ;
#41457 = CARTESIAN_POINT ( 'NONE',  ( 31.68648011654244456, -287.8252788996738900, -304.6004228847726267 ) ) ;
#41458 = CARTESIAN_POINT ( 'NONE',  ( -94.36262064907354841, -281.2016807607589612, -222.1702798802900531 ) ) ;
#41459 = CARTESIAN_POINT ( 'NONE',  ( -85.87313592555500463, -284.4193181181659043, -215.4471252058430082 ) ) ;
#41460 = CARTESIAN_POINT ( 'NONE',  ( -36.37780040960624461, -290.0640810599271617, -195.3546134821183671 ) ) ;
#41461 = CARTESIAN_POINT ( 'NONE',  ( -72.39245198575343920, -211.1690049852372226, -355.6323962662157783 ) ) ;
#41462 = TOROIDAL_SURFACE ( 'NONE', #684, 24.16304133878946558, 4.003189038634632269 ) ;
#41463 = CARTESIAN_POINT ( 'NONE',  ( 11.17960546522221321, -286.2532224697061451, -215.6701459217152888 ) ) ;
#41464 = CARTESIAN_POINT ( 'NONE',  ( 155.0786878258427066, 18.48484813926865655, 9.250287988714237741 ) ) ;
#41465 = CARTESIAN_POINT ( 'NONE',  ( -2.987354850028779207, -283.5506475113002125, -339.0241008027304588 ) ) ;
#41466 = CARTESIAN_POINT ( 'NONE',  ( -109.6479822902343955, -289.2827295766998077, -296.2990371597725812 ) ) ;
#41467 = CARTESIAN_POINT ( 'NONE',  ( -84.09235222965038759, -281.0221604726231703, -210.1211068474909212 ) ) ;
#41468 = CARTESIAN_POINT ( 'NONE',  ( -95.54163159470810740, -280.5416025944564353, -220.6814874622443767 ) ) ;
#41469 = CARTESIAN_POINT ( 'NONE',  ( 15.26085450888212947, -280.6539499138401084, -219.6729841377985508 ) ) ;
#41470 = CARTESIAN_POINT ( 'NONE',  ( 1.630558087549926150, -276.5734098269544461, -206.2817629779650872 ) ) ;
#41471 = CARTESIAN_POINT ( 'NONE',  ( 17.56154560499861716, -294.2940206919910793, -324.4243018859324934 ) ) ;
#41472 = VECTOR ( 'NONE', #48189, 1000.000000000000000 ) ;
#41473 = CARTESIAN_POINT ( 'NONE',  ( -109.3316657499150466, -288.8272000385535989, -250.6306427063725266 ) ) ;
#41474 = CARTESIAN_POINT ( 'NONE',  ( -79.89635740851900891, -296.3814757464465401, -210.6675067955377756 ) ) ;
#41475 = ORIENTED_EDGE ( 'NONE', *, *, #89206, .F. ) ;
#41476 = ORIENTED_EDGE ( 'NONE', *, *, #27512, .F. ) ;
#41477 = CARTESIAN_POINT ( 'NONE',  ( -13.03653723666044861, -284.6541846856612779, -340.7760969264413689 ) ) ;
#41478 = CARTESIAN_POINT ( 'NONE',  ( -77.96502750404248161, -295.2811527920156323, -331.1003016930922058 ) ) ;
#41479 = CARTESIAN_POINT ( 'NONE',  ( 8.654503940854340271, -293.7452787957932401, -208.9283932366735712 ) ) ;
#41480 = VECTOR ( 'NONE', #74954, 1000.000000000000114 ) ;
#41481 = CARTESIAN_POINT ( 'NONE',  ( -33.48255945011700163, -283.6537431950467862, -343.3737060117775854 ) ) ;
#41482 = EDGE_CURVE ( 'NONE', #16610, #86290, #77613, .T. ) ;
#41483 = CARTESIAN_POINT ( 'NONE',  ( -2.653111489142776502, -273.5582507639357459, -201.8663742341396699 ) ) ;
#41484 = CARTESIAN_POINT ( 'NONE',  ( -111.5366392243365823, -291.4575787174883317, -250.1016344997444776 ) ) ;
#41485 = CARTESIAN_POINT ( 'NONE',  ( -70.50386244415177828, -283.7591896734205079, -202.2393411752990744 ) ) ;
#41486 = CARTESIAN_POINT ( 'NONE',  ( -91.58061881280454486, -290.1321316693956760, -325.0610376856986363 ) ) ;
#41487 = CARTESIAN_POINT ( 'NONE',  ( 34.58747631600389383, -287.7157585265050557, -257.4950100333157366 ) ) ;
#41488 = CARTESIAN_POINT ( 'NONE',  ( 196.8803347170859865, 73.40565171261609123, -12.49999999999998579 ) ) ;
#41489 = CARTESIAN_POINT ( 'NONE',  ( 153.7700350902760533, 129.6490463903463990, -11.80126012119838030 ) ) ;
#41490 = CARTESIAN_POINT ( 'NONE',  ( 193.0906159184471846, 275.7967025259000593, -123.9984796719191422 ) ) ;
#41491 = CARTESIAN_POINT ( 'NONE',  ( -89.94602559131035946, -285.2986515701680332, -325.7100612913062037 ) ) ;
#41492 = CARTESIAN_POINT ( 'NONE',  ( 21.27581636871891391, -285.6952119285919025, -317.1477375740089997 ) ) ;
#41493 = EDGE_LOOP ( 'NONE', ( #34974, #64302, #38951, #84428 ) ) ;
#41494 = CARTESIAN_POINT ( 'NONE',  ( 35.66151926106301318, -280.3775458185024263, -263.1344880193751123 ) ) ;
#41495 = CARTESIAN_POINT ( 'NONE',  ( -4.007846544576714187, -276.2912354927674983, -339.7629202201153475 ) ) ;
#41496 = CARTESIAN_POINT ( 'NONE',  ( -74.91222203738804808, -279.5539075092778489, -335.0796185089115511 ) ) ;
#41497 = CARTESIAN_POINT ( 'NONE',  ( 175.6347583417331748, 240.9695037902932029, -178.4445647501395058 ) ) ;
#41498 = EDGE_CURVE ( 'NONE', #66468, #88799, #87995, .T. ) ;
#41499 = CARTESIAN_POINT ( 'NONE',  ( 37.56430762138740675, -280.3170572111532692, -285.4507269113763073 ) ) ;
#41500 = CARTESIAN_POINT ( 'NONE',  ( -94.49866316113217124, -283.2390678192696782, -222.3514483033902138 ) ) ;
#41501 = CARTESIAN_POINT ( 'NONE',  ( -111.3141019553943210, -298.0913164673240203, -287.7971380697699715 ) ) ;
#41502 = AXIS2_PLACEMENT_3D ( 'NONE', #31713, #60605, #1431 ) ;
#41503 = CARTESIAN_POINT ( 'NONE',  ( 25.84902749512648867, -294.5472004113508433, -307.0342741595256939 ) ) ;
#41504 = ORIENTED_EDGE ( 'NONE', *, *, #79580, .T. ) ;
#41505 = CARTESIAN_POINT ( 'NONE',  ( -108.2231117701188339, -289.4918107992207865, -250.9428543479009761 ) ) ;
#41506 = CARTESIAN_POINT ( 'NONE',  ( -39.95117398810393894, -277.7355083739330439, -347.2279465269218690 ) ) ;
#41507 = CARTESIAN_POINT ( 'NONE',  ( -66.82128638378274843, -297.8214885693381575, -203.5645509084472167 ) ) ;
#41508 = EDGE_LOOP ( 'NONE', ( #7403, #32668, #75859, #52877, #42314 ) ) ;
#41509 = CARTESIAN_POINT ( 'NONE',  ( -24.19900087458676552, -273.1363941837475977, -194.7508178983115386 ) ) ;
#41510 = LINE ( 'NONE', #56215, #29577 ) ;
#41511 = DIRECTION ( 'NONE',  ( -0.000000000000000000, -1.000000000000000000, -0.000000000000000000 ) ) ;
#41512 = EDGE_CURVE ( 'NONE', #64288, #88194, #6590, .T. ) ;
#41513 = CARTESIAN_POINT ( 'NONE',  ( 156.6695768423687696, 18.03393767896977451, 8.087387968559804463 ) ) ;
#41514 = CARTESIAN_POINT ( 'NONE',  ( 29.60232393066930001, -283.0339455442720578, -300.3642940624312700 ) ) ;
#41515 = CARTESIAN_POINT ( 'NONE',  ( -4.580158049601985581, -284.3866045963768556, -338.9367445439181665 ) ) ;
#41516 = CARTESIAN_POINT ( 'NONE',  ( -53.75402061754415683, -282.3265910824628122, -341.7859453671997585 ) ) ;
#41517 = CARTESIAN_POINT ( 'NONE',  ( 36.25419105348277782, -283.2815160131809762, -260.2582051990389118 ) ) ;
#41518 = CARTESIAN_POINT ( 'NONE',  ( 3.502449031520246336, -274.9716349172953755, -331.7000389930661868 ) ) ;
#41519 = CARTESIAN_POINT ( 'NONE',  ( 196.1227023549103592, 275.0000000000000568, -11.81026827902096521 ) ) ;
#41520 = CARTESIAN_POINT ( 'NONE',  ( 152.4536156746142410, 275.0000000000000568, -11.50000000000000355 ) ) ;
#41521 = CARTESIAN_POINT ( 'NONE',  ( -41.36574395494807987, -277.9044063292082001, -347.1073812851673779 ) ) ;
#41522 = ORIENTED_EDGE ( 'NONE', *, *, #27345, .T. ) ;
#41523 = ORIENTED_EDGE ( 'NONE', *, *, #8883, .T. ) ;
#41524 = CARTESIAN_POINT ( 'NONE',  ( 184.7149167944524493, 8.542400036368780647, -9.000000000000001776 ) ) ;
#41525 = CARTESIAN_POINT ( 'NONE',  ( -110.2955976910047582, -286.1521804467080869, -290.8070054030278584 ) ) ;
#41526 = CARTESIAN_POINT ( 'NONE',  ( 23.06053835761465720, -293.3235401869716270, -311.7313027195789346 ) ) ;
#41527 = CARTESIAN_POINT ( 'NONE',  ( 33.94471415763714361, -287.2689357643765788, -299.3396933785547276 ) ) ;
#41528 = CARTESIAN_POINT ( 'NONE',  ( -24.95040502862489262, -284.4520589960428083, -197.3404152852579898 ) ) ;
#41530 = CARTESIAN_POINT ( 'NONE',  ( -99.70753367729410854, -288.2482962413515111, -310.2168179338679010 ) ) ;
#41529 = CARTESIAN_POINT ( 'NONE',  ( -102.2998172363050458, -282.6581329209695355, -305.0502218231461597 ) ) ;
#41531 = CARTESIAN_POINT ( 'NONE',  ( -110.7066776044088243, -285.7857108612488446, -268.1907300975811381 ) ) ;
#41532 = CARTESIAN_POINT ( 'NONE',  ( 7.036594990000758720, -274.4481728403393390, -330.8866921735930759 ) ) ;
#41533 = CARTESIAN_POINT ( 'NONE',  ( -5.093791064963393289, -284.8694863026918824, -201.3211818632843233 ) ) ;
#41534 = CARTESIAN_POINT ( 'NONE',  ( -15.56249213115096097, -300.3249431746697269, -195.3536842308016617 ) ) ;
#41535 = CARTESIAN_POINT ( 'NONE',  ( -54.52028126809830866, -283.8317529060831816, -197.1837664763651219 ) ) ;
#41536 = CARTESIAN_POINT ( 'NONE',  ( 35.58547329939473514, -282.3981436429428413, -263.1161870991642786 ) ) ;
#41537 = EDGE_CURVE ( 'NONE', #50728, #28948, #55776, .T. ) ;
#41538 = CARTESIAN_POINT ( 'NONE',  ( 36.22384026247603828, -289.3538093336782140, -254.8671198385670209 ) ) ;
#41539 = CARTESIAN_POINT ( 'NONE',  ( 193.6552470326849402, 275.5000000000000568, 16.89672165344822119 ) ) ;
#41540 = DIRECTION ( 'NONE',  ( 0.000000000000000000, 0.000000000000000000, -1.000000000000000000 ) ) ;
#41541 = CARTESIAN_POINT ( 'NONE',  ( -92.61901793798266169, -297.7564623106414388, -321.8945566341897120 ) ) ;
#41542 = CARTESIAN_POINT ( 'NONE',  ( -3.420831710505241929, -278.4997593246368410, -203.4560727217182148 ) ) ;
#41543 = CARTESIAN_POINT ( 'NONE',  ( -112.4799072212602340, -289.9515286357162154, -254.2239865104348837 ) ) ;
#41544 = CARTESIAN_POINT ( 'NONE',  ( -39.73517681792971246, -293.4825457400801270, -344.1348644714923921 ) ) ;
#41545 = CARTESIAN_POINT ( 'NONE',  ( -101.2323203910118963, -277.7311004750494021, -234.0398828799493742 ) ) ;
#41546 = CARTESIAN_POINT ( 'NONE',  ( -37.80687756199515093, -296.1858490380373610, -196.1273716551077655 ) ) ;
#41547 = CARTESIAN_POINT ( 'NONE',  ( 32.01095838245846892, -295.1905251591877573, -294.8333896647420147 ) ) ;
#41548 = CARTESIAN_POINT ( 'NONE',  ( -114.2704648735229114, -293.0519495502702512, -270.3937649182068981 ) ) ;
#41549 = CARTESIAN_POINT ( 'NONE',  ( -113.5426982570904499, -294.9700149871536041, -275.2752556983063528 ) ) ;
#41550 = CARTESIAN_POINT ( 'NONE',  ( -10.41340708330305453, -290.2951021242247407, -339.1277056067564217 ) ) ;
#41551 = CARTESIAN_POINT ( 'NONE',  ( 21.43981081841886649, -291.1368129287019997, -222.2081535054409756 ) ) ;
#41552 = VECTOR ( 'NONE', #7130, 1000.000000000000227 ) ;
#41553 = CARTESIAN_POINT ( 'NONE',  ( -110.7085486079273551, -291.8944991757177263, -276.6985717526271742 ) ) ;
#41554 = DIRECTION ( 'NONE',  ( -1.000000000000000000, 0.000000000000000000, 0.000000000000000000 ) ) ;
#41555 = CARTESIAN_POINT ( 'NONE',  ( -83.93973002601904909, -292.1954752220521527, -213.9587657616031890 ) ) ;
#41556 = CYLINDRICAL_SURFACE ( 'NONE', #20294, 161.1282194813176716 ) ;
#41557 = CARTESIAN_POINT ( 'NONE',  ( -94.42570921331406453, -292.4536984853795047, -219.2785903849262468 ) ) ;
#41559 = CARTESIAN_POINT ( 'NONE',  ( 34.71394299542819795, -293.3967254417360095, -258.5789227502350514 ) ) ;
#41558 = CARTESIAN_POINT ( 'NONE',  ( 18.91786417711920976, -278.8776249305042825, -220.2092013673012616 ) ) ;
#41560 = CARTESIAN_POINT ( 'NONE',  ( 37.67749848607583374, -281.3344768217687601, -252.9503824223577908 ) ) ;
#41561 = CARTESIAN_POINT ( 'NONE',  ( -114.1304238725785893, -284.2953746480517907, -264.2456914075312966 ) ) ;
#41562 = AXIS2_PLACEMENT_3D ( 'NONE', #18098, #68769, #17644 ) ;
#41563 = CARTESIAN_POINT ( 'NONE',  ( -67.08045649038925262, -287.4425783561480898, -339.0869808148911488 ) ) ;
#41564 = CARTESIAN_POINT ( 'NONE',  ( -109.6335024211604008, -282.4721776528767236, -287.2915931714493922 ) ) ;
#41565 = FACE_OUTER_BOUND ( 'NONE', #67856, .T. ) ;
#41566 = CARTESIAN_POINT ( 'NONE',  ( 20.55282127485811827, -279.3548368245381539, -220.6327715716640512 ) ) ;
#41567 = EDGE_CURVE ( 'NONE', #45901, #42154, #90323, .T. ) ;
#41568 = CARTESIAN_POINT ( 'NONE',  ( -67.05654831457397336, -284.5919779865603800, -199.6609036442864067 ) ) ;
#41569 = DIRECTION ( 'NONE',  ( -0.000000000000000000, 1.000000000000000000, -0.000000000000000000 ) ) ;
#41570 = CARTESIAN_POINT ( 'NONE',  ( 36.33191401159005096, -295.0854739651622367, -265.2407560999006932 ) ) ;
#41571 = CARTESIAN_POINT ( 'NONE',  ( 6.879091576360326421, -276.0658375190361085, -207.9814464762356181 ) ) ;
#41572 = CARTESIAN_POINT ( 'NONE',  ( -108.1936299300499940, -277.9851940958232603, -288.0787889379510034 ) ) ;
#41573 = CARTESIAN_POINT ( 'NONE',  ( -69.62509661333739075, -291.8055178983028668, -200.4412521545260688 ) ) ;
#41574 = CARTESIAN_POINT ( 'NONE',  ( -92.39934421272458565, -281.9121035074234101, -322.1291997727531680 ) ) ;
#41575 = CLOSED_SHELL ( 'NONE', ( #865, #79292, #91837, #10069, #59068, #88356, #23659, #72985, #40088, #15324, #68204, #58558, #35341, #76716, #74313, #69031, #83824, #39878, #39129, #76387, #33634, #58733 ) ) ;
#41576 = CARTESIAN_POINT ( 'NONE',  ( 34.44951332011830658, -292.4206051034574330, -255.8894173084161423 ) ) ;
#41577 = CARTESIAN_POINT ( 'NONE',  ( -94.08546788035883424, -293.8718696552895722, -319.4034004788132393 ) ) ;
#41578 = ORIENTED_EDGE ( 'NONE', *, *, #6798, .T. ) ;
#41579 = CARTESIAN_POINT ( 'NONE',  ( 175.2296996224750103, 140.2072866198470251, 24.00000000000002132 ) ) ;
#41580 = CARTESIAN_POINT ( 'NONE',  ( -79.56115982651462559, -290.9724038011422067, -210.6710488745503369 ) ) ;
#41581 = CARTESIAN_POINT ( 'NONE',  ( -36.09237171215955442, -55.96374926131388605, -22.50000000000000000 ) ) ;
#41582 = CARTESIAN_POINT ( 'NONE',  ( -21.39648532958014826, -274.3380690714489560, -340.3683826091709079 ) ) ;
#41583 = CARTESIAN_POINT ( 'NONE',  ( -102.9208208713124293, -295.0882822397881000, -310.2634880261027206 ) ) ;
#41584 = CARTESIAN_POINT ( 'NONE',  ( -7.993226794930098578, -278.5721042578804258, -200.4973993423118372 ) ) ;
#41585 = CARTESIAN_POINT ( 'NONE',  ( -108.5754930492163766, -286.2250307942047698, -242.3055826994246615 ) ) ;
#41586 = CARTESIAN_POINT ( 'NONE',  ( -19.81380064240008920, -286.1171645995170252, -199.4966505528033736 ) ) ;
#41587 = CARTESIAN_POINT ( 'NONE',  ( 29.79379416280975335, -277.4780001990760638, -300.7508063137664749 ) ) ;
#41588 = CARTESIAN_POINT ( 'NONE',  ( -87.61596725676020014, -293.7783860190706946, -325.5367001267342744 ) ) ;
#41589 = CARTESIAN_POINT ( 'NONE',  ( -78.49482072034837188, -297.3742380632951949, -331.9404433679606541 ) ) ;
#41590 = CARTESIAN_POINT ( 'NONE',  ( -109.8868493745971477, -277.2007750650690809, -281.5115361781025740 ) ) ;
#41591 = VERTEX_POINT ( 'NONE', #40132 ) ;
#41592 = CARTESIAN_POINT ( 'NONE',  ( 194.8488057663960831, 40.40495866097701594, 13.83703082863031497 ) ) ;
#41593 = CARTESIAN_POINT ( 'NONE',  ( -99.99376879883324420, -295.6252415433453393, -315.1774376555846970 ) ) ;
#41594 = CARTESIAN_POINT ( 'NONE',  ( -66.87833645481680378, -291.3622593980742295, -338.7455489394475876 ) ) ;
#41595 = CYLINDRICAL_SURFACE ( 'NONE', #88412, 0.5000000000000000000 ) ;
#41596 = CARTESIAN_POINT ( 'NONE',  ( -50.76204978943955126, -289.8794172020000701, -342.2723619224744880 ) ) ;
#41598 = ORIENTED_EDGE ( 'NONE', *, *, #34788, .F. ) ;
#41597 = EDGE_CURVE ( 'NONE', #85293, #38685, #71619, .T. ) ;
#41599 = CARTESIAN_POINT ( 'NONE',  ( -50.88630447160315384, -278.9418867547200307, -194.8007850987532379 ) ) ;
#41600 = CARTESIAN_POINT ( 'NONE',  ( -110.2464297723367821, -296.8951612652207359, -294.8195149453471231 ) ) ;
#41601 = CARTESIAN_POINT ( 'NONE',  ( -102.1468385063062527, -289.2135586312229520, -231.0095459031336418 ) ) ;
#41602 = CARTESIAN_POINT ( 'NONE',  ( -82.96146110630758130, -297.7805255820161960, -208.2901946683190317 ) ) ;
#41603 = CARTESIAN_POINT ( 'NONE',  ( 21.81934756833250333, -293.2865567852622348, -227.5373111288986365 ) ) ;
#41604 = CARTESIAN_POINT ( 'NONE',  ( 196.9312215853254600, 70.66127120904285164, -10.51348395302562722 ) ) ;
#41605 = DIRECTION ( 'NONE',  ( -0.7957555401921962979, -0.6056179655966504871, 0.000000000000000000 ) ) ;
#41606 = DIRECTION ( 'NONE',  ( -0.000000000000000000, -1.000000000000000000, -0.000000000000000000 ) ) ;
#41607 = CARTESIAN_POINT ( 'NONE',  ( -20.62923130197297539, -290.3615992699166668, -344.8693166486516475 ) ) ;
#41608 = CARTESIAN_POINT ( 'NONE',  ( 13.84574458161073096, -278.9090924074131408, -334.4957818155094174 ) ) ;
#41609 = ORIENTED_EDGE ( 'NONE', *, *, #9644, .F. ) ;
#41610 = CARTESIAN_POINT ( 'NONE',  ( 3.774488552245651718, -279.9382868265000752, -205.3153579709764358 ) ) ;
#41611 = CARTESIAN_POINT ( 'NONE',  ( -108.2781457802385745, -286.8630330687701644, -246.3649136130257773 ) ) ;
#41612 = CARTESIAN_POINT ( 'NONE',  ( 11.71330621739024913, -285.2922024623816242, -211.7069721845812182 ) ) ;
#41613 = CARTESIAN_POINT ( 'NONE',  ( -90.52770824079732392, -271.2964016181175566, -217.7181985470718075 ) ) ;
#41614 = CARTESIAN_POINT ( 'NONE',  ( -35.37634163115831853, -275.9971320135749693, -195.9343108153315711 ) ) ;
#41615 = CARTESIAN_POINT ( 'NONE',  ( -110.0748593996025591, -288.4262529255840377, -286.2698117605277162 ) ) ;
#41616 = CARTESIAN_POINT ( 'NONE',  ( 0.4517791500610099931, -278.4149966243742824, -336.0861389971571498 ) ) ;
#41617 = ORIENTED_EDGE ( 'NONE', *, *, #90766, .T. ) ;
#41619 = CARTESIAN_POINT ( 'NONE',  ( 35.45467088625077423, -280.8057350154866185, -263.1495266674969571 ) ) ;
#41618 = CARTESIAN_POINT ( 'NONE',  ( -103.3698487317648187, -278.9742419918925407, -239.1089849171963237 ) ) ;
#41620 = CARTESIAN_POINT ( 'NONE',  ( -20.18183872319299610, -277.9164709957369723, -345.1620687583575204 ) ) ;
#41621 = CARTESIAN_POINT ( 'NONE',  ( -113.3740930089107195, -277.2244783269777031, -280.1136452566762500 ) ) ;
#41622 = CARTESIAN_POINT ( 'NONE',  ( 201.0614859237756775, 294.6279256560665090, -68.41024071426262765 ) ) ;
#41623 = CARTESIAN_POINT ( 'NONE',  ( -13.14803923713535561, -275.3002158549089131, -197.5086164110182096 ) ) ;
#41624 = EDGE_CURVE ( 'NONE', #72504, #33370, #86650, .T. ) ;
#41625 = CARTESIAN_POINT ( 'NONE',  ( -35.50789907027257186, -299.4999520329629945, -193.9499080600656669 ) ) ;
#41626 = CARTESIAN_POINT ( 'NONE',  ( 21.27581636871892101, -289.4090924074130839, -223.5744983911110353 ) ) ;
#41627 = ORIENTED_EDGE ( 'NONE', *, *, #82958, .T. ) ;
#41628 = CARTESIAN_POINT ( 'NONE',  ( 82.63923273776656231, -300.3135941503064714, -192.9728626493033801 ) ) ;
#41629 = CARTESIAN_POINT ( 'NONE',  ( 23.78423427710064431, -288.0715849740251997, -229.7989241006791303 ) ) ;
#41630 = CARTESIAN_POINT ( 'NONE',  ( 25.50647157808987231, -288.7413759433204063, -227.6286188763099005 ) ) ;
#41631 = ADVANCED_FACE ( 'NONE', ( #53899 ), #70045, .T. ) ;
#41632 = CARTESIAN_POINT ( 'NONE',  ( 23.58988187244508694, -287.4606736498562327, -310.7725284359871125 ) ) ;
#41633 = CARTESIAN_POINT ( 'NONE',  ( -106.6209770983899148, -284.4895264130075248, -236.8960812199129293 ) ) ;
#41634 = CARTESIAN_POINT ( 'NONE',  ( -8.920632395264135539, -278.8301062886173440, -202.2532379311441844 ) ) ;
#41635 = CARTESIAN_POINT ( 'NONE',  ( -84.44968318218414538, -287.2565238148146136, -212.9209421357792849 ) ) ;
#41636 = CARTESIAN_POINT ( 'NONE',  ( 33.78783447648743277, -279.7793127673329536, -251.0437210441863272 ) ) ;
#41637 = CARTESIAN_POINT ( 'NONE',  ( -109.3739208729831347, -280.0592136932062317, -255.7169522442660536 ) ) ;
#41638 = CARTESIAN_POINT ( 'NONE',  ( -51.28649568409007031, -277.7276336572794548, -342.0795334584285570 ) ) ;
#41639 = CARTESIAN_POINT ( 'NONE',  ( 12.14755339502901421, -287.1761069587424799, -328.8318157996811237 ) ) ;
#41640 = CIRCLE ( 'NONE', #841, 0.4999999999999998335 ) ;
#41641 = CARTESIAN_POINT ( 'NONE',  ( 11.39808363886833398, -283.1992571258298881, -329.8319329765034809 ) ) ;
#41642 = CARTESIAN_POINT ( 'NONE',  ( -96.21917046797801731, -284.3768480404935417, -319.9089714645272693 ) ) ;
#41643 = CARTESIAN_POINT ( 'NONE',  ( 34.06475212451169199, -281.5179630639535162, -255.1319065323168900 ) ) ;
#41644 = ORIENTED_EDGE ( 'NONE', *, *, #46824, .T. ) ;
#41645 = ORIENTED_EDGE ( 'NONE', *, *, #25097, .F. ) ;
#41646 = CARTESIAN_POINT ( 'NONE',  ( 194.8949733755876252, 19.89707320078522557, -13.96765070539848530 ) ) ;
#41647 = CARTESIAN_POINT ( 'NONE',  ( -103.5423949123394749, -292.8980245138036480, -233.5131399065905669 ) ) ;
#41648 = CARTESIAN_POINT ( 'NONE',  ( 3.889958749570145091, -291.2793407527752834, -205.8526114901084156 ) ) ;
#41649 = CARTESIAN_POINT ( 'NONE',  ( 34.60689690629411075, -274.4311759228303913, -256.6933517624825640 ) ) ;
#41650 = CARTESIAN_POINT ( 'NONE',  ( 1.710513562695761713, -293.8927571321402752, -336.6048904627697311 ) ) ;
#41651 = CARTESIAN_POINT ( 'NONE',  ( -71.51127199249741295, -287.9918936810018977, -335.6681638812212896 ) ) ;
#41652 = CARTESIAN_POINT ( 'NONE',  ( 2.808777516213296632, -290.8384062685925642, -208.1239280299051586 ) ) ;
#41653 = CARTESIAN_POINT ( 'NONE',  ( -94.40335296259695497, -291.1077805326222006, -316.5249380365361276 ) ) ;
#41654 = CARTESIAN_POINT ( 'NONE',  ( 189.9243309297870610, 250.0000000000000568, 20.22542485937349355 ) ) ;
#41655 = CARTESIAN_POINT ( 'NONE',  ( -112.3885822208017515, -292.5411397846005457, -271.2316422452453821 ) ) ;
#41656 = CARTESIAN_POINT ( 'NONE',  ( -39.14163571056497659, -290.0294877915744678, -195.2032754166945949 ) ) ;
#41657 = CARTESIAN_POINT ( 'NONE',  ( 8.939620280993420209, -294.6867878811980290, -211.2785924188806064 ) ) ;
#41658 = CARTESIAN_POINT ( 'NONE',  ( -6.929696902326653252, -287.4025858886413971, -203.7251408791647975 ) ) ;
#41659 = CARTESIAN_POINT ( 'NONE',  ( 37.41658326311324601, -295.6587166311339843, -278.6663784264282526 ) ) ;
#41660 = DIRECTION ( 'NONE',  ( 0.000000000000000000, 1.000000000000000000, 0.000000000000000000 ) ) ;
#41661 = CARTESIAN_POINT ( 'NONE',  ( 37.91014550762238855, -277.4701774622000130, -265.5197760581237958 ) ) ;
#41662 = CARTESIAN_POINT ( 'NONE',  ( -103.7051730876373767, -296.2555370279769136, -231.5258277155712392 ) ) ;
#41663 = CARTESIAN_POINT ( 'NONE',  ( -40.57212219243000106, -275.3331529661656418, -344.3165599633954344 ) ) ;
#41664 = CARTESIAN_POINT ( 'NONE',  ( -111.0440694423989214, -276.7718420363114546, -259.5508040766388831 ) ) ;
#41665 = CARTESIAN_POINT ( 'NONE',  ( -103.5699316611706706, -274.1827799328040669, -238.7232948651893878 ) ) ;
#41666 = CARTESIAN_POINT ( 'NONE',  ( -84.84472907284245480, -297.1471853337678795, -326.6315422115357592 ) ) ;
#41667 = CARTESIAN_POINT ( 'NONE',  ( 175.2296996224750103, 128.0000000000000568, 0.000000000000000000 ) ) ;
#41668 = CARTESIAN_POINT ( 'NONE',  ( -108.4535525103710398, -297.1279464807188901, -287.6100276268018092 ) ) ;
#41669 = DIRECTION ( 'NONE',  ( 0.000000000000000000, 0.000000000000000000, 1.000000000000000000 ) ) ;
#41671 = CARTESIAN_POINT ( 'NONE',  ( -66.81933986555078775, -297.6548354787283870, -203.5636919474551689 ) ) ;
#41670 = CARTESIAN_POINT ( 'NONE',  ( 37.99618899985917864, -285.5516144945797237, -268.7457971012664188 ) ) ;
#41672 = CARTESIAN_POINT ( 'NONE',  ( 7.543931294060559622, -286.6455329396953289, -207.7312399161872349 ) ) ;
#41673 = CARTESIAN_POINT ( 'NONE',  ( -98.14551663014650273, -289.5882481465149567, -317.5695938150835786 ) ) ;
#41674 = CARTESIAN_POINT ( 'NONE',  ( -82.01617823731210422, -299.4268715949281159, -209.6118577671483365 ) ) ;
#41675 = CARTESIAN_POINT ( 'NONE',  ( 17.48543136529931274, -292.2661600562431659, -321.2925825132865043 ) ) ;
#41676 = CARTESIAN_POINT ( 'NONE',  ( 23.62543954828221260, -280.1239585154711449, -223.5724660165973603 ) ) ;
#41677 = CARTESIAN_POINT ( 'NONE',  ( -37.30987171927208834, -295.5523547857347353, -195.3611179825600175 ) ) ;
#41678 = CARTESIAN_POINT ( 'NONE',  ( 222.8344101925596306, 0.000000000000000000, -21.49999999999998579 ) ) ;
#41679 = CARTESIAN_POINT ( 'NONE',  ( -73.75522210830541781, -288.3420212531743800, -334.1030439030342905 ) ) ;
#41680 = DIRECTION ( 'NONE',  ( 0.000000000000000000, 0.000000000000000000, -1.000000000000000000 ) ) ;
#41681 = CARTESIAN_POINT ( 'NONE',  ( -79.31421646316049134, -287.6181027514745097, -332.5791718530181242 ) ) ;
#41682 = CARTESIAN_POINT ( 'NONE',  ( -105.0240918310044407, -274.4618434606221626, -241.0803634061171294 ) ) ;
#41683 = CARTESIAN_POINT ( 'NONE',  ( 20.60729127639539016, -282.2997550093975292, -220.5364024447617339 ) ) ;
#41685 = CARTESIAN_POINT ( 'NONE',  ( 33.94041483488990707, -281.7598360453405917, -286.1046908428020288 ) ) ;
#41684 = CARTESIAN_POINT ( 'NONE',  ( -83.20455907463373535, -293.6964141724263300, -330.2182697912767253 ) ) ;
#41686 = CARTESIAN_POINT ( 'NONE',  ( -77.08040976879073014, -295.7354882012526218, -336.3764263417740494 ) ) ;
#41687 = CARTESIAN_POINT ( 'NONE',  ( 95.96543556739594294, -301.2707763474030571, -196.6326178096987860 ) ) ;
#41688 = EDGE_CURVE ( 'NONE', #86306, #72022, #61491, .T. ) ;
#41689 = CARTESIAN_POINT ( 'NONE',  ( 36.46215972292451113, -283.7245304312448866, -283.7739075632489971 ) ) ;
#41690 = CARTESIAN_POINT ( 'NONE',  ( -41.87095832627058201, -297.0524230194331494, -197.2660137102401734 ) ) ;
#41691 = VERTEX_POINT ( 'NONE', #76616 ) ;
#41692 = CARTESIAN_POINT ( 'NONE',  ( 221.4259212729440094, 36.93618551656547311, -7.000000000000000888 ) ) ;
#41693 = CARTESIAN_POINT ( 'NONE',  ( -112.0361296218977145, -286.5244943658366310, -270.9468144176681221 ) ) ;
#41694 = CARTESIAN_POINT ( 'NONE',  ( 186.2362647323748206, 250.5000000000000568, 22.80382896336985965 ) ) ;
#41695 = CARTESIAN_POINT ( 'NONE',  ( 13.79469577742117181, -273.9094976428776818, -334.5364918783848793 ) ) ;
#41696 = CARTESIAN_POINT ( 'NONE',  ( 31.70568146570080970, -275.1844804328716805, -304.1960407099032864 ) ) ;
#41697 = CARTESIAN_POINT ( 'NONE',  ( -7.268306688921768455, -292.2912716140305065, -203.8435187205360251 ) ) ;
#41698 = CARTESIAN_POINT ( 'NONE',  ( -59.13487383315286650, -284.8593530868857897, -340.8119567251113153 ) ) ;
#41699 = PRESENTATION_LAYER_ASSIGNMENT (  '', '', ( #22120 ) ) ;
#41700 = CARTESIAN_POINT ( 'NONE',  ( 18.04901839466556979, -277.8412556586205824, -319.1480958424884307 ) ) ;
#41701 = CARTESIAN_POINT ( 'NONE',  ( -111.6419001824270225, -285.7519484915279122, -288.2514335980770852 ) ) ;
#41702 = CARTESIAN_POINT ( 'NONE',  ( -89.18557169189418232, -282.5961383796832251, -322.3876777027833782 ) ) ;
#41703 = CARTESIAN_POINT ( 'NONE',  ( -70.65085845100729500, -281.6130930223119435, -203.1494154472848095 ) ) ;
#41704 = CARTESIAN_POINT ( 'NONE',  ( 37.63442460701440240, -275.4988421891508779, -252.7657895295491528 ) ) ;
#41705 = CARTESIAN_POINT ( 'NONE',  ( 23.51674089509399224, -276.0155820897891772, -317.5550585629911211 ) ) ;
#41706 = CARTESIAN_POINT ( 'NONE',  ( -96.73884558491587882, -297.8539093632993513, -315.2518449888248711 ) ) ;
#41707 = DIRECTION ( 'NONE',  ( -1.000000000000000000, 0.000000000000000000, 0.000000000000000000 ) ) ;
#41708 = CARTESIAN_POINT ( 'NONE',  ( 195.5881128153457098, -0.9999999999999991118, 22.50000000000000000 ) ) ;
#41709 = EDGE_CURVE ( 'NONE', #6120, #24267, #47234, .T. ) ;
#41710 = CARTESIAN_POINT ( 'NONE',  ( -102.0727733461083346, -294.1692663981784222, -309.7336164939565037 ) ) ;
#41711 = CARTESIAN_POINT ( 'NONE',  ( 35.41472029519250242, -275.1477191736769896, -277.0313300294994860 ) ) ;
#41712 = CARTESIAN_POINT ( 'NONE',  ( -60.31413826022249225, -287.5103150477829672, -200.0031681948654239 ) ) ;
#41713 = CARTESIAN_POINT ( 'NONE',  ( -25.00069408847846830, -296.4177634806480341, -345.7168059011630703 ) ) ;
#41714 = CARTESIAN_POINT ( 'NONE',  ( 19.24677467267338926, -295.4634734750544567, -322.0693317182562510 ) ) ;
#41715 = CARTESIAN_POINT ( 'NONE',  ( -96.38164189535217474, -291.9200719071964727, -316.3634780867970449 ) ) ;
#41716 = CARTESIAN_POINT ( 'NONE',  ( -108.0035765230149991, -276.2304972260376417, -295.1543290588861623 ) ) ;
#41717 = CARTESIAN_POINT ( 'NONE',  ( -111.6030148488140981, -280.3965702138244751, -276.2160208940152870 ) ) ;
#41718 = CARTESIAN_POINT ( 'NONE',  ( -106.3049748690865783, -294.2638691184287723, -298.3857666423747332 ) ) ;
#41719 = CARTESIAN_POINT ( 'NONE',  ( -19.19097222564238336, -284.6815656523039593, -343.9737227675237818 ) ) ;
#41720 = CARTESIAN_POINT ( 'NONE',  ( -96.00507022231452936, -284.0870177650495521, -226.3970976523370666 ) ) ;
#41721 = CARTESIAN_POINT ( 'NONE',  ( 7.521071455173375497, -59.59353953422439076, -353.8445329526322780 ) ) ;
#41722 = EDGE_LOOP ( 'NONE', ( #88032, #39152, #78459, #29086 ) ) ;
#41723 = CARTESIAN_POINT ( 'NONE',  ( -105.2351610430884534, -283.8577569231067059, -297.3793561735712387 ) ) ;
#41724 = VERTEX_POINT ( 'NONE', #3234 ) ;
#41725 = CARTESIAN_POINT ( 'NONE',  ( 35.87648806123711864, -282.3440265301103977, -247.5446890760673000 ) ) ;
#41726 = CARTESIAN_POINT ( 'NONE',  ( -103.6888315564941649, -283.8486317876976273, -231.9664155074464134 ) ) ;
#41727 = CARTESIAN_POINT ( 'NONE',  ( -107.3565628231119859, -279.0887027739138944, -301.9664277389737777 ) ) ;
#41728 = ADVANCED_FACE ( 'NONE', ( #10796 ), #3716, .T. ) ;
#41729 =( LENGTH_UNIT ( ) NAMED_UNIT ( * ) SI_UNIT ( .MILLI., .METRE. ) );
#41730 = CARTESIAN_POINT ( 'NONE',  ( -9.447083545083982514, -278.2142350011095573, -341.3864523252224217 ) ) ;
#41731 = CARTESIAN_POINT ( 'NONE',  ( 3.760469193432061097, -281.2409032959117212, -205.3064978043875044 ) ) ;
#41732 = CARTESIAN_POINT ( 'NONE',  ( -53.35057174420112602, -300.3376638359844719, -200.3683826091709648 ) ) ;
#41733 = CARTESIAN_POINT ( 'NONE',  ( 162.3984126888688877, 219.7162322416178597, -205.2442872645431748 ) ) ;
#41734 = VERTEX_POINT ( 'NONE', #11739 ) ;
#41735 = CARTESIAN_POINT ( 'NONE',  ( 23.76348346342304652, -276.9638032030176760, -227.1395828135516126 ) ) ;
#41736 = CARTESIAN_POINT ( 'NONE',  ( -48.68011135779718046, -154.6331602903188696, -364.9585083841176925 ) ) ;
#41737 = CARTESIAN_POINT ( 'NONE',  ( -69.20298245349890465, -277.6510244092736457, -202.8577440260321794 ) ) ;
#41738 = CARTESIAN_POINT ( 'NONE',  ( 31.26132543115433293, -294.8864756245884564, -237.5647813649045759 ) ) ;
#41739 = CARTESIAN_POINT ( 'NONE',  ( -6.729768481844214278, -293.9878953299498221, -336.7448683241781850 ) ) ;
#41740 = CARTESIAN_POINT ( 'NONE',  ( -100.6335452153688124, -289.4816391902241435, -314.1066234512865094 ) ) ;
#41741 = CARTESIAN_POINT ( 'NONE',  ( 175.2296996224750103, 20.99999999999998934, 0.000000000000000000 ) ) ;
#41743 = CARTESIAN_POINT ( 'NONE',  ( -69.10094620801039866, -284.0271802005248105, -203.7304346851486514 ) ) ;
#41742 = CARTESIAN_POINT ( 'NONE',  ( -58.70412568069531289, -293.8977481573832051, -343.7801090511866278 ) ) ;
#41744 = CARTESIAN_POINT ( 'NONE',  ( -44.44153510163963006, -293.8219487703494224, -196.4145287119885950 ) ) ;
#41745 = CARTESIAN_POINT ( 'NONE',  ( -80.90507619547820184, -284.9723917196544107, -329.6145901829643208 ) ) ;
#41746 = ORIENTED_EDGE ( 'NONE', *, *, #61930, .T. ) ;
#41747 = CARTESIAN_POINT ( 'NONE',  ( -90.63125093652246278, -292.2606380785858846, -215.0329754065286068 ) ) ;
#41748 = CARTESIAN_POINT ( 'NONE',  ( 20.23333590796336523, -282.6779471400249690, -315.3400426842292745 ) ) ;
#41749 = CARTESIAN_POINT ( 'NONE',  ( -50.41493378120410540, -294.0102974119830037, -345.8939175681458096 ) ) ;
#41750 = CARTESIAN_POINT ( 'NONE',  ( 10.13621599041971422, -289.2195304871756321, -330.8440964674711040 ) ) ;
#41751 = EDGE_CURVE ( 'NONE', #86547, #63082, #39854, .T. ) ;
#41752 = CARTESIAN_POINT ( 'NONE',  ( -68.02357214386728401, -289.9366709306814300, -340.9171215045449799 ) ) ;
#41753 = CARTESIAN_POINT ( 'NONE',  ( 22.75110663907214104, -288.2963254169742413, -311.8301617820586671 ) ) ;
#41754 = EDGE_LOOP ( 'NONE', ( #52556, #93444, #4944, #15802 ) ) ;
#41755 = FACE_OUTER_BOUND ( 'NONE', #37677, .T. ) ;
#41756 = CARTESIAN_POINT ( 'NONE',  ( -111.6814052290836230, -298.5993105178982887, -255.6685047828887605 ) ) ;
#41757 = CARTESIAN_POINT ( 'NONE',  ( -57.24517541272127374, -296.4855112107333071, -196.4336717589160060 ) ) ;
#41758 = ADVANCED_FACE ( 'NONE', ( #19777 ), #91259, .F. ) ;
#41759 = CARTESIAN_POINT ( 'NONE',  ( 20.70976343061323277, -279.9843449149510093, -225.6928195841554157 ) ) ;
#41760 = ORIENTED_EDGE ( 'NONE', *, *, #1240, .F. ) ;
#41761 = CARTESIAN_POINT ( 'NONE',  ( 19.30376808285199175, -298.0924932148090534, -193.4691040211189090 ) ) ;
#41762 = CARTESIAN_POINT ( 'NONE',  ( -70.04903514772988160, -293.9710051964875106, -336.3985164054278130 ) ) ;
#41763 = CARTESIAN_POINT ( 'NONE',  ( 35.71099084174209537, -277.4709839282748476, -282.5574158634472042 ) ) ;
#41764 = CARTESIAN_POINT ( 'NONE',  ( -77.20793339934965616, -271.6510381350398120, -207.7388461943276923 ) ) ;
#41765 = CARTESIAN_POINT ( 'NONE',  ( -20.74354049236241337, -296.0395239726513523, -341.9091842634544491 ) ) ;
#41766 = CARTESIAN_POINT ( 'NONE',  ( -5.394424088937386230, -295.7013090630406964, -336.3567863077590800 ) ) ;
#41767 = DIRECTION ( 'NONE',  ( 1.000000000000000000, 0.000000000000000000, 0.000000000000000000 ) ) ;
#41768 = CARTESIAN_POINT ( 'NONE',  ( -69.17495047838239941, -297.0640410419794648, -339.6075056637247371 ) ) ;
#41769 = CARTESIAN_POINT ( 'NONE',  ( -77.20801665719200457, -295.5188283460266234, -206.6374549372561376 ) ) ;
#41770 = CARTESIAN_POINT ( 'NONE',  ( -86.00305685567641945, -292.0081559091677263, -215.7405716127899211 ) ) ;
#41771 = CARTESIAN_POINT ( 'NONE',  ( -34.12021816225008308, -274.8945311294402813, -193.5901542346542215 ) ) ;
#41772 = CARTESIAN_POINT ( 'NONE',  ( -108.6751992140893037, -289.3642052792698678, -252.2293552061949811 ) ) ;
#41773 = CARTESIAN_POINT ( 'NONE',  ( 199.0743954165634761, 275.0000000000000568, -2.725891136377206703 ) ) ;
#41774 = CARTESIAN_POINT ( 'NONE',  ( -32.69259138734448555, -274.6015834248199212, -193.5501087911893023 ) ) ;
#41775 = CARTESIAN_POINT ( 'NONE',  ( -100.1825056089172108, -296.3733661951385443, -307.6510001221028006 ) ) ;
#41776 = CARTESIAN_POINT ( 'NONE',  ( 22.42698246003470430, -282.9062330948988802, -224.4476578473702659 ) ) ;
#41777 = CARTESIAN_POINT ( 'NONE',  ( 3.572488707568652444, -279.2746329902387288, -205.6508138377376724 ) ) ;
#41778 = CARTESIAN_POINT ( 'NONE',  ( -48.48742303607134119, -276.5389311568097241, -346.5009828279039539 ) ) ;
#41779 = CARTESIAN_POINT ( 'NONE',  ( 37.07975229812336693, -280.1596354939910043, -286.7885837395131716 ) ) ;
#41780 = CARTESIAN_POINT ( 'NONE',  ( 24.78017994419907311, -278.9792107219777790, -227.9512250103759641 ) ) ;
#41781 = CARTESIAN_POINT ( 'NONE',  ( -76.86552517544035368, -272.0861116446538404, -208.2866290991796063 ) ) ;
#41782 = CARTESIAN_POINT ( 'NONE',  ( -99.60396546988273769, -281.1180038728288650, -228.5242565469726799 ) ) ;
#41783 = CARTESIAN_POINT ( 'NONE',  ( 180.7287904564219332, 215.0000000000000568, -24.90000000000002345 ) ) ;
#41784 = PLANE ( 'NONE',  #60990 ) ;
#41785 = CARTESIAN_POINT ( 'NONE',  ( -62.48828682775742749, -295.9692418881478488, -198.6560052633979012 ) ) ;
#41786 = CARTESIAN_POINT ( 'NONE',  ( 30.71162955993893462, -291.1470440113635618, -237.8800528281001334 ) ) ;
#41787 = CARTESIAN_POINT ( 'NONE',  ( -74.67889708995357978, -291.5693216877177179, -203.0192014444159270 ) ) ;
#41788 = CARTESIAN_POINT ( 'NONE',  ( 37.48952540902096331, -277.4546810752640909, -262.7402752453760968 ) ) ;
#41789 = CARTESIAN_POINT ( 'NONE',  ( -3.171342694323064926, -272.5032799732290982, -203.5830308869954877 ) ) ;
#41790 = CARTESIAN_POINT ( 'NONE',  ( -57.23711263161519724, -285.8906705383787994, 57.50000000000000711 ) ) ;
#41791 = CARTESIAN_POINT ( 'NONE',  ( 3.782857655889125592, -284.4238637016883331, -333.8113350966390840 ) ) ;
#41792 = DIRECTION ( 'NONE',  ( 0.000000000000000000, 0.000000000000000000, 1.000000000000000000 ) ) ;
#41793 = CARTESIAN_POINT ( 'NONE',  ( 34.12633415019790561, -285.8460164134294246, -293.1478109287773464 ) ) ;
#41794 = CARTESIAN_POINT ( 'NONE',  ( 139.1539576904058606, 276.0000000000000568, 10.50000000000000000 ) ) ;
#41795 = CARTESIAN_POINT ( 'NONE',  ( -50.55768478198633886, -294.0196223028262921, -342.5585435140632740 ) ) ;
#41796 = CARTESIAN_POINT ( 'NONE',  ( -6.481770789091785723, -284.6013712154704081, -202.8302678869715692 ) ) ;
#41797 = CARTESIAN_POINT ( 'NONE',  ( 175.2296996224750103, 275.5000000000000568, 0.000000000000000000 ) ) ;
#41798 = CARTESIAN_POINT ( 'NONE',  ( -50.85592009661865376, -293.2246655496550147, -344.1335146128425322 ) ) ;
#41799 = CARTESIAN_POINT ( 'NONE',  ( -94.82529980900078215, -282.3472038480871902, -320.5442179421402216 ) ) ;
#41800 = CARTESIAN_POINT ( 'NONE',  ( -41.11221562341206948, -281.6040378283707923, -196.6574977922192886 ) ) ;
#41801 = CARTESIAN_POINT ( 'NONE',  ( -1.170669037677460222, -287.7263251712611236, -202.8358247273881432 ) ) ;
#41802 = CARTESIAN_POINT ( 'NONE',  ( 36.55755895016432078, -280.0168397491460723, -288.1047801723910879 ) ) ;
#41803 = CARTESIAN_POINT ( 'NONE',  ( 30.97459740206149803, -287.2071295239269375, -244.4913271381309983 ) ) ;
#41804 = CARTESIAN_POINT ( 'NONE',  ( -14.14017566206672605, -281.7842070762887943, -200.4712716021699066 ) ) ;
#41805 = CARTESIAN_POINT ( 'NONE',  ( -27.54685636486275868, -280.9824608197324096, -197.8069680105778616 ) ) ;
#41806 = CARTESIAN_POINT ( 'NONE',  ( 15.13529776561737528, -288.7683233690289626, -216.2818105420631980 ) ) ;
#41807 = ORIENTED_EDGE ( 'NONE', *, *, #69089, .F. ) ;
#41808 = CARTESIAN_POINT ( 'NONE',  ( 53.58966561814242624, -298.9944938268030228, -193.3635553575743984 ) ) ;
#41809 = CARTESIAN_POINT ( 'NONE',  ( -105.0588228997770557, -292.9465989243751665, -238.9566902197576042 ) ) ;
#41810 = CARTESIAN_POINT ( 'NONE',  ( 209.2568086740250237, 34.98978593258875236, 12.09245862095555601 ) ) ;
#41811 = CARTESIAN_POINT ( 'NONE',  ( -37.37352853689063181, -300.5519495502701375, -190.3611179825600175 ) ) ;
#41812 = ORIENTED_EDGE ( 'NONE', *, *, #5059, .F. ) ;
#41813 = CARTESIAN_POINT ( 'NONE',  ( -2.137042854149974414, -272.5169823304725014, -203.9483139813929427 ) ) ;
#41814 = CARTESIAN_POINT ( 'NONE',  ( -69.21208553357716653, -293.8643020225778741, -339.5904229530310658 ) ) ;
#41815 = CARTESIAN_POINT ( 'NONE',  ( -71.68839007505155791, -297.0930535614419910, -205.8620784804440973 ) ) ;
#41816 = CARTESIAN_POINT ( 'NONE',  ( 21.74085038285266336, -289.6846729316810070, -314.4272254184750182 ) ) ;
#41817 = CARTESIAN_POINT ( 'NONE',  ( 14.02243007738041314, -282.5447841570524474, -217.0008812081251222 ) ) ;
#41818 = CARTESIAN_POINT ( 'NONE',  ( -86.98771432678967130, -291.1524935598838510, -328.5157067783189291 ) ) ;
#41819 = CARTESIAN_POINT ( 'NONE',  ( -67.84179295458659453, -290.7593647584248515, -340.5255150182598527 ) ) ;
#41820 = CARTESIAN_POINT ( 'NONE',  ( -19.36036283374808420, -288.2836563955695510, -197.5485355892342056 ) ) ;
#41821 = CARTESIAN_POINT ( 'NONE',  ( -98.57764851473837098, -279.3413593344394599, -223.6581797274827466 ) ) ;
#41822 = CARTESIAN_POINT ( 'NONE',  ( 22.86645927910179665, -292.2518661865717036, -316.0151620746462413 ) ) ;
#41823 = CARTESIAN_POINT ( 'NONE',  ( 20.13010064881657257, -280.6905442306977534, -219.0968566879743094 ) ) ;
#41824 = CARTESIAN_POINT ( 'NONE',  ( 33.28044864426563265, -277.7110339564296737, -293.2385650201309772 ) ) ;
#41825 = CARTESIAN_POINT ( 'NONE',  ( -92.08974858914540107, -281.6948066931272479, -226.7417163044926838 ) ) ;
#41826 = CARTESIAN_POINT ( 'NONE',  ( 32.08471656633341951, -274.1914893272100926, -301.2471451849967252 ) ) ;
#41827 = DIRECTION ( 'NONE',  ( -1.000000000000000000, 0.000000000000000000, 0.000000000000000000 ) ) ;
#41828 = CARTESIAN_POINT ( 'NONE',  ( 33.17462298238724827, -280.8069214334814774, -251.1968409042158896 ) ) ;
#41829 = CARTESIAN_POINT ( 'NONE',  ( -86.82692729869314974, -278.9275873386572471, -328.9046151632535384 ) ) ;
#41830 = CARTESIAN_POINT ( 'NONE',  ( -66.02092967001290447, -274.9839746959575564, -202.6946915088247749 ) ) ;
#41831 = CARTESIAN_POINT ( 'NONE',  ( -37.96846180250446423, -285.1032326207889014, -193.5989698632314173 ) ) ;
#41832 = CARTESIAN_POINT ( 'NONE',  ( -101.1665947577201621, -291.8035560310515280, -307.9367605296737906 ) ) ;
#41833 = CARTESIAN_POINT ( 'NONE',  ( -80.81091470282231626, -275.0735625324317652, -207.7122821438863980 ) ) ;
#41834 = CARTESIAN_POINT ( 'NONE',  ( -100.8088841455731597, -274.4348457224380127, -227.5442398412263287 ) ) ;
#41835 = CARTESIAN_POINT ( 'NONE',  ( 82.64890176555634582, -299.5541904835127980, -195.3611179825600175 ) ) ;
#41836 = CARTESIAN_POINT ( 'NONE',  ( 5.395067839312406299, -276.2891231396670264, -329.6060420001832654 ) ) ;
#41837 = CARTESIAN_POINT ( 'NONE',  ( -105.5986415013631472, -298.1477255315018624, -301.1637126802027637 ) ) ;
#41838 = CARTESIAN_POINT ( 'NONE',  ( -80.34244608713942171, -283.4684023586116268, -209.0524005957549889 ) ) ;
#41839 = CARTESIAN_POINT ( 'NONE',  ( 6.487675469906672099, -292.2968144910672663, -207.0781808972672309 ) ) ;
#41840 = CARTESIAN_POINT ( 'NONE',  ( 35.77061901868826510, -273.7663918847093782, -285.4088950623718688 ) ) ;
#41841 = CARTESIAN_POINT ( 'NONE',  ( 23.51571138032539210, -289.7692768306808375, -316.2175884309407365 ) ) ;
#41842 = CARTESIAN_POINT ( 'NONE',  ( -109.5789663791787660, -289.6403510633914493, -257.5814579526740431 ) ) ;
#41843 = ORIENTED_EDGE ( 'NONE', *, *, #77906, .T. ) ;
#41844 = CARTESIAN_POINT ( 'NONE',  ( -104.0864034529987094, -289.6128653067518712, -233.1623159914257144 ) ) ;
#41845 = CARTESIAN_POINT ( 'NONE',  ( -109.4406586793314489, -290.0652698400853069, -282.0081835085784974 ) ) ;
#41846 = VERTEX_POINT ( 'NONE', #89867 ) ;
#41847 = CARTESIAN_POINT ( 'NONE',  ( 39.04081402945485735, -288.7180930021364702, -277.2316376238222233 ) ) ;
#41848 = CARTESIAN_POINT ( 'NONE',  ( -107.6398201698862209, -279.1470379476784842, -250.5597196312261872 ) ) ;
#41849 = CARTESIAN_POINT ( 'NONE',  ( -92.48433814451546198, -294.7394129464480557, -323.6601046720264208 ) ) ;
#41850 = CARTESIAN_POINT ( 'NONE',  ( -105.6897389913451235, -284.7474459712592534, -305.7172865382960367 ) ) ;
#41851 = CARTESIAN_POINT ( 'NONE',  ( -105.7634070545326068, -284.4293651346633283, -305.7508317293314235 ) ) ;
#41852 = CARTESIAN_POINT ( 'NONE',  ( 21.02936191867633653, -282.5015535409899599, -314.2555394901853560 ) ) ;
#41853 = CARTESIAN_POINT ( 'NONE',  ( -12.84209639897599331, -91.63111746082969944, -360.1199121724810652 ) ) ;
#41854 = CARTESIAN_POINT ( 'NONE',  ( -40.89730568847058834, -138.9793244955967566, -363.4251286451764145 ) ) ;
#41855 = CARTESIAN_POINT ( 'NONE',  ( 192.0717789903930282, 276.6821163107279631, -124.1503466236808606 ) ) ;
#41856 = CARTESIAN_POINT ( 'NONE',  ( 29.23723054607156868, -274.3398496504575519, -239.9095363816517192 ) ) ;
#41857 = CARTESIAN_POINT ( 'NONE',  ( 0.7849195434376035063, -273.4940745938593523, -207.7465274629228418 ) ) ;
#41858 = CARTESIAN_POINT ( 'NONE',  ( -22.11586145835835282, -294.3697736302283943, -345.7779645081329818 ) ) ;
#41859 = CARTESIAN_POINT ( 'NONE',  ( -110.4703370556568274, -271.6448334738088306, -283.7149836808490591 ) ) ;
#41860 = CARTESIAN_POINT ( 'NONE',  ( 39.21375012171231589, -274.2473265192939493, -271.1831682273236765 ) ) ;
#41861 = CARTESIAN_POINT ( 'NONE',  ( -110.9643546477779239, -298.5410764386292044, -260.4550081734931268 ) ) ;
#41862 = CARTESIAN_POINT ( 'NONE',  ( -98.56523825880174172, -292.1897704973823124, -229.9463785342367430 ) ) ;
#41863 = VERTEX_POINT ( 'NONE', #83230 ) ;
#41864 = CARTESIAN_POINT ( 'NONE',  ( -112.3726326459767648, -297.2898888310659231, -286.5839222873647714 ) ) ;
#41865 = CARTESIAN_POINT ( 'NONE',  ( 16.06022524577605992, -288.7617109895744534, -320.2971887779788176 ) ) ;
#41866 = CARTESIAN_POINT ( 'NONE',  ( -99.87112668147683792, -296.7611718172383348, -315.1075192663511189 ) ) ;
#41867 = CARTESIAN_POINT ( 'NONE',  ( -11.07232150900850698, -295.2112240252720881, -342.7325570573085542 ) ) ;
#41868 = CARTESIAN_POINT ( 'NONE',  ( 27.15906500562259751, -294.1858136088330298, -304.6546838007758993 ) ) ;
#41869 = EDGE_LOOP ( 'NONE', ( #10596, #54566, #56686, #62704 ) ) ;
#41870 = CARTESIAN_POINT ( 'NONE',  ( 30.57194676240640518, -277.9070289200757884, -303.6021289741994451 ) ) ;
#41871 = EDGE_CURVE ( 'NONE', #13111, #30328, #48944, .T. ) ;
#41872 = ORIENTED_EDGE ( 'NONE', *, *, #27827, .T. ) ;
#41873 = CARTESIAN_POINT ( 'NONE',  ( -38.16295524897140012, -279.5497740893025025, -193.4270394245857858 ) ) ;
#41874 = CARTESIAN_POINT ( 'NONE',  ( 5.304060844957506404, -275.5860567421741507, -210.7606646313418821 ) ) ;
#41875 = CARTESIAN_POINT ( 'NONE',  ( -8.101517869821336149, -276.1899073587616726, -200.1697926859102381 ) ) ;
#41876 = CARTESIAN_POINT ( 'NONE',  ( -112.0823112359125133, -276.7000599708243840, -260.3606039124429117 ) ) ;
#41877 = CARTESIAN_POINT ( 'NONE',  ( -40.53070915468340019, -298.6624442500717009, -197.3162103618080891 ) ) ;
#41878 = CARTESIAN_POINT ( 'NONE',  ( -93.54406556422443941, -294.4569962302094837, -317.8850560523690660 ) ) ;
#41879 = CARTESIAN_POINT ( 'NONE',  ( 151.7498149058220918, 20.88232504567557513, -8.615841630442520938 ) ) ;
#41880 = CARTESIAN_POINT ( 'NONE',  ( -99.38196549910016131, -279.6495326459144621, -224.8357777372608837 ) ) ;
#41881 = CARTESIAN_POINT ( 'NONE',  ( 32.89843655600366645, -275.9822301287650816, -290.2896039483050572 ) ) ;
#41882 = CARTESIAN_POINT ( 'NONE',  ( -32.32194196038565792, -284.7990067571389545, -194.0060404334572866 ) ) ;
#41883 = CARTESIAN_POINT ( 'NONE',  ( -107.3102321367805416, -274.9051788823219908, -243.2105324511977642 ) ) ;
#41884 = CARTESIAN_POINT ( 'NONE',  ( 154.1407330040854333, 250.5000000000000568, 13.42592592592592915 ) ) ;
#41885 = CARTESIAN_POINT ( 'NONE',  ( 33.86984322072535747, -286.5277573782993272, -253.5284509875894230 ) ) ;
#41886 = CARTESIAN_POINT ( 'NONE',  ( -90.18153463057848285, -277.5326517656418446, -218.4625902907441457 ) ) ;
#41888 = CARTESIAN_POINT ( 'NONE',  ( -81.49962851721817003, -281.7375843010298695, -330.3534847119999540 ) ) ;
#41887 = CARTESIAN_POINT ( 'NONE',  ( -81.62812457132237398, -278.0109564714315411, -211.5256579711591769 ) ) ;
#41889 = CARTESIAN_POINT ( 'NONE',  ( 20.66213241999287575, -288.8966279077454828, -222.7960340271066286 ) ) ;
#41890 = CARTESIAN_POINT ( 'NONE',  ( -70.61918831324051382, -278.7062861809214382, -335.7808343228430772 ) ) ;
#41891 = CARTESIAN_POINT ( 'NONE',  ( 175.2296996224750103, 246.0000000000001137, 0.000000000000000000 ) ) ;
#41892 = CARTESIAN_POINT ( 'NONE',  ( -101.5180298370174796, -293.0735131249141432, -231.4485713819197485 ) ) ;
#41893 = CARTESIAN_POINT ( 'NONE',  ( -23.15042539779668118, -275.1130522489181089, -345.0643143919090789 ) ) ;
#41894 = CARTESIAN_POINT ( 'NONE',  ( 35.45627300659815972, -276.2912953246813572, -277.0205305308269317 ) ) ;
#41895 = CARTESIAN_POINT ( 'NONE',  ( 37.80664170710721095, -283.5106728994605305, -267.1106326446460457 ) ) ;
#41896 = CARTESIAN_POINT ( 'NONE',  ( 29.33919985515026596, -212.1443419142231051, 25.50000000000000000 ) ) ;
#41897 = CARTESIAN_POINT ( 'NONE',  ( 33.72658272043302929, -289.8043227270357534, -296.1769489249382445 ) ) ;
#41898 = CARTESIAN_POINT ( 'NONE',  ( -112.3908556221205544, -294.5593570887893975, -269.7871270381273803 ) ) ;
#41899 = DIRECTION ( 'NONE',  ( -0.6632250457539263788, -5.193207171581228641E-15, 0.7484200282493129741 ) ) ;
#41900 = CARTESIAN_POINT ( 'NONE',  ( 5.477575510487311838, -273.3299939084214998, -210.5675373881622932 ) ) ;
#41901 = CARTESIAN_POINT ( 'NONE',  ( 36.87585445388072714, -291.7332972146494967, -273.5655249357238858 ) ) ;
#41902 = CARTESIAN_POINT ( 'NONE',  ( 24.80950920047307307, -22.49099280560490399, -345.4124233396505019 ) ) ;
#41903 = CYLINDRICAL_SURFACE ( 'NONE', #8105, 4.000000000000003553 ) ;
#41904 = CARTESIAN_POINT ( 'NONE',  ( -47.63056831016412218, -290.4036346126384274, -194.6979755647244303 ) ) ;
#41905 = CARTESIAN_POINT ( 'NONE',  ( -85.36711489528526897, -285.3292034701503326, -326.3968204372601463 ) ) ;
#41906 = CARTESIAN_POINT ( 'NONE',  ( 15.60932666036774386, -285.0288925818903749, -215.8619182235494804 ) ) ;
#41907 = CARTESIAN_POINT ( 'NONE',  ( -75.03740207644374038, -286.9645654988524370, -207.1597811948694527 ) ) ;
#41908 = CARTESIAN_POINT ( 'NONE',  ( -94.25409117056919683, -286.0039061796629198, -224.3675546153488085 ) ) ;
#41909 = CARTESIAN_POINT ( 'NONE',  ( -80.99843655355134331, -293.4423891886222577, -208.9404686464075098 ) ) ;
#41910 = CARTESIAN_POINT ( 'NONE',  ( 0.3078932788897342787, -274.6350367119741804, -335.9324573039849042 ) ) ;
#41911 = CARTESIAN_POINT ( 'NONE',  ( -11.86917589862481570, -277.0628490104348884, -343.0592690511407454 ) ) ;
#41912 = CARTESIAN_POINT ( 'NONE',  ( -98.03308049333863039, -289.2420431318808483, -225.3297805556749438 ) ) ;
#41913 = CARTESIAN_POINT ( 'NONE',  ( -54.13124844823479975, -277.2618680714534207, -345.5630208357262632 ) ) ;
#41914 = CARTESIAN_POINT ( 'NONE',  ( -31.44788545383180889, -296.9573954717786251, -344.8241182409000203 ) ) ;
#41915 = CARTESIAN_POINT ( 'NONE',  ( -48.18343439339133027, -254.9503577894309387, -483.2618064832606706 ) ) ;
#41916 = CARTESIAN_POINT ( 'NONE',  ( 208.0393982316568326, 37.47427918878999265, 11.99999999999999822 ) ) ;
#41917 = CARTESIAN_POINT ( 'NONE',  ( -109.9053897566342499, -283.3906862479408915, -258.6301455001369618 ) ) ;
#41918 = EDGE_CURVE ( 'NONE', #46489, #27188, #74627, .T. ) ;
#41919 = CARTESIAN_POINT ( 'NONE',  ( -85.50047368505818213, -277.3865062857793191, -212.7979408751504593 ) ) ;
#41920 = ADVANCED_FACE ( 'NONE', ( #62900 ), #39656, .F. ) ;
#41921 = CARTESIAN_POINT ( 'NONE',  ( 203.5977283565847813, 62.01285785379744198, 7.000000000000000000 ) ) ;
#41922 = CARTESIAN_POINT ( 'NONE',  ( -38.32884969992191770, -272.5198731679579964, -194.0608342937703696 ) ) ;
#41923 = CARTESIAN_POINT ( 'NONE',  ( -21.63920055035339018, -276.1942183734960281, -341.8087288914282453 ) ) ;
#41924 = CARTESIAN_POINT ( 'NONE',  ( 31.23782842602319221, -295.4312339739874460, -297.4740760878866013 ) ) ;
#41925 = CARTESIAN_POINT ( 'NONE',  ( 30.45500933927811005, -280.0064373228339036, -234.3995908357573512 ) ) ;
#41926 = CARTESIAN_POINT ( 'NONE',  ( -94.95112746176029361, -296.8578235159841370, -315.5779547936736549 ) ) ;
#41927 = CARTESIAN_POINT ( 'NONE',  ( 1.533372733041707958, -295.8590270837037224, -336.2551767639329796 ) ) ;
#41928 = CARTESIAN_POINT ( 'NONE',  ( -96.88150751432041830, -296.9752630237763356, -228.1235595667913856 ) ) ;
#41929 = CARTESIAN_POINT ( 'NONE',  ( -106.5584265348968529, -292.9309371318239528, -241.3460153535657184 ) ) ;
#41930 = CARTESIAN_POINT ( 'NONE',  ( -93.92117932652872980, -285.4306092939054338, -218.0549869248505956 ) ) ;
#41931 = CARTESIAN_POINT ( 'NONE',  ( 21.80912381269400058, -273.0470448052685697, -222.9962066773518359 ) ) ;
#41932 = CARTESIAN_POINT ( 'NONE',  ( -26.61900576794774054, -286.0181514389761901, -194.0578724827441874 ) ) ;
#41933 = CARTESIAN_POINT ( 'NONE',  ( -39.77965525347264020, -282.0013032815086831, -195.7433354173287512 ) ) ;
#41934 = CARTESIAN_POINT ( 'NONE',  ( 2.585298234370239090, -285.6608861773589751, -208.9669549900454513 ) ) ;
#41935 = CARTESIAN_POINT ( 'NONE',  ( -54.08068690888060104, -287.2667779909892261, -343.5225992571189408 ) ) ;
#41936 = CARTESIAN_POINT ( 'NONE',  ( -92.83893396777953910, -239.1568807800618686, -338.3566629249717153 ) ) ;
#41937 = CARTESIAN_POINT ( 'NONE',  ( -22.44116389277090917, -285.7556263887379373, -198.7832360582742410 ) ) ;
#41938 = CARTESIAN_POINT ( 'NONE',  ( 155.4202369374260400, 19.37982107812020871, 12.54055055082743309 ) ) ;
#41939 = CARTESIAN_POINT ( 'NONE',  ( -0.4778688367892073852, -283.5157583794382958, -337.7100911827484993 ) ) ;
#41940 = CARTESIAN_POINT ( 'NONE',  ( -84.11346918569235243, -290.4859367224390212, -209.4235973339414443 ) ) ;
#41941 = CARTESIAN_POINT ( 'NONE',  ( -101.2317039163527426, -280.7044450471170762, -228.7384085576266557 ) ) ;
#41942 = CARTESIAN_POINT ( 'NONE',  ( -111.9247549951099501, -280.0819143946588383, -253.3121824743580532 ) ) ;
#41943 = CARTESIAN_POINT ( 'NONE',  ( 35.03307748140585431, -281.2547469748348590, -260.4515029785027309 ) ) ;
#41944 = CARTESIAN_POINT ( 'NONE',  ( 14.87123209026071535, -276.7882957706938782, -216.5205166084354858 ) ) ;
#41945 = CARTESIAN_POINT ( 'NONE',  ( -32.01250978761930810, -294.9866973648014437, -347.1897338214240563 ) ) ;
#41946 = CARTESIAN_POINT ( 'NONE',  ( -100.2410300335867817, -288.0285807071863360, -310.5546634766658940 ) ) ;
#41947 = CARTESIAN_POINT ( 'NONE',  ( -78.13310918154785156, -294.5348827684800881, -331.3345653198613263 ) ) ;
#41948 = ORIENTED_EDGE ( 'NONE', *, *, #78922, .F. ) ;
#41949 = CARTESIAN_POINT ( 'NONE',  ( 10.85937363433953706, -284.3000377125366072, -327.1560846676737810 ) ) ;
#41950 = CARTESIAN_POINT ( 'NONE',  ( -107.8549698101690808, -296.4699687175842087, -251.3401685275310058 ) ) ;
#41951 = CARTESIAN_POINT ( 'NONE',  ( 39.40228548394804875, -294.6310100162099843, -270.2964404024463647 ) ) ;
#41952 = CARTESIAN_POINT ( 'NONE',  ( -48.33583839450611919, -283.8472040996707619, -342.6315932246827742 ) ) ;
#41953 = CARTESIAN_POINT ( 'NONE',  ( -1.401012977857417185, -273.5757196555520636, -202.5298035277165241 ) ) ;
#41954 = CARTESIAN_POINT ( 'NONE',  ( -111.4415249420204503, -290.9456895251522610, -290.9166220954808750 ) ) ;
#41955 = CARTESIAN_POINT ( 'NONE',  ( -37.94839629985712293, -284.1842174689621174, -194.5987433871758583 ) ) ;
#41956 = CARTESIAN_POINT ( 'NONE',  ( -105.9871784207898742, -291.3353689238521724, -235.4076355378543894 ) ) ;
#41957 = CARTESIAN_POINT ( 'NONE',  ( 24.96655473593886754, -287.3609803330804198, -232.2852875578358010 ) ) ;
#41958 = FACE_OUTER_BOUND ( 'NONE', #29857, .T. ) ;
#41959 = DIRECTION ( 'NONE',  ( 0.000000000000000000, 0.000000000000000000, 1.000000000000000000 ) ) ;
#41960 = CARTESIAN_POINT ( 'NONE',  ( 84.74214838284052576, 81.45383407810274434, -298.7931483813066507 ) ) ;
#41961 = CARTESIAN_POINT ( 'NONE',  ( 21.99644242613736367, -283.7215959280204629, -318.3576993332041525 ) ) ;
#41962 = CARTESIAN_POINT ( 'NONE',  ( 35.77081079830085031, -279.2666405000204009, -287.0812184334320705 ) ) ;
#41963 = ORIENTED_EDGE ( 'NONE', *, *, #87773, .T. ) ;
#41964 = CARTESIAN_POINT ( 'NONE',  ( -72.26490900774759041, -278.4988606263323163, -205.9049657880165967 ) ) ;
#41965 = CARTESIAN_POINT ( 'NONE',  ( -5.297447172730779030, -276.3086070062365707, -340.3533328651019474 ) ) ;
#41966 = CARTESIAN_POINT ( 'NONE',  ( -112.1108829561311069, -280.5124506622398712, -273.4591371667618773 ) ) ;
#41967 = CARTESIAN_POINT ( 'NONE',  ( -96.92303018069374332, -248.0440586835610759, -332.3996513594258317 ) ) ;
#41968 = CARTESIAN_POINT ( 'NONE',  ( -5.175390555506203860, -279.0420206143805899, -201.0506943540317479 ) ) ;
#41969 = CARTESIAN_POINT ( 'NONE',  ( -68.20526823414608941, -283.6648983628518863, -202.3957814513628932 ) ) ;
#41970 = CARTESIAN_POINT ( 'NONE',  ( -94.81950335412450670, -298.9932702060419274, -220.5806862762501623 ) ) ;
#41971 = CARTESIAN_POINT ( 'NONE',  ( 33.50727149462049681, -294.2798027013412252, -288.2052111746689889 ) ) ;
#41972 = ORIENTED_EDGE ( 'NONE', *, *, #31412, .T. ) ;
#41973 = CARTESIAN_POINT ( 'NONE',  ( -72.85062871364783632, -290.2564973392907746, -205.9583113522526219 ) ) ;
#41974 = CARTESIAN_POINT ( 'NONE',  ( 15.95041519588032841, -275.4353468568287440, -214.9240975839217640 ) ) ;
#41975 = CARTESIAN_POINT ( 'NONE',  ( -65.81314604114456301, -273.6690131771414372, -203.1422458734602117 ) ) ;
#41976 = ORIENTED_EDGE ( 'NONE', *, *, #3596, .F. ) ;
#41977 = CARTESIAN_POINT ( 'NONE',  ( 212.4629471475955427, 32.98517505407394168, 9.000000000000001776 ) ) ;
#41978 = DIRECTION ( 'NONE',  ( -1.000000000000000000, -0.000000000000000000, -0.000000000000000000 ) ) ;
#41979 = CARTESIAN_POINT ( 'NONE',  ( 175.2296996224750103, 142.2541816238762920, 24.00000000000001066 ) ) ;
#41980 = CARTESIAN_POINT ( 'NONE',  ( 35.82754170954765982, -282.5723709375300245, -265.8347373353341254 ) ) ;
#41981 = CARTESIAN_POINT ( 'NONE',  ( -56.32544983727824928, -281.5710994409631098, -196.7297259328687744 ) ) ;
#41982 = CARTESIAN_POINT ( 'NONE',  ( -94.47608406517130675, -282.9653463255980910, -316.1966870901869697 ) ) ;
#41983 = CARTESIAN_POINT ( 'NONE',  ( -46.63417465790233507, -281.7935173203842396, -196.6578400377112530 ) ) ;
#41984 = CARTESIAN_POINT ( 'NONE',  ( 25.96134958546090488, -274.5458729936648297, -308.0895111145813416 ) ) ;
#41985 = CARTESIAN_POINT ( 'NONE',  ( 154.5567693064130026, 20.34893504152563537, 12.19321973754205857 ) ) ;
#41986 = DIRECTION ( 'NONE',  ( -0.000000000000000000, -0.000000000000000000, -1.000000000000000000 ) ) ;
#41987 = CARTESIAN_POINT ( 'NONE',  ( -54.08607961464261393, -278.0645714637532251, -345.4075389757854282 ) ) ;
#41988 = ORIENTED_EDGE ( 'NONE', *, *, #32434, .F. ) ;
#41989 = ORIENTED_EDGE ( 'NONE', *, *, #56745, .T. ) ;
#41990 = CYLINDRICAL_SURFACE ( 'NONE', #67113, 4.999999999999978684 ) ;
#41991 = CARTESIAN_POINT ( 'NONE',  ( -73.46486226879098069, -285.5084218535164950, -336.5519544734756892 ) ) ;
#41992 = CARTESIAN_POINT ( 'NONE',  ( 8.958918719834645827, -291.9032233439606330, -213.6486487599679265 ) ) ;
#41993 = CARTESIAN_POINT ( 'NONE',  ( 18.56500581520394633, -287.6227629015178309, -323.1602942747457519 ) ) ;
#41994 = CARTESIAN_POINT ( 'NONE',  ( -42.72578242040736995, -284.2231796829869950, -196.5310720479739643 ) ) ;
#41996 = CARTESIAN_POINT ( 'NONE',  ( -53.65336685484921020, -287.5041829092231183, -342.5546325075417258 ) ) ;
#41995 = CARTESIAN_POINT ( 'NONE',  ( -57.53881849520140435, -284.3611245330838528, -199.5447370108839777 ) ) ;
#41997 = CARTESIAN_POINT ( 'NONE',  ( 28.51409099227173272, -283.1953442102738450, -302.8824520391976876 ) ) ;
#41998 = CARTESIAN_POINT ( 'NONE',  ( 3.788222921563208612, -272.6051628098734909, -207.5832207573302810 ) ) ;
#41999 = CARTESIAN_POINT ( 'NONE',  ( -54.76172544957044863, -284.2317206339737368, -196.1790235716186430 ) ) ;
#42000 = CARTESIAN_POINT ( 'NONE',  ( -36.93678113737666990, -300.0573775642432679, -195.3609712150442306 ) ) ;
#42001 = CARTESIAN_POINT ( 'NONE',  ( -86.53051407642091419, -283.3709929069373743, -213.4548401910015798 ) ) ;
#42002 = CARTESIAN_POINT ( 'NONE',  ( -57.18845146303002736, -280.7309636367400003, -199.8663315871593511 ) ) ;
#42003 = CARTESIAN_POINT ( 'NONE',  ( 22.38871256499044193, -288.9287967997583451, -224.7077295684182445 ) ) ;
#42004 = CARTESIAN_POINT ( 'NONE',  ( 199.0061125298537377, 250.0000000000000568, -7.725424859374024678 ) ) ;
#42005 = CYLINDRICAL_SURFACE ( 'NONE', #2003, 6.000000000000000000 ) ;
#42006 = CARTESIAN_POINT ( 'NONE',  ( 14.43331700338484502, -294.6931859882693061, -215.2560209799082429 ) ) ;
#42007 = CARTESIAN_POINT ( 'NONE',  ( -72.61677874022292656, -275.5189877917511012, -336.5622321948986837 ) ) ;
#42008 = CARTESIAN_POINT ( 'NONE',  ( -93.48182401163136035, -289.0317140774898235, -322.9015643338077552 ) ) ;
#42009 = CARTESIAN_POINT ( 'NONE',  ( -18.03057504029044722, -293.1988835312152446, -341.5897699496218820 ) ) ;
#42010 = CARTESIAN_POINT ( 'NONE',  ( -41.05949469224684378, -278.6892064019946247, -196.9620615692227545 ) ) ;
#42011 = CARTESIAN_POINT ( 'NONE',  ( -74.98078798095811237, -271.6269403856402391, -206.0782649918740503 ) ) ;
#42012 = CARTESIAN_POINT ( 'NONE',  ( 33.59708217105109185, -295.1199185804352396, -289.6166278810821950 ) ) ;
#42013 = CARTESIAN_POINT ( 'NONE',  ( 35.77081079830085031, -289.8376638359844719, -253.6410175316879361 ) ) ;
#42014 = CARTESIAN_POINT ( 'NONE',  ( -100.9608510622046396, -295.5915997388620440, -228.2028894894580731 ) ) ;
#42015 = CARTESIAN_POINT ( 'NONE',  ( -13.00504929679409116, -290.3307013512223307, -340.0329762955774413 ) ) ;
#42016 = CARTESIAN_POINT ( 'NONE',  ( 16.78376262359265425, -291.0491589107470531, -216.9540078373960910 ) ) ;
#42017 = CARTESIAN_POINT ( 'NONE',  ( -101.6473357735172840, -292.4639642137094029, -234.4770846594436193 ) ) ;
#42018 = CARTESIAN_POINT ( 'NONE',  ( 151.4990405259949569, 130.0000000000000568, -12.50000000000000178 ) ) ;
#42019 = CARTESIAN_POINT ( 'NONE',  ( -101.2697393067074785, -291.8416246946439969, -234.6788492769836978 ) ) ;
#42020 = CARTESIAN_POINT ( 'NONE',  ( 196.7320021107339301, 20.33855172480464546, 12.75691961062094570 ) ) ;
#42021 = AXIS2_PLACEMENT_3D ( 'NONE', #76524, #11647, #90683 ) ;
#42022 = CARTESIAN_POINT ( 'NONE',  ( -99.53884922450360762, -291.1611827008999853, -315.0996158264422888 ) ) ;
#42024 = CARTESIAN_POINT ( 'NONE',  ( 21.80470881790645521, -292.9533294582095095, -227.5531542952972472 ) ) ;
#42023 = CARTESIAN_POINT ( 'NONE',  ( 37.23968221855819394, -279.7099127654923336, -281.1325714673180300 ) ) ;
#42025 = CARTESIAN_POINT ( 'NONE',  ( 24.59174256752283227, -280.9441236267071531, -224.6090833188391400 ) ) ;
#42026 = CARTESIAN_POINT ( 'NONE',  ( 34.30630027885666777, -280.8602972240879581, -242.0676377927984788 ) ) ;
#42027 = CARTESIAN_POINT ( 'NONE',  ( -31.75939365461977104, -286.9815068654440893, -345.0378491626451023 ) ) ;
#42028 = CARTESIAN_POINT ( 'NONE',  ( 21.50943443380162989, -279.0653299630772040, -225.0921397182632688 ) ) ;
#42029 = EDGE_CURVE ( 'NONE', #45543, #1135, #4637, .T. ) ;
#42030 = CARTESIAN_POINT ( 'NONE',  ( -35.17968537688549446, -284.0791100073068947, -195.3794803803363038 ) ) ;
#42031 = CARTESIAN_POINT ( 'NONE',  ( -36.73841714686708571, -278.5394898503541299, -194.0439052400876676 ) ) ;
#42032 = CARTESIAN_POINT ( 'NONE',  ( -68.36306966320466927, -284.5744498255943995, -200.2100262135897992 ) ) ;
#42033 = CARTESIAN_POINT ( 'NONE',  ( 20.80365377746020883, -275.7316505180644981, -225.9364515393609736 ) ) ;
#42034 = CARTESIAN_POINT ( 'NONE',  ( 196.0553440093420079, 41.98397561837970215, 13.83198452061308359 ) ) ;
#42035 = CARTESIAN_POINT ( 'NONE',  ( -9.443748522189213901, -294.0229316460628297, -201.9829288310226900 ) ) ;
#42036 = CARTESIAN_POINT ( 'NONE',  ( 38.14266781216138469, -276.8268595040063360, -258.4145068128436264 ) ) ;
#42037 = CARTESIAN_POINT ( 'NONE',  ( -85.12228183661055425, -277.3997901489917695, -325.6467889821460631 ) ) ;
#42038 = CARTESIAN_POINT ( 'NONE',  ( -106.0050719069330967, -291.1687945960239290, -235.3961465443591692 ) ) ;
#42039 = CARTESIAN_POINT ( 'NONE',  ( 3.741840187476821011, -280.5841742682672475, -333.8379039944675242 ) ) ;
#42040 = CARTESIAN_POINT ( 'NONE',  ( -101.3234253852497204, -290.0978208675721248, -234.6234748633722518 ) ) ;
#42041 = CARTESIAN_POINT ( 'NONE',  ( -34.94475575749886787, -293.0218790351939901, -345.3228102614483532 ) ) ;
#42042 = ORIENTED_EDGE ( 'NONE', *, *, #7316, .T. ) ;
#42043 = DIRECTION ( 'NONE',  ( 0.000000000000000000, 0.000000000000000000, 1.000000000000000000 ) ) ;
#42044 = CARTESIAN_POINT ( 'NONE',  ( -7.239167516334062746, -291.9656571399365248, -203.7891571266743256 ) ) ;
#42045 = CARTESIAN_POINT ( 'NONE',  ( 140.6539576904058606, 275.5000000000000568, -10.49999999999999822 ) ) ;
#42046 = CIRCLE ( 'NONE', #35245, 1.000000000000000888 ) ;
#42047 = CARTESIAN_POINT ( 'NONE',  ( 27.36219212280433055, -278.6237833571632905, -239.2376011013261916 ) ) ;
#42048 = CARTESIAN_POINT ( 'NONE',  ( -87.30001534795461282, -296.4344745822299956, -212.0073767418146531 ) ) ;
#42049 = CARTESIAN_POINT ( 'NONE',  ( 28.22961642614604472, -279.1901131627832910, -232.4044594910565422 ) ) ;
#42050 = CARTESIAN_POINT ( 'NONE',  ( -110.2107022552328743, -285.5718615468011876, -293.7153783079858158 ) ) ;
#42051 = CARTESIAN_POINT ( 'NONE',  ( -12.01999254973419085, -286.2244361981587986, -201.8935261611792669 ) ) ;
#42052 = CARTESIAN_POINT ( 'NONE',  ( 35.39465542970469158, -277.2310034248228021, -282.5076081247422621 ) ) ;
#42053 = CARTESIAN_POINT ( 'NONE',  ( -61.57036041639354096, -293.3884373128452694, -341.0191559482328785 ) ) ;
#42054 = CARTESIAN_POINT ( 'NONE',  ( -108.9442868164720579, -298.0677189211679661, -289.1473247931770061 ) ) ;
#42055 = CARTESIAN_POINT ( 'NONE',  ( 19.47929614660065667, -275.0015746348555012, -316.8406299265187727 ) ) ;
#42056 = EDGE_LOOP ( 'NONE', ( #19746, #56213, #30811, #89105, #15538, #50356, #87713 ) ) ;
#42057 = CARTESIAN_POINT ( 'NONE',  ( 194.7685530992919780, 41.40013651751808510, 13.93755082198983075 ) ) ;
#42058 = CARTESIAN_POINT ( 'NONE',  ( -101.6129552175586497, -295.6605510865146584, -312.8243787881069693 ) ) ;
#42059 = CARTESIAN_POINT ( 'NONE',  ( 35.39801062582398572, -289.2676602293741439, -254.5418676521328791 ) ) ;
#42060 = DIRECTION ( 'NONE',  ( -0.000000000000000000, 1.000000000000000000, -0.000000000000000000 ) ) ;
#42061 = CARTESIAN_POINT ( 'NONE',  ( -37.25958740186422347, -289.7025121495771600, -343.4630052775654576 ) ) ;
#42062 = ORIENTED_EDGE ( 'NONE', *, *, #42403, .T. ) ;
#42063 = CARTESIAN_POINT ( 'NONE',  ( -77.35959418939796706, -278.5884135566461168, -204.7908966724019137 ) ) ;
#42064 = CARTESIAN_POINT ( 'NONE',  ( -82.91684607929566653, -298.0986064139047471, -208.3577355048848858 ) ) ;
#42065 = CARTESIAN_POINT ( 'NONE',  ( -112.1443741957517233, -288.5387581724811525, -282.3971236965435878 ) ) ;
#42066 = CARTESIAN_POINT ( 'NONE',  ( -70.79484542062520802, -295.8146109541293072, -339.7054972979488525 ) ) ;
#42067 = CARTESIAN_POINT ( 'NONE',  ( 10.94160792830293261, -293.0751463410686597, -215.5140034193332497 ) ) ;
#42068 = CYLINDRICAL_SURFACE ( 'NONE', #21875, 4.000000000000003553 ) ;
#42069 = CARTESIAN_POINT ( 'NONE',  ( 185.0172044724083946, 250.5000000000000568, 22.46007009812148070 ) ) ;
#42070 = CARTESIAN_POINT ( 'NONE',  ( 200.4644824113734671, 275.0000000000000568, -2.942835885954290465 ) ) ;
#42071 = CARTESIAN_POINT ( 'NONE',  ( -23.41926306724479900, -290.3975307037973721, -345.4405661913328345 ) ) ;
#42072 = CARTESIAN_POINT ( 'NONE',  ( -37.37352853689063181, -276.5519495502701375, -190.3611179825600175 ) ) ;
#42073 = CARTESIAN_POINT ( 'NONE',  ( 28.21375987243529337, -281.4277882269954603, -310.6589574306599957 ) ) ;
#42074 = CARTESIAN_POINT ( 'NONE',  ( -26.45141992758102845, -284.9135586063146661, -344.4503898334593259 ) ) ;
#42075 = CARTESIAN_POINT ( 'NONE',  ( -1.231864890178082872, -285.0964021877157961, -203.0210400719131201 ) ) ;
#42076 = CARTESIAN_POINT ( 'NONE',  ( -110.8448092849325093, -288.4786531565889049, -282.2146085632067525 ) ) ;
#42077 = CARTESIAN_POINT ( 'NONE',  ( 35.39325635673228732, -277.1401082105775231, -248.9663918718121636 ) ) ;
#42078 = VERTEX_POINT ( 'NONE', #48648 ) ;
#42080 = CARTESIAN_POINT ( 'NONE',  ( 18.91986168076719466, -280.2395298437859310, -223.6669689975476274 ) ) ;
#42079 = CARTESIAN_POINT ( 'NONE',  ( -108.6067547304953962, -278.7615401045008525, -254.4832753974120578 ) ) ;
#42081 = CARTESIAN_POINT ( 'NONE',  ( 8.069140569896507742, -277.5275090555168731, -332.2277495529352223 ) ) ;
#42082 = CARTESIAN_POINT ( 'NONE',  ( -48.04802613618277718, -278.7139081193637367, -194.4564924471395670 ) ) ;
#42083 = CARTESIAN_POINT ( 'NONE',  ( 195.1507973710101567, 283.8842776367829401, -110.7649439234235729 ) ) ;
#42084 = CARTESIAN_POINT ( 'NONE',  ( -70.04246372125138009, -274.5731428576596045, -200.8954679847426519 ) ) ;
#42085 = CARTESIAN_POINT ( 'NONE',  ( -103.6368475773368942, -274.5686611828822947, -232.4706282480738935 ) ) ;
#42086 = CARTESIAN_POINT ( 'NONE',  ( -69.91165696735023971, -282.1233781216988064, -202.8022627189028810 ) ) ;
#42087 = ORIENTED_EDGE ( 'NONE', *, *, #63349, .T. ) ;
#42088 = CIRCLE ( 'NONE', #1281, 7.500000000000012434 ) ;
#42089 = LINE ( 'NONE', #93691, #87701 ) ;
#42090 = CARTESIAN_POINT ( 'NONE',  ( 34.82840873836469342, -288.8009209392869820, -283.2336259117558939 ) ) ;
#42091 = CARTESIAN_POINT ( 'NONE',  ( -110.7482355669279315, -286.5636539579506916, -250.5301347197553810 ) ) ;
#42092 = CARTESIAN_POINT ( 'NONE',  ( 27.11643658544443625, -287.3714257439831954, -304.9513084693872997 ) ) ;
#42093 = CARTESIAN_POINT ( 'NONE',  ( -113.5393281124190707, -283.9217793124122409, -281.3888541548994908 ) ) ;
#42094 = CARTESIAN_POINT ( 'NONE',  ( 22.77689436350958374, -279.3605917052735776, -227.5569708410353371 ) ) ;
#42095 = CARTESIAN_POINT ( 'NONE',  ( -33.19292430996794963, -287.9652290802163748, -196.1912722001160034 ) ) ;
#42096 = CARTESIAN_POINT ( 'NONE',  ( 29.93963459380002945, -280.4345705094478944, -300.5517617227233700 ) ) ;
#42097 = CARTESIAN_POINT ( 'NONE',  ( -83.30220137022500637, -279.0119753137107068, -327.7753249892749636 ) ) ;
#42098 = CARTESIAN_POINT ( 'NONE',  ( 27.91343983204256674, -275.5988971401802132, -237.5014900138333189 ) ) ;
#42099 = CARTESIAN_POINT ( 'NONE',  ( 33.66844956706929537, -286.7153623773274944, -299.2350239973816315 ) ) ;
#42100 = CARTESIAN_POINT ( 'NONE',  ( -67.80790689833449392, -284.2447944517442693, -340.9016670723125912 ) ) ;
#42101 = CARTESIAN_POINT ( 'NONE',  ( -106.9473036443437906, -284.6242651026552153, -303.1420097061146635 ) ) ;
#42102 = CARTESIAN_POINT ( 'NONE',  ( -6.031017544437445643, -282.7955433783161538, -336.3190961069706759 ) ) ;
#42103 = EDGE_LOOP ( 'NONE', ( #20443, #45557, #80130, #5430 ) ) ;
#42104 = ORIENTED_EDGE ( 'NONE', *, *, #21510, .T. ) ;
#42105 = CARTESIAN_POINT ( 'NONE',  ( -112.3417001280820386, -272.5521521680024648, -270.3611179825637691 ) ) ;
#42106 = CARTESIAN_POINT ( 'NONE',  ( -43.06497225699423836, -290.9840985263101061, -345.9094444818704233 ) ) ;
#42107 = CARTESIAN_POINT ( 'NONE',  ( -56.05186982195797185, -290.5010254134408569, -196.1227815674955650 ) ) ;
#42108 = CARTESIAN_POINT ( 'NONE',  ( -85.45575128015269684, -272.4266123007801070, -215.0807985892640488 ) ) ;
#42109 = CARTESIAN_POINT ( 'NONE',  ( 29.48197768727347068, -293.3967643590737566, -308.5200631123209973 ) ) ;
#42110 = CARTESIAN_POINT ( 'NONE',  ( -104.6891480445574985, -288.6315859034411346, -300.4042494969926906 ) ) ;
#42111 = CARTESIAN_POINT ( 'NONE',  ( -6.832337385176574962, -290.6980681784572766, -202.9285383130988976 ) ) ;
#42112 = CARTESIAN_POINT ( 'NONE',  ( -10.56501337521648587, -289.9001132167441597, -338.7540531596937967 ) ) ;
#42113 = DIRECTION ( 'NONE',  ( -0.000000000000000000, -0.000000000000000000, -1.000000000000000000 ) ) ;
#42114 = CARTESIAN_POINT ( 'NONE',  ( -90.17118355432761234, -291.7987423681811947, -323.6699113191148172 ) ) ;
#42115 = CARTESIAN_POINT ( 'NONE',  ( -98.52363673168103730, -289.1445077760039908, -226.6942076087616158 ) ) ;
#42116 = CARTESIAN_POINT ( 'NONE',  ( -45.51933279605668758, -293.9488161272667526, -195.7571921396720995 ) ) ;
#42117 = CARTESIAN_POINT ( 'NONE',  ( 11.28135300780948214, -287.6865909179635423, -215.5279746838696440 ) ) ;
#42118 = CARTESIAN_POINT ( 'NONE',  ( -4.154314380642599502, -294.4888015521621014, -202.9034280918289426 ) ) ;
#42119 = DIRECTION ( 'NONE',  ( -0.000000000000000000, -1.000000000000000000, -0.000000000000000000 ) ) ;
#42120 = DIRECTION ( 'NONE',  ( -0.000000000000000000, 0.000000000000000000, -1.000000000000000000 ) ) ;
#42121 = CARTESIAN_POINT ( 'NONE',  ( 33.17353357999118657, -277.1885329724655662, -243.7902953377071071 ) ) ;
#42122 = CARTESIAN_POINT ( 'NONE',  ( -92.58802361285535198, -295.0162071209260830, -323.7652616586175327 ) ) ;
#42123 = CARTESIAN_POINT ( 'NONE',  ( -33.97242895344523106, -272.3349687238520573, -196.4245098187130338 ) ) ;
#42124 = CARTESIAN_POINT ( 'NONE',  ( -90.12378267622244721, -275.8847210037165496, -322.9259199327958072 ) ) ;
#42125 = CARTESIAN_POINT ( 'NONE',  ( -34.03807967223432485, -275.2997065238326400, -197.0384298331000537 ) ) ;
#42126 = EDGE_CURVE ( 'NONE', #76803, #64817, #32499, .T. ) ;
#42127 = CARTESIAN_POINT ( 'NONE',  ( -69.96912571342598142, -296.9159226804785021, -336.3219095078279679 ) ) ;
#42128 = EDGE_CURVE ( 'NONE', #78327, #83522, #9593, .T. ) ;
#42129 = DIRECTION ( 'NONE',  ( -1.000000000000000000, -0.000000000000000000, -0.000000000000000000 ) ) ;
#42130 = CARTESIAN_POINT ( 'NONE',  ( -72.93436184399428157, -298.3704235147003487, -206.4411355109402564 ) ) ;
#42131 = DIRECTION ( 'NONE',  ( -1.000000000000000000, -0.000000000000000000, -0.000000000000000000 ) ) ;
#42133 = CARTESIAN_POINT ( 'NONE',  ( -44.56908489952338925, -297.9582964478407234, -197.6693916683557006 ) ) ;
#42132 = CARTESIAN_POINT ( 'NONE',  ( 36.93986834925429008, -285.4093115655298334, -257.6100704862456041 ) ) ;
#42134 = CARTESIAN_POINT ( 'NONE',  ( -32.30641958262449975, -286.1139684545679529, -193.5127647814072986 ) ) ;
#42135 = CARTESIAN_POINT ( 'NONE',  ( -99.01474309014216146, -289.6055843361505708, -316.4500430296726563 ) ) ;
#42136 = CARTESIAN_POINT ( 'NONE',  ( -105.6642417930441837, -298.1163139150809798, -302.1484912650414003 ) ) ;
#42137 = CARTESIAN_POINT ( 'NONE',  ( 9.352746220141005651, -292.4090604623286822, -328.9055307825724981 ) ) ;
#42138 = CARTESIAN_POINT ( 'NONE',  ( -45.24656889051706798, -279.1517471477288268, -193.8774083148039153 ) ) ;
#42139 = CARTESIAN_POINT ( 'NONE',  ( -85.28047601435908120, -294.9094976428776249, -210.1954327657594206 ) ) ;
#42140 = CARTESIAN_POINT ( 'NONE',  ( -55.80257052418233599, -229.5268262511776527, 22.47499999999998721 ) ) ;
#42141 = CARTESIAN_POINT ( 'NONE',  ( -88.95111478276238870, -288.5924118681971322, -322.5492279637877004 ) ) ;
#42142 = CARTESIAN_POINT ( 'NONE',  ( 198.1245416649653919, 70.21476723776075346, -10.41797401930329592 ) ) ;
#42143 = CARTESIAN_POINT ( 'NONE',  ( -88.10121063534423058, -287.7618270281723198, -325.6445708824180088 ) ) ;
#42144 = CARTESIAN_POINT ( 'NONE',  ( -98.42867341926329061, -274.6408742057246855, -229.0500343712124618 ) ) ;
#42145 = CARTESIAN_POINT ( 'NONE',  ( -53.65253667913266611, -281.2722276150786342, -195.6573632819490172 ) ) ;
#42147 = CARTESIAN_POINT ( 'NONE',  ( 35.35234721594390095, -281.4570432862635698, -263.1513449924633505 ) ) ;
#42146 = CARTESIAN_POINT ( 'NONE',  ( -90.45789314581270446, -295.3245937662110805, -216.9094871293813753 ) ) ;
#42148 = CARTESIAN_POINT ( 'NONE',  ( -112.6047098731618803, -296.5154422344219824, -286.6239396518015496 ) ) ;
#42149 = CARTESIAN_POINT ( 'NONE',  ( -36.49258129533864548, -299.5830937490768520, -196.6675549952466611 ) ) ;
#42150 = EDGE_CURVE ( 'NONE', #2981, #30245, #64319, .T. ) ;
#42151 = CARTESIAN_POINT ( 'NONE',  ( 35.04776516096256955, -283.2995422298061499, -250.6970259347930892 ) ) ;
#42153 = CARTESIAN_POINT ( 'NONE',  ( -101.6797210199117387, -295.1349046563659613, -305.3472225843132719 ) ) ;
#42152 = AXIS2_PLACEMENT_3D ( 'NONE', #86276, #43662, #72557 ) ;
#42154 = VERTEX_POINT ( 'NONE', #27840 ) ;
#42155 = CARTESIAN_POINT ( 'NONE',  ( 73.43068321062709458, -178.2391364535880882, 0.000000000000000000 ) ) ;
#42156 = CARTESIAN_POINT ( 'NONE',  ( -15.63054467777635992, -284.7497122728523777, -341.7787105588999452 ) ) ;
#42157 = LINE ( 'NONE', #63991, #74572 ) ;
#42158 = CARTESIAN_POINT ( 'NONE',  ( -85.28047601435909542, -294.9094976428776818, -210.1954327657594206 ) ) ;
#42159 = CARTESIAN_POINT ( 'NONE',  ( 34.03046139196352726, -275.1128073459044003, -298.9680657569005575 ) ) ;
#42160 = CARTESIAN_POINT ( 'NONE',  ( 27.48751066261156595, -292.9291070127144962, -236.8026103765939467 ) ) ;
#42161 = CARTESIAN_POINT ( 'NONE',  ( 34.91428985651987915, -283.2623752425332100, -284.9084766489496587 ) ) ;
#42162 = SHAPE_REPRESENTATION ( 'cast Iron C-Frame Chassis', ( #18940 ), #770 ) ;
#42163 = CARTESIAN_POINT ( 'NONE',  ( 34.02092610902858638, -277.3979666706746912, -289.1711151475886936 ) ) ;
#42164 = CARTESIAN_POINT ( 'NONE',  ( -83.51261380528107736, -285.0962838659742715, -331.3115024803383903 ) ) ;
#42165 = EDGE_CURVE ( 'NONE', #5311, #13346, #8124, .T. ) ;
#42166 = CARTESIAN_POINT ( 'NONE',  ( -83.05394679926037327, -282.4885527937484540, -327.8503918926580241 ) ) ;
#42167 = CARTESIAN_POINT ( 'NONE',  ( -102.5632736793492796, -281.0459011237286404, -233.3321159723420806 ) ) ;
#42168 = CARTESIAN_POINT ( 'NONE',  ( -113.0686821389476222, -272.8967761882815921, -256.1327989363236952 ) ) ;
#42169 = CARTESIAN_POINT ( 'NONE',  ( 24.48113922993194436, -274.7751614573199390, -224.4597395910907665 ) ) ;
#42170 =( BOUNDED_CURVE ( )  B_SPLINE_CURVE ( 3, ( #34708, #64567, #92931, #49384 ),
 .UNSPECIFIED., .F., .F. ) 
 B_SPLINE_CURVE_WITH_KNOTS ( ( 4, 4 ),
 ( 3.141592653589793116, 4.289818581637806716 ),
 .UNSPECIFIED. ) 
 CURVE ( )  GEOMETRIC_REPRESENTATION_ITEM ( )  RATIONAL_B_SPLINE_CURVE ( ( 1.000000000000000000, 0.8931162488198155502, 0.8931162488198155502, 1.000000000000000000 ) ) 
 REPRESENTATION_ITEM ( '' )  );
#42171 = CARTESIAN_POINT ( 'NONE',  ( 15.35257030271881362, -296.2211767302954968, -323.0133506394817573 ) ) ;
#42172 = CYLINDRICAL_SURFACE ( 'NONE', #53614, 2.397123461337413719 ) ;
#42173 = CARTESIAN_POINT ( 'NONE',  ( 208.6208076322478746, 32.98517505407394168, 12.09245862095555601 ) ) ;
#42174 = CARTESIAN_POINT ( 'NONE',  ( -89.87300498813381466, -293.9233782169240499, -325.0297771315518389 ) ) ;
#42175 = CARTESIAN_POINT ( 'NONE',  ( 32.95535355670186561, -275.3233093522191552, -290.3144907837802293 ) ) ;
#42176 = CARTESIAN_POINT ( 'NONE',  ( -27.81502623903721982, -296.4535314705951805, -346.1235756325683042 ) ) ;
#42177 = CARTESIAN_POINT ( 'NONE',  ( 39.10700906647314667, -294.8280454373270345, -275.9945798117737468 ) ) ;
#42178 = CARTESIAN_POINT ( 'NONE',  ( 22.65831315928593170, -290.1646338485070373, -315.1042372017852244 ) ) ;
#42179 = CARTESIAN_POINT ( 'NONE',  ( -111.7872645182141156, -276.6562656011413992, -262.2578052085316358 ) ) ;
#42180 = CARTESIAN_POINT ( 'NONE',  ( -104.4181645627269006, -280.0426010191475257, -302.7612964063426944 ) ) ;
#42181 = CARTESIAN_POINT ( 'NONE',  ( -98.37783157152060198, -294.0493405247094074, -312.9745531562338670 ) ) ;
#42182 = CARTESIAN_POINT ( 'NONE',  ( 36.35255977281524764, -283.6368109510935938, -288.0080504870875870 ) ) ;
#42183 = CARTESIAN_POINT ( 'NONE',  ( -33.20753275144534911, -285.0256165265851678, -197.1186374804175045 ) ) ;
#42184 = CARTESIAN_POINT ( 'NONE',  ( 27.25360408407748025, -24.20672218296157752, -344.2562845684955164 ) ) ;
#42185 = ORIENTED_EDGE ( 'NONE', *, *, #91432, .F. ) ;
#42186 = CARTESIAN_POINT ( 'NONE',  ( -104.6153801052060146, -284.6014429029134476, -241.8350534578070210 ) ) ;
#42187 = EDGE_LOOP ( 'NONE', ( #20900, #24748, #48498, #78350 ) ) ;
#42188 = CARTESIAN_POINT ( 'NONE',  ( 36.89605633750436908, -282.8736171719617118, -289.6029480837335655 ) ) ;
#42189 = CARTESIAN_POINT ( 'NONE',  ( -109.5976008122744361, -283.6696528231084926, -244.9230847573956567 ) ) ;
#42190 = CARTESIAN_POINT ( 'NONE',  ( -112.4896841582854989, -279.6907874466978683, -254.6260255366181582 ) ) ;
#42191 =( NAMED_UNIT ( * ) SI_UNIT ( $, .STERADIAN. ) SOLID_ANGLE_UNIT ( ) );
#42192 = CARTESIAN_POINT ( 'NONE',  ( -71.24524488177144121, -279.0117448326091107, -338.7223453594258444 ) ) ;
#42193 = CARTESIAN_POINT ( 'NONE',  ( 12.91927517772756495, -281.3841028665469821, -212.1619156890937745 ) ) ;
#42194 = CARTESIAN_POINT ( 'NONE',  ( -105.5937364680635966, -299.2662352645559167, -254.8156830097664738 ) ) ;
#42195 = CARTESIAN_POINT ( 'NONE',  ( -113.0732809282716147, -274.2376448861158451, -284.1882621119263490 ) ) ;
#42196 = ORIENTED_EDGE ( 'NONE', *, *, #47322, .T. ) ;
#42197 = CARTESIAN_POINT ( 'NONE',  ( 22.94335637594691235, -276.9462939732044902, -226.0244470289034950 ) ) ;
#42198 = CARTESIAN_POINT ( 'NONE',  ( -104.7838118829956073, -255.6369273504282091, -326.4926257996353343 ) ) ;
#42199 = CARTESIAN_POINT ( 'NONE',  ( -49.38295309825753776, -277.9179990950224237, -196.6939270010225300 ) ) ;
#42200 = CARTESIAN_POINT ( 'NONE',  ( -110.5594846597458911, -292.0542383915988012, -290.6867186739625595 ) ) ;
#42201 = CARTESIAN_POINT ( 'NONE',  ( 28.83431919691496503, -292.4803615584298768, -239.1831744904247898 ) ) ;
#42202 = CARTESIAN_POINT ( 'NONE',  ( -87.34920049625704053, -289.2351826819626126, -328.9014072892380796 ) ) ;
#42203 = CARTESIAN_POINT ( 'NONE',  ( 215.7837434059060229, -147.7221692137691775, 8.778910157967997563 ) ) ;
#42205 = CARTESIAN_POINT ( 'NONE',  ( -57.59457826035073680, -284.1862965901574967, -199.3413116473142566 ) ) ;
#42204 = CARTESIAN_POINT ( 'NONE',  ( 1.454508968936686575, -293.1190228977339984, -336.1901423747411286 ) ) ;
#42206 = CARTESIAN_POINT ( 'NONE',  ( -107.7502061521683316, -292.7198254812090568, -246.8343723662671891 ) ) ;
#42207 = CARTESIAN_POINT ( 'NONE',  ( -16.96173304368145196, -284.7998639787448951, -199.4885245944802534 ) ) ;
#42208 = CARTESIAN_POINT ( 'NONE',  ( -45.67889087126178538, -284.4750703068490907, -343.4311843225646612 ) ) ;
#42209 = VERTEX_POINT ( 'NONE', #70464 ) ;
#42210 = CARTESIAN_POINT ( 'NONE',  ( -99.84645246660110729, -292.0854451413042625, -225.7968256807372143 ) ) ;
#42211 = CARTESIAN_POINT ( 'NONE',  ( 5.633343002982027059, -282.9443524922580195, -329.4469378496282275 ) ) ;
#42212 = CARTESIAN_POINT ( 'NONE',  ( -34.88283910893213147, -293.8168352204102689, -346.9245735088458105 ) ) ;
#42213 = CARTESIAN_POINT ( 'NONE',  ( -59.96994870452659399, -290.1409676069350780, -343.7921821615907447 ) ) ;
#42214 = CARTESIAN_POINT ( 'NONE',  ( -98.10714326194072044, -290.4137429133613750, -317.5531493466613711 ) ) ;
#42215 = CARTESIAN_POINT ( 'NONE',  ( 34.99584765746132575, -287.5845243074135738, -260.1797802226952285 ) ) ;
#42216 = ORIENTED_EDGE ( 'NONE', *, *, #36169, .F. ) ;
#42217 = FACE_OUTER_BOUND ( 'NONE', #74124, .T. ) ;
#42218 = CARTESIAN_POINT ( 'NONE',  ( -98.98942229970184314, -297.8185843613829888, -314.4933335870838960 ) ) ;
#42219 = CARTESIAN_POINT ( 'NONE',  ( -73.03554292154213101, -296.2743859815861924, -202.6325172155620749 ) ) ;
#42220 = CARTESIAN_POINT ( 'NONE',  ( -107.8415725520628712, -277.8727106818788002, -250.4859891648111159 ) ) ;
#42221 = CARTESIAN_POINT ( 'NONE',  ( -94.09562997993657518, -272.7671124503519877, -218.3944026816361372 ) ) ;
#42222 = CIRCLE ( 'NONE', #22557, 24.50000000000000355 ) ;
#42223 = CARTESIAN_POINT ( 'NONE',  ( -96.98081189327255913, -294.4316892329314328, -313.6710468714568378 ) ) ;
#42224 = CARTESIAN_POINT ( 'NONE',  ( 32.22176225944927808, -277.6462176144157752, -295.7866218366769999 ) ) ;
#42225 = CARTESIAN_POINT ( 'NONE',  ( -106.5595144590962491, -271.0459273630126518, -243.3911021035835631 ) ) ;
#42226 = CARTESIAN_POINT ( 'NONE',  ( -26.13170543039678861, -296.1113294050147715, -342.8970850806831550 ) ) ;
#42227 = CARTESIAN_POINT ( 'NONE',  ( -50.51330823245528023, -296.3040016795968654, -342.4772383211392253 ) ) ;
#42228 = CARTESIAN_POINT ( 'NONE',  ( 133.0872704186301405, -299.5541904835127980, -195.3611179825600175 ) ) ;
#42229 = CARTESIAN_POINT ( 'NONE',  ( -102.4216391125737999, -297.6292531184909080, -309.9974896128650812 ) ) ;
#42230 = CARTESIAN_POINT ( 'NONE',  ( -111.7824907539996673, -294.6866888240654703, -259.8472399430826272 ) ) ;
#42231 = CARTESIAN_POINT ( 'NONE',  ( -7.235835244455974369, -293.1092325283569267, -203.7463330762865041 ) ) ;
#42232 = CARTESIAN_POINT ( 'NONE',  ( -114.1806035973878863, -273.3907171491254076, -267.5098654519179036 ) ) ;
#42233 = CARTESIAN_POINT ( 'NONE',  ( -87.14137452677120166, -288.3366226459800714, -324.6092932845065206 ) ) ;
#42234 = CARTESIAN_POINT ( 'NONE',  ( -86.64354579147382651, -275.3675513877705043, -213.7734863356731694 ) ) ;
#42235 = CARTESIAN_POINT ( 'NONE',  ( -95.04447986815924310, -273.7341246248622610, -219.4698995494528333 ) ) ;
#42236 = CARTESIAN_POINT ( 'NONE',  ( -106.7282076962837181, -297.1892042104578309, -247.4499622215209911 ) ) ;
#42237 = CARTESIAN_POINT ( 'NONE',  ( -38.17750912248671824, -282.0216133365882456, -195.0105491031473548 ) ) ;
#42238 = CARTESIAN_POINT ( 'NONE',  ( -17.10620383300768665, -278.9929290163530027, -196.5788507280984163 ) ) ;
#42239 = ORIENTED_EDGE ( 'NONE', *, *, #74648, .F. ) ;
#42240 = CARTESIAN_POINT ( 'NONE',  ( -41.57183794321338866, -282.4525661027702768, -347.1950050990007526 ) ) ;
#42241 = CARTESIAN_POINT ( 'NONE',  ( 29.00381038165020442, -275.4074882379208020, -309.2402386202039679 ) ) ;
#42242 = CARTESIAN_POINT ( 'NONE',  ( 34.84459382249985993, -280.2645185754401496, -294.9294596004835398 ) ) ;
#42243 = CARTESIAN_POINT ( 'NONE',  ( 5.168896820478852128, -278.6254773600643375, -208.3701704873829499 ) ) ;
#42244 = EDGE_CURVE ( 'NONE', #92063, #61209, #56547, .T. ) ;
#42245 = CARTESIAN_POINT ( 'NONE',  ( -72.17070865561098003, -272.1570538325202619, -205.4790794785414221 ) ) ;
#42246 = CARTESIAN_POINT ( 'NONE',  ( 35.35380634154680024, -277.7899070664295209, -288.8610073231438946 ) ) ;
#42247 = DIRECTION ( 'NONE',  ( -1.000000000000000000, -0.000000000000000000, -0.000000000000000000 ) ) ;
#42248 = PLANE ( 'NONE',  #39777 ) ;
#42249 = CARTESIAN_POINT ( 'NONE',  ( -99.90346104626898693, -295.3692772052853002, -227.2105427463845899 ) ) ;
#42250 = CARTESIAN_POINT ( 'NONE',  ( -25.25977348276387247, -290.2255582279785813, -195.9807855761962685 ) ) ;
#42251 = CARTESIAN_POINT ( 'NONE',  ( -94.71130554120206568, -291.2488173687601716, -219.0022981485447815 ) ) ;
#42252 = CARTESIAN_POINT ( 'NONE',  ( 36.14746065538369635, -277.3492191554605029, -254.5088575786688239 ) ) ;
#42253 = CARTESIAN_POINT ( 'NONE',  ( -65.29108103802053620, -271.6867263482307067, -200.7496220629793697 ) ) ;
#42254 = CARTESIAN_POINT ( 'NONE',  ( 193.5407187895461618, 250.2122328390418602, 16.89624193607488323 ) ) ;
#42255 = CARTESIAN_POINT ( 'NONE',  ( -38.68201801359813174, -284.9889888730991174, -345.9092334427348305 ) ) ;
#42256 = CARTESIAN_POINT ( 'NONE',  ( -23.40286736638519471, -135.2391364535880598, -22.50000000000000000 ) ) ;
#42257 = CARTESIAN_POINT ( 'NONE',  ( -112.3519692451748142, -282.5201479316810946, -272.8408409343114158 ) ) ;
#42258 = CARTESIAN_POINT ( 'NONE',  ( 208.6208076322478746, 32.98517505407394168, 14.26380412667038655 ) ) ;
#42259 = CARTESIAN_POINT ( 'NONE',  ( -20.77338096908489717, -293.6297602833795395, -341.9160998228068706 ) ) ;
#42260 = CARTESIAN_POINT ( 'NONE',  ( 33.86133416336743096, -285.4179608160854968, -249.3163830905704117 ) ) ;
#42261 = B_SPLINE_CURVE_WITH_KNOTS ( 'NONE', 3,
 ( #82921, #17145, #46468, #23320 ),
 .UNSPECIFIED., .F., .F.,
 ( 4, 4 ),
 ( 0.000000000000000000, 9.632970524406852609E-05 ),
 .UNSPECIFIED. ) ;
#42262 = DIRECTION ( 'NONE',  ( 0.000000000000000000, 0.000000000000000000, -1.000000000000000000 ) ) ;
#42263 = CARTESIAN_POINT ( 'NONE',  ( -34.24338683495191304, -293.0130252916814015, -345.2970980308921867 ) ) ;
#42264 = CARTESIAN_POINT ( 'NONE',  ( -108.3758997270184921, -283.3901913537162613, -242.3454811052901334 ) ) ;
#42265 = CARTESIAN_POINT ( 'NONE',  ( -54.70051500970891567, -281.4255993396954523, -198.5789091378471483 ) ) ;
#42266 = CARTESIAN_POINT ( 'NONE',  ( -113.0971089942133858, -285.9044788522738259, -258.6474786108802846 ) ) ;
#42267 = CARTESIAN_POINT ( 'NONE',  ( 38.60627189909572365, -279.8227406011047265, -272.7858976308131105 ) ) ;
#42268 = CARTESIAN_POINT ( 'NONE',  ( 34.99614351355761954, -287.4178711535176376, -260.1818832611007224 ) ) ;
#42269 = CARTESIAN_POINT ( 'NONE',  ( -78.95032884280882968, -279.0502580464121820, -331.1199194987961505 ) ) ;
#42270 = CARTESIAN_POINT ( 'NONE',  ( -87.19811882456576768, -278.5714949338289443, -323.9049247334257302 ) ) ;
#42271 = ADVANCED_FACE ( 'NONE', ( #34463 ), #32320, .F. ) ;
#42272 = EDGE_CURVE ( 'NONE', #71428, #23799, #68551, .T. ) ;
#42273 = CARTESIAN_POINT ( 'NONE',  ( -94.58400159273634245, -287.2083764284462291, -221.2754231474131075 ) ) ;
#42274 = ORIENTED_EDGE ( 'NONE', *, *, #84910, .F. ) ;
#42275 = CARTESIAN_POINT ( 'NONE',  ( -23.35769572636721492, -298.0560261227212777, -193.3614995326353494 ) ) ;
#42276 = CARTESIAN_POINT ( 'NONE',  ( 36.38773870376633113, -289.6834478554512202, -282.0967856895698560 ) ) ;
#42277 = FACE_OUTER_BOUND ( 'NONE', #46060, .T. ) ;
#42278 = CARTESIAN_POINT ( 'NONE',  ( -115.3288506153726871, -286.8376638359844719, -288.1938231032136741 ) ) ;
#42279 = EDGE_LOOP ( 'NONE', ( #30953, #31415, #37114, #2735 ) ) ;
#42280 = CARTESIAN_POINT ( 'NONE',  ( 25.41429355638885212, -272.9947051449473179, -228.9882563095496835 ) ) ;
#42281 = ORIENTED_EDGE ( 'NONE', *, *, #58419, .T. ) ;
#42282 = CARTESIAN_POINT ( 'NONE',  ( 30.18390022370923731, -292.4123690577949901, -305.6702345193893393 ) ) ;
#42283 = CARTESIAN_POINT ( 'NONE',  ( -86.13673567776757523, -296.8609934912890935, -215.9825105417341433 ) ) ;
#42284 = CARTESIAN_POINT ( 'NONE',  ( 36.32395554261007220, -289.1168641302172659, -273.7728047627415435 ) ) ;
#42285 = CARTESIAN_POINT ( 'NONE',  ( 5.491607269823510329, -282.4012247385679188, -210.0015140351610228 ) ) ;
#42286 = CARTESIAN_POINT ( 'NONE',  ( -45.94128965665010611, -290.5842973735720989, -346.3391519802719927 ) ) ;
#42287 = CARTESIAN_POINT ( 'NONE',  ( -113.8759504293081477, -291.8922074113866074, -268.3842748251791477 ) ) ;
#42288 = CARTESIAN_POINT ( 'NONE',  ( -111.4712786417625523, -286.4017563327539051, -282.0868400082505332 ) ) ;
#42289 = CARTESIAN_POINT ( 'NONE',  ( -7.538949499501011786, -280.5988727940028866, -199.3482512648447198 ) ) ;
#42290 = ORIENTED_EDGE ( 'NONE', *, *, #40031, .F. ) ;
#42291 = CARTESIAN_POINT ( 'NONE',  ( 29.61479403485629547, -292.0923948850980310, -305.3774296770954493 ) ) ;
#42292 = CARTESIAN_POINT ( 'NONE',  ( 39.71045392701341825, -281.3801105752831404, -269.9323865911590588 ) ) ;
#42293 = CARTESIAN_POINT ( 'NONE',  ( 21.64889258855931686, -276.7890627938688226, -225.2738572682821996 ) ) ;
#42294 = EDGE_CURVE ( 'NONE', #74338, #66586, #55027, .T. ) ;
#42295 = CARTESIAN_POINT ( 'NONE',  ( 7.399455738971494334, -277.1948066931273047, -214.2051214447836571 ) ) ;
#42296 = VECTOR ( 'NONE', #36472, 1000.000000000000000 ) ;
#42297 = CARTESIAN_POINT ( 'NONE',  ( 36.91062037888140424, -273.9973579792975329, -286.5639148675630281 ) ) ;
#42298 = DIRECTION ( 'NONE',  ( -0.000000000000000000, -0.000000000000000000, -1.000000000000000000 ) ) ;
#42299 = CARTESIAN_POINT ( 'NONE',  ( 35.09465133165635109, -280.9291323441817099, -260.4472580575271650 ) ) ;
#42300 = CARTESIAN_POINT ( 'NONE',  ( -113.8346825827095330, -279.7056499331107489, -274.4638430257937216 ) ) ;
#42301 = CIRCLE ( 'NONE', #1484, 3.491568894204821749 ) ;
#42302 = CARTESIAN_POINT ( 'NONE',  ( -54.34175520056412978, -275.1443525508907442, -198.8611766951847528 ) ) ;
#42303 = CARTESIAN_POINT ( 'NONE',  ( -46.46560637000157357, -284.9977964188837518, -194.1405528607957081 ) ) ;
#42304 = CARTESIAN_POINT ( 'NONE',  ( -104.9645617908895616, -291.9113212542195583, -300.5728567032115279 ) ) ;
#42305 = CARTESIAN_POINT ( 'NONE',  ( -24.31661036425930433, -275.8157626102602649, -195.2289749244463337 ) ) ;
#42306 = CARTESIAN_POINT ( 'NONE',  ( -109.6413436277052540, -274.1847978990736010, -245.3399305201349421 ) ) ;
#42307 = CARTESIAN_POINT ( 'NONE',  ( 175.2296996224750103, 133.0000000000000000, 0.000000000000000000 ) ) ;
#42308 = CARTESIAN_POINT ( 'NONE',  ( -112.2089796716966106, -298.5734697482130855, -268.7174222125194660 ) ) ;
#42309 = CARTESIAN_POINT ( 'NONE',  ( -51.38634014322530419, -281.2318447437779128, -343.9175740812002005 ) ) ;
#42310 = CARTESIAN_POINT ( 'NONE',  ( -111.9730258420098323, -290.4555910380806267, -251.4424713074985220 ) ) ;
#42311 = CARTESIAN_POINT ( 'NONE',  ( 32.79884400571190639, -273.9067867190649963, -296.0484217280280177 ) ) ;
#42312 = CARTESIAN_POINT ( 'NONE',  ( 36.59559386667802983, -288.9192593325754501, -251.9297052691628664 ) ) ;
#42313 = CARTESIAN_POINT ( 'NONE',  ( -94.52341181032628015, -290.1183116424578543, -224.4665854958456919 ) ) ;
#42314 = ORIENTED_EDGE ( 'NONE', *, *, #73681, .T. ) ;
#42315 = CARTESIAN_POINT ( 'NONE',  ( -108.2584001906662365, -288.7630462449582751, -298.8115651460922777 ) ) ;
#42316 = CARTESIAN_POINT ( 'NONE',  ( -110.3276322273784444, -290.1721227383386008, -273.9057526129781195 ) ) ;
#42317 = ORIENTED_EDGE ( 'NONE', *, *, #23269, .T. ) ;
#42318 = CARTESIAN_POINT ( 'NONE',  ( 38.78547465501085867, -288.7537375978986915, -280.0703550040175855 ) ) ;
#42319 = CARTESIAN_POINT ( 'NONE',  ( -96.10749623106048034, -278.2778698193772584, -313.7256870808129179 ) ) ;
#42320 = CARTESIAN_POINT ( 'NONE',  ( -13.88969348611722943, -293.6751192062753830, -343.3782111430602413 ) ) ;
#42321 = CARTESIAN_POINT ( 'NONE',  ( -111.8534275305500074, -284.6428104518091118, -289.7458969499454042 ) ) ;
#42322 = CARTESIAN_POINT ( 'NONE',  ( -8.481980394220936859, -282.9969334636175518, -337.4372244864086952 ) ) ;
#42323 = CARTESIAN_POINT ( 'NONE',  ( -71.04534101611670849, -196.2794566099099995, -360.5068448367716769 ) ) ;
#42324 = CARTESIAN_POINT ( 'NONE',  ( 201.7737866479175750, 295.5635967683617196, -68.54576060224776768 ) ) ;
#42325 = CARTESIAN_POINT ( 'NONE',  ( 5.009449089156567503, -58.86080836571535713, -351.0592355680212222 ) ) ;
#42326 = CARTESIAN_POINT ( 'NONE',  ( -43.48551367926898337, -273.1698670285560411, -197.4072412621284229 ) ) ;
#42327 = CARTESIAN_POINT ( 'NONE',  ( -1.559789011583864404, -273.4586660888683696, -206.3633002098954989 ) ) ;
#42328 = CARTESIAN_POINT ( 'NONE',  ( -88.56913578991110114, -295.2554266174283839, -327.8370669536779474 ) ) ;
#42329 = CARTESIAN_POINT ( 'NONE',  ( 202.1135227227061364, 289.8103657602464978, -82.43770367997073834 ) ) ;
#42330 = CARTESIAN_POINT ( 'NONE',  ( -15.89941324210910167, -273.0085409260970550, -196.8654961622563349 ) ) ;
#42331 = CARTESIAN_POINT ( 'NONE',  ( -111.2828678737150057, -298.5054208216035931, -263.2037346356970602 ) ) ;
#42332 = CARTESIAN_POINT ( 'NONE',  ( -12.16691537103328180, -293.4671075416617896, -201.4560448007708544 ) ) ;
#42333 = ORIENTED_EDGE ( 'NONE', *, *, #46568, .T. ) ;
#42334 = CARTESIAN_POINT ( 'NONE',  ( -106.9479631355059013, -297.0778408655646103, -302.7306771767038072 ) ) ;
#42335 = CARTESIAN_POINT ( 'NONE',  ( 34.82099056833637007, -288.1961430047854265, -281.8660588170914707 ) ) ;
#42336 = CARTESIAN_POINT ( 'NONE',  ( 0.4699689440745843938, -295.3644352029350557, -337.2674955967511892 ) ) ;
#42337 = CARTESIAN_POINT ( 'NONE',  ( -50.45086305970222895, -295.7074471055738059, -346.2284531132146981 ) ) ;
#42338 = CARTESIAN_POINT ( 'NONE',  ( 31.80035113723905127, -293.4058135548237374, -246.7863298713807012 ) ) ;
#42339 = EDGE_LOOP ( 'NONE', ( #18780, #32200, #23130, #90074, #67636 ) ) ;
#42340 = CARTESIAN_POINT ( 'NONE',  ( 27.86581817928561478, -277.9786413101349467, -308.5356350356919393 ) ) ;
#42341 = EDGE_CURVE ( 'NONE', #12355, #11722, #78028, .T. ) ;
#42343 = VERTEX_POINT ( 'NONE', #65231 ) ;
#42342 = B_SPLINE_CURVE_WITH_KNOTS ( 'NONE', 3,
 ( #1180, #15859, #58026, #50903, #28213, #58488 ),
 .UNSPECIFIED., .F., .F.,
 ( 4, 2, 4 ),
 ( -4.472146915458784344E-06, 0.0004206930844425981289, 0.0008458583158006550539 ),
 .UNSPECIFIED. ) ;
#42344 = CARTESIAN_POINT ( 'NONE',  ( -114.1708897964509646, -278.0085002865974957, -274.4602054389801538 ) ) ;
#42345 = CARTESIAN_POINT ( 'NONE',  ( 32.32569665369121736, -276.7920182781443827, -292.9412480483022136 ) ) ;
#42346 = CARTESIAN_POINT ( 'NONE',  ( 30.33745307036346617, -276.8614041650806712, -235.8139584224055341 ) ) ;
#42347 = CARTESIAN_POINT ( 'NONE',  ( -96.97068175585063443, -297.7932241403557896, -228.0730910909286138 ) ) ;
#42348 = CARTESIAN_POINT ( 'NONE',  ( -110.3916744350586328, -295.0051563750857326, -279.6624581978121569 ) ) ;
#42349 = DIRECTION ( 'NONE',  ( -0.000000000000000000, -0.000000000000000000, 1.000000000000000000 ) ) ;
#42350 = CARTESIAN_POINT ( 'NONE',  ( -113.1768922274226270, -279.2069937476874770, -257.3784163155972919 ) ) ;
#42351 = CARTESIAN_POINT ( 'NONE',  ( -48.60574581701071395, -277.3661147383069761, -342.5382392165624879 ) ) ;
#42352 = CARTESIAN_POINT ( 'NONE',  ( 37.54428224780750867, -286.0390112312750261, -254.6327574638088151 ) ) ;
#42353 = CARTESIAN_POINT ( 'NONE',  ( -86.28822615237660898, -299.3754136867460147, -213.2463084346213122 ) ) ;
#42354 = DIRECTION ( 'NONE',  ( 0.000000000000000000, 1.000000000000000000, -0.000000000000000000 ) ) ;
#42355 = CARTESIAN_POINT ( 'NONE',  ( 3.696748015782929997, -287.6816985566318863, -330.9899108658565297 ) ) ;
#42356 = CARTESIAN_POINT ( 'NONE',  ( 14.05469148327361495, -279.0250687541832235, -217.0319533307971653 ) ) ;
#42357 = CARTESIAN_POINT ( 'NONE',  ( -43.78473630159547270, -278.5439990237646271, -197.0038471786520233 ) ) ;
#42359 = CARTESIAN_POINT ( 'NONE',  ( -47.03146446348424092, -287.9293704560428182, -195.9383397457096123 ) ) ;
#42358 = CIRCLE ( 'NONE', #31817, 5.000000000000000888 ) ;
#42360 = CARTESIAN_POINT ( 'NONE',  ( -61.90834894662256005, -278.5836759167299306, -339.5787949518490336 ) ) ;
#42361 = PLANE ( 'NONE',  #79083 ) ;
#42362 = CARTESIAN_POINT ( 'NONE',  ( -109.7085897907247869, -276.4948309697917921, -293.7041084104981792 ) ) ;
#42363 = AXIS2_PLACEMENT_3D ( 'NONE', #18452, #6135, #28385 ) ;
#42364 = CARTESIAN_POINT ( 'NONE',  ( 34.21942695004410240, -276.0060889641903827, -255.3702799987047172 ) ) ;
#42365 = CARTESIAN_POINT ( 'NONE',  ( 32.88398243018339429, -283.8999001097074597, -297.1637658701103533 ) ) ;
#42366 = DIRECTION ( 'NONE',  ( 0.000000000000000000, 0.000000000000000000, 1.000000000000000000 ) ) ;
#42367 = CARTESIAN_POINT ( 'NONE',  ( 31.56194128015845379, -289.8759331276331181, -301.3708325234615018 ) ) ;
#42368 = CARTESIAN_POINT ( 'NONE',  ( -31.72090765526752065, -290.1228095979524255, -195.5214087712234345 ) ) ;
#42369 = DIRECTION ( 'NONE',  ( -0.000000000000000000, -0.000000000000000000, 1.000000000000000000 ) ) ;
#42370 = CARTESIAN_POINT ( 'NONE',  ( -27.20570452537729622, -272.8683533986801422, -197.5190438051477031 ) ) ;
#42371 = CARTESIAN_POINT ( 'NONE',  ( 36.05564652922612368, -291.8403350076195011, -281.8166089304377238 ) ) ;
#42372 = CARTESIAN_POINT ( 'NONE',  ( 185.7741171649701926, 251.7621132184994508, -165.9827577097485118 ) ) ;
#42373 = CARTESIAN_POINT ( 'NONE',  ( 198.0449163674539079, 67.45573463390418567, -11.11900013380403962 ) ) ;
#42374 = CARTESIAN_POINT ( 'NONE',  ( -77.78549515300409212, -288.0643079586167801, -335.1298514573048237 ) ) ;
#42375 = CARTESIAN_POINT ( 'NONE',  ( -108.1538423715957578, -285.8797177728571342, -291.1927510768438196 ) ) ;
#42376 = CARTESIAN_POINT ( 'NONE',  ( 35.72316052809414089, -285.5247871268720701, -249.3054454384577241 ) ) ;
#42377 = CARTESIAN_POINT ( 'NONE',  ( -100.9009958447769293, -285.4724550515371675, -307.4500765017594972 ) ) ;
#42378 = CARTESIAN_POINT ( 'NONE',  ( -45.64766972519907284, -283.9628114373571179, -343.1006869732456153 ) ) ;
#42379 = CARTESIAN_POINT ( 'NONE',  ( -97.06056401540871548, -293.1588555032605541, -224.3830303256112302 ) ) ;
#42380 = CARTESIAN_POINT ( 'NONE',  ( 5.042938605749641034, -274.5638675266405357, -332.9139484170273136 ) ) ;
#42381 = CARTESIAN_POINT ( 'NONE',  ( -2.570892734687665548, -274.8325777617924928, -201.6679277018994583 ) ) ;
#42382 = CARTESIAN_POINT ( 'NONE',  ( -98.84446049999326078, -289.2245012691943202, -226.4666460520591045 ) ) ;
#42383 = CARTESIAN_POINT ( 'NONE',  ( -31.45026642415595219, -276.9798372843007428, -347.1880273555456142 ) ) ;
#42384 = CARTESIAN_POINT ( 'NONE',  ( -20.45203625092333866, -296.8142157503624503, -343.1233143870522326 ) ) ;
#42385 = FACE_OUTER_BOUND ( 'NONE', #61061, .T. ) ;
#42386 = CARTESIAN_POINT ( 'NONE',  ( 60.83730532400069535, -250.0090898647485176, -22.49999999999998579 ) ) ;
#42387 = CARTESIAN_POINT ( 'NONE',  ( -86.04048163229326462, -284.0454562775648810, -215.2506559664484200 ) ) ;
#42388 = CARTESIAN_POINT ( 'NONE',  ( 9.591820881458989589, -278.6971356682384453, -211.7945740586631871 ) ) ;
#42389 = CARTESIAN_POINT ( 'NONE',  ( 222.0386546523673985, 36.13108063356137478, -7.000000000000000888 ) ) ;
#42390 = CARTESIAN_POINT ( 'NONE',  ( 29.92970205765440284, -297.2809173091810635, -194.1790562426981239 ) ) ;
#42391 = CARTESIAN_POINT ( 'NONE',  ( -8.706383249097893184, -276.0158887314272533, -337.6347060179286927 ) ) ;
#42392 = CARTESIAN_POINT ( 'NONE',  ( -23.36857653014567049, -296.3905295839335281, -342.7696901447928894 ) ) ;
#42393 = CARTESIAN_POINT ( 'NONE',  ( 21.74139317677540006, -279.8125819635281459, -221.4665314059629964 ) ) ;
#42394 = CARTESIAN_POINT ( 'NONE',  ( -7.882696117460126217, -295.5976935185100274, -337.4237935270852518 ) ) ;
#42395 = EDGE_CURVE ( 'NONE', #28813, #34201, #64135, .T. ) ;
#42396 = CARTESIAN_POINT ( 'NONE',  ( -71.83660135248504730, -296.8137152771133174, -338.6502098201679587 ) ) ;
#42397 = CARTESIAN_POINT ( 'NONE',  ( -47.27064680046883183, -297.7559347124358169, -197.9882923834420865 ) ) ;
#42398 = CARTESIAN_POINT ( 'NONE',  ( -108.9177393926346582, -292.8417942542102423, -247.9153236157475533 ) ) ;
#42399 = CARTESIAN_POINT ( 'NONE',  ( -102.5196037710115320, -285.2556876483272958, -229.3630585015199870 ) ) ;
#42400 = CARTESIAN_POINT ( 'NONE',  ( -52.27854330543111416, -272.0025896527199620, -196.0297226417642662 ) ) ;
#42401 = CARTESIAN_POINT ( 'NONE',  ( 38.29058305408145202, -287.2047751234372299, -255.9126666753702182 ) ) ;
#42402 = CARTESIAN_POINT ( 'NONE',  ( -93.46133121964680868, -281.2191930362118342, -221.1234393951787069 ) ) ;
#42403 = EDGE_CURVE ( 'NONE', #37341, #32542, #59502, .T. ) ;
#42404 = CARTESIAN_POINT ( 'NONE',  ( -41.32377650584606954, -285.0595677206560481, -197.2216244785268771 ) ) ;
#42405 = CARTESIAN_POINT ( 'NONE',  ( -79.43963163530425220, -287.6200394192532599, -332.4945149792881125 ) ) ;
#42406 = CARTESIAN_POINT ( 'NONE',  ( 197.9739649220119588, 291.4634315377682583, -67.91333382494548232 ) ) ;
#42407 = CARTESIAN_POINT ( 'NONE',  ( 35.33625001697656387, -286.9612525715483002, -262.8842199427909918 ) ) ;
#42408 = CARTESIAN_POINT ( 'NONE',  ( 13.53384431242066555, -283.3017363432580282, -327.9166570225073087 ) ) ;
#42409 = CARTESIAN_POINT ( 'NONE',  ( -42.02758827201233771, -291.0531947517390563, -193.7395631467328485 ) ) ;
#42410 = CARTESIAN_POINT ( 'NONE',  ( -61.81023454774331327, -281.3396145714237377, -198.1408521450441640 ) ) ;
#42411 = CARTESIAN_POINT ( 'NONE',  ( -113.7195135901158949, -279.9232309594380581, -265.9195098998526419 ) ) ;
#42412 = CARTESIAN_POINT ( 'NONE',  ( 26.45986893634234605, -280.9004665539023335, -234.8877506571367917 ) ) ;
#42413 = CARTESIAN_POINT ( 'NONE',  ( 37.34799268838678898, -277.6398253032924117, -277.1765735041109906 ) ) ;
#42414 = CARTESIAN_POINT ( 'NONE',  ( -16.50687936599918970, -294.7902771600710707, -344.5440125573325645 ) ) ;
#42415 = CARTESIAN_POINT ( 'NONE',  ( -20.78857403068984055, -286.8587213615697920, -343.1473860278132406 ) ) ;
#42416 = CARTESIAN_POINT ( 'NONE',  ( -107.7524451484439254, -295.7412925800470589, -249.9514864393960920 ) ) ;
#42417 = ORIENTED_EDGE ( 'NONE', *, *, #41382, .T. ) ;
#42418 = ORIENTED_EDGE ( 'NONE', *, *, #27281, .T. ) ;
#42419 = CARTESIAN_POINT ( 'NONE',  ( -7.902694791021886545, -284.5835498985225058, -338.7325971581332169 ) ) ;
#42420 = CARTESIAN_POINT ( 'NONE',  ( -94.79270246972060932, -295.5834966995126933, -315.4329475085029912 ) ) ;
#42421 = CARTESIAN_POINT ( 'NONE',  ( 38.54397403782432008, -294.4881709102701279, -258.9211454097292631 ) ) ;
#42422 = CARTESIAN_POINT ( 'NONE',  ( -80.67990542881109661, -284.3087377346972744, -329.2942258662741324 ) ) ;
#42423 = CARTESIAN_POINT ( 'NONE',  ( -7.770104050997200140, -273.4889504037163306, -199.4644398280292421 ) ) ;
#42424 = CARTESIAN_POINT ( 'NONE',  ( -80.47656587688828722, -290.2711861293694824, -334.0862302019627350 ) ) ;
#42425 = CARTESIAN_POINT ( 'NONE',  ( -34.54861462927985372, -281.1569840664961930, -346.0744203545301616 ) ) ;
#42426 = VECTOR ( 'NONE', #20060, 1000.000000000000000 ) ;
#42427 = CARTESIAN_POINT ( 'NONE',  ( -101.6686282695899024, -291.4424893707802653, -227.9831831999890710 ) ) ;
#42428 = CARTESIAN_POINT ( 'NONE',  ( 34.78077425787379440, -288.0371026675803705, -281.8616965868361603 ) ) ;
#42429 = LINE ( 'NONE', #21133, #56543 ) ;
#42430 = CARTESIAN_POINT ( 'NONE',  ( 153.0292788520805232, 130.2722548028652909, -11.54371207238995645 ) ) ;
#42431 = CARTESIAN_POINT ( 'NONE',  ( 25.57469608755605961, -24.14966140349115875, -341.3741087935360383 ) ) ;
#42432 = CIRCLE ( 'NONE', #30338, 2.000000000000010658 ) ;
#42433 = CARTESIAN_POINT ( 'NONE',  ( -4.829096099716524648, -286.1237833571632905, -337.9475929042657754 ) ) ;
#42434 = ORIENTED_EDGE ( 'NONE', *, *, #42126, .T. ) ;
#42435 = CARTESIAN_POINT ( 'NONE',  ( -4.195556142615309625, -279.4200995118495712, -204.9594066443358713 ) ) ;
#42436 = CARTESIAN_POINT ( 'NONE',  ( -32.67964170847187688, -273.7760883626745567, -193.5104183097055852 ) ) ;
#42437 = CARTESIAN_POINT ( 'NONE',  ( -98.36633488680406856, -279.9620341449951297, -313.6964367216176583 ) ) ;
#42438 = CARTESIAN_POINT ( 'NONE',  ( 203.1614497710260707, 290.3320369869807109, -82.66081499759458495 ) ) ;
#42439 = CARTESIAN_POINT ( 'NONE',  ( 36.97104023705923481, -280.3516544767687719, -288.1995297295993623 ) ) ;
#42440 = CARTESIAN_POINT ( 'NONE',  ( 8.791148951116039001, -280.4366319136524339, -329.1093686124274313 ) ) ;
#42441 = CARTESIAN_POINT ( 'NONE',  ( -110.6505008171513538, -298.5682850794868273, -250.1716295355531656 ) ) ;
#42442 = CARTESIAN_POINT ( 'NONE',  ( 34.89978769456786267, -294.1927184156310773, -281.6062306115200613 ) ) ;
#42443 = VERTEX_POINT ( 'NONE', #48312 ) ;
#42444 = CARTESIAN_POINT ( 'NONE',  ( -79.80206140066704279, -290.1497094277491442, -210.3124076780740381 ) ) ;
#42445 = CARTESIAN_POINT ( 'NONE',  ( 19.95436720214620507, -275.5063312634803196, -218.9947344057348744 ) ) ;
#42446 = CARTESIAN_POINT ( 'NONE',  ( -83.19058505835093342, -273.4036441152288148, -213.5554866538713270 ) ) ;
#42447 = ORIENTED_EDGE ( 'NONE', *, *, #48576, .F. ) ;
#42448 = DIRECTION ( 'NONE',  ( 1.124465274301078281E-16, 1.000000000000000000, -0.000000000000000000 ) ) ;
#42449 = FACE_OUTER_BOUND ( 'NONE', #21985, .T. ) ;
#42450 = CARTESIAN_POINT ( 'NONE',  ( 194.3144103428324172, 249.5000000000000568, 16.91223866672520515 ) ) ;
#42451 = CARTESIAN_POINT ( 'NONE',  ( -66.20401008319879566, -280.7449299340070183, -202.9590445077823802 ) ) ;
#42452 = CARTESIAN_POINT ( 'NONE',  ( -4.121137745965621768, -282.2442633692047025, -202.0067007805730555 ) ) ;
#42453 = CARTESIAN_POINT ( 'NONE',  ( -108.9526602651009455, -283.4084199611544364, -285.7595257860030529 ) ) ;
#42454 = CARTESIAN_POINT ( 'NONE',  ( -11.33220374933405239, -282.2549389893032412, -200.7771188105159865 ) ) ;
#42455 = CARTESIAN_POINT ( 'NONE',  ( 36.33648845465727817, -274.0124985707211067, -268.8670370939927921 ) ) ;
#42456 = EDGE_CURVE ( 'NONE', #9812, #19395, #37993, .T. ) ;
#42457 = LINE ( 'NONE', #91239, #89590 ) ;
#42458 = ADVANCED_FACE ( 'NONE', ( #77213 ), #33182, .F. ) ;
#42459 = DIRECTION ( 'NONE',  ( 0.000000000000000000, 0.000000000000000000, 1.000000000000000000 ) ) ;
#42460 = CARTESIAN_POINT ( 'NONE',  ( -48.46049489216986217, -277.9929427585155395, -346.4447032779111737 ) ) ;
#42461 = VERTEX_POINT ( 'NONE', #91401 ) ;
#42462 = ORIENTED_EDGE ( 'NONE', *, *, #55666, .F. ) ;
#42463 = DIRECTION ( 'NONE',  ( 0.000000000000000000, 0.000000000000000000, 1.000000000000000000 ) ) ;
#42464 = CARTESIAN_POINT ( 'NONE',  ( -38.67755565546019625, -285.0487173313849212, -345.7044806404859969 ) ) ;
#42465 = CARTESIAN_POINT ( 'NONE',  ( 35.78304895597343460, -292.7188047607918975, -268.0431883363229417 ) ) ;
#42466 = CARTESIAN_POINT ( 'NONE',  ( -4.384282607917082686, -287.9777280974648761, -339.8530659658521245 ) ) ;
#42467 = CARTESIAN_POINT ( 'NONE',  ( -108.3204279705254294, -283.0678573580605644, -249.2075155727910385 ) ) ;
#42469 = CARTESIAN_POINT ( 'NONE',  ( -45.49604767983542075, -287.3967462372113459, -343.9238845749121083 ) ) ;
#42468 = CARTESIAN_POINT ( 'NONE',  ( -49.50115984828789806, -284.4689485472754313, -197.7315063751577497 ) ) ;
#42470 = CARTESIAN_POINT ( 'NONE',  ( 5.838006246322387405, -283.6569663060549260, -329.7129794628483523 ) ) ;
#42471 = CARTESIAN_POINT ( 'NONE',  ( 20.32972382687431789, -272.8899438423821948, -222.4131512750598461 ) ) ;
#42472 = CARTESIAN_POINT ( 'NONE',  ( -112.3531629457156384, -282.7789410388660372, -284.0572552147507395 ) ) ;
#42473 = CARTESIAN_POINT ( 'NONE',  ( -95.83128075245272726, -297.9062562714833575, -317.3278898714050342 ) ) ;
#42474 = CARTESIAN_POINT ( 'NONE',  ( -31.01222614726124860, -284.1317716816291181, -195.4484320985835382 ) ) ;
#42475 = CARTESIAN_POINT ( 'NONE',  ( -92.39320718732552962, -280.1807206404401995, -222.0435897916533463 ) ) ;
#42476 = CARTESIAN_POINT ( 'NONE',  ( 8.667988948866881316, -288.6812277524787191, -210.9209216966050917 ) ) ;
#42477 = CARTESIAN_POINT ( 'NONE',  ( 195.6227410709891501, 26.52170211303658576, 13.75379487587555438 ) ) ;
#42478 = DIRECTION ( 'NONE',  ( 0.5335274993777835428, -0.8457827187922967171, 0.000000000000000000 ) ) ;
#42479 = CARTESIAN_POINT ( 'NONE',  ( 36.94609038373248922, -295.6491640990642509, -284.2383344620357661 ) ) ;
#42480 = CARTESIAN_POINT ( 'NONE',  ( -100.8827153437524657, -276.0153548599132023, -310.3021231736551613 ) ) ;
#42481 = CARTESIAN_POINT ( 'NONE',  ( -109.3189808297879750, -290.0919167419311862, -243.3128910110611116 ) ) ;
#42482 = CARTESIAN_POINT ( 'NONE',  ( -10.21469398820136831, -293.0919215033308092, -338.9946808617684724 ) ) ;
#42483 = CARTESIAN_POINT ( 'NONE',  ( -104.8887827829167065, -277.6233996011955583, -241.4019207983978106 ) ) ;
#42484 = CARTESIAN_POINT ( 'NONE',  ( -97.42953907880669817, -271.2364393961005931, -226.3350328184559999 ) ) ;
#42485 = CARTESIAN_POINT ( 'NONE',  ( -106.1784018442980937, -292.2101778352040355, -244.4726537207301931 ) ) ;
#42486 = CARTESIAN_POINT ( 'NONE',  ( -4.771743288812468897, -285.1233781216987495, -337.9199732462171255 ) ) ;
#42487 = CARTESIAN_POINT ( 'NONE',  ( -14.01258554482040708, -293.2347395927417324, -343.0141300620367133 ) ) ;
#42488 = CARTESIAN_POINT ( 'NONE',  ( -94.71348264742380252, -291.5027692296777104, -316.7822229693273357 ) ) ;
#42489 = CARTESIAN_POINT ( 'NONE',  ( 35.32457609781123864, -291.5093369746655867, -248.1443154795454120 ) ) ;
#42490 = CARTESIAN_POINT ( 'NONE',  ( -102.9430045682343433, -292.4279951046752331, -236.9039410442110523 ) ) ;
#42491 = DIRECTION ( 'NONE',  ( 0.000000000000000000, 1.000000000000000000, 0.000000000000000000 ) ) ;
#42492 = CARTESIAN_POINT ( 'NONE',  ( -18.42190869602884362, -289.6050660920769815, -341.0866118805447513 ) ) ;
#42493 = CARTESIAN_POINT ( 'NONE',  ( 195.5378547391706263, 20.94045493971685090, 14.59381989330956131 ) ) ;
#42494 = CARTESIAN_POINT ( 'NONE',  ( -113.9926312953178353, -291.7461829576876653, -271.2395999151335673 ) ) ;
#42496 = CARTESIAN_POINT ( 'NONE',  ( -12.26020631080762868, -292.3876102128842263, -201.7512875080602157 ) ) ;
#42495 = CARTESIAN_POINT ( 'NONE',  ( 38.06466923558203774, -279.5671901812859232, -269.9646359496893524 ) ) ;
#42497 = CARTESIAN_POINT ( 'NONE',  ( -2.390141635068330661, -280.5016501009009176, -201.7359788623843428 ) ) ;
#42498 = AXIS2_PLACEMENT_3D ( 'NONE', #22389, #7260, #79699 ) ;
#42499 = CARTESIAN_POINT ( 'NONE',  ( 24.23563647454788494, -281.8338757631203748, -316.5560950745872333 ) ) ;
#42500 = CARTESIAN_POINT ( 'NONE',  ( 28.12527861860371914, -285.0635795148411944, -233.6614189914476469 ) ) ;
#42501 = CARTESIAN_POINT ( 'NONE',  ( 31.17042443314550937, -279.3147150633383831, -241.7787061532553423 ) ) ;
#42502 = CARTESIAN_POINT ( 'NONE',  ( -109.7826122830774551, -282.8039599091048331, -250.7415842636285390 ) ) ;
#42503 = FACE_OUTER_BOUND ( 'NONE', #31457, .T. ) ;
#42504 = CARTESIAN_POINT ( 'NONE',  ( -64.47750154657505561, -278.1843143148682316, -198.9867079554612985 ) ) ;
#42505 = CARTESIAN_POINT ( 'NONE',  ( -75.93920986785983018, -284.4700130524016686, -204.0298806287281934 ) ) ;
#42506 = CARTESIAN_POINT ( 'NONE',  ( -32.69095757330136109, -274.9150655198245659, -197.3350561345241658 ) ) ;
#42507 = CYLINDRICAL_SURFACE ( 'NONE', #80903, 4.000000000000003553 ) ;
#42508 = CARTESIAN_POINT ( 'NONE',  ( 34.72666839505038183, -294.9441368203573006, -254.4096540843970899 ) ) ;
#42509 = CARTESIAN_POINT ( 'NONE',  ( -36.96103440260684891, -275.4821281253670122, -193.9383408897356276 ) ) ;
#42510 = CARTESIAN_POINT ( 'NONE',  ( -97.66868864158274732, -277.6466347378795945, -311.5040632305970689 ) ) ;
#42511 = CARTESIAN_POINT ( 'NONE',  ( -106.5125782799321001, -290.2830593939783057, -304.3111369788155685 ) ) ;
#42512 = CARTESIAN_POINT ( 'NONE',  ( -4.265463125965251123, -278.5645641888096407, -202.4110404023321905 ) ) ;
#42513 = CARTESIAN_POINT ( 'NONE',  ( 17.49109674441720585, -292.6423632383825293, -216.2271383537219265 ) ) ;
#42514 = ADVANCED_FACE ( 'NONE', ( #61613 ), #39323, .T. ) ;
#42515 = CARTESIAN_POINT ( 'NONE',  ( -103.7647076125308843, -290.0259248478650420, -239.5164665159246056 ) ) ;
#42516 = CARTESIAN_POINT ( 'NONE',  ( 19.82621375535443065, -292.2238954035275924, -318.9083143378635441 ) ) ;
#42517 = EDGE_LOOP ( 'NONE', ( #7535, #68727, #90919, #57380 ) ) ;
#42518 = CARTESIAN_POINT ( 'NONE',  ( 153.6987871352777404, 19.48326534539592103, 11.45812909364015297 ) ) ;
#42519 = CARTESIAN_POINT ( 'NONE',  ( -65.34475253577710419, -291.1836363983406386, -202.8656139963957230 ) ) ;
#42520 = CARTESIAN_POINT ( 'NONE',  ( 30.91033621190086578, -278.8380690714489560, -254.8156830097664738 ) ) ;
#42521 = CARTESIAN_POINT ( 'NONE',  ( -110.1264353503709401, -295.3027528842199558, -294.7578909529135558 ) ) ;
#42522 = CARTESIAN_POINT ( 'NONE',  ( -81.26465132796487012, -284.9503086261767066, -333.0679782429864417 ) ) ;
#42523 = CARTESIAN_POINT ( 'NONE',  ( -2.184521322503762519, -286.3642642267885208, -206.3280554522691830 ) ) ;
#42524 = CARTESIAN_POINT ( 'NONE',  ( 12.22825554471529408, -277.8678339576953249, -324.9604371279157249 ) ) ;
#42525 = CARTESIAN_POINT ( 'NONE',  ( -74.13461051777825617, -293.5638124406008274, -335.3082391557379083 ) ) ;
#42526 = CARTESIAN_POINT ( 'NONE',  ( -95.55677961956858724, -297.6765801856430471, -316.0664627061902934 ) ) ;
#42527 = EDGE_CURVE ( 'NONE', #46265, #40166, #71684, .T. ) ;
#42528 = CARTESIAN_POINT ( 'NONE',  ( 22.78232720893039698, -274.9320457407357594, -312.5462334195946710 ) ) ;
#42529 = ORIENTED_EDGE ( 'NONE', *, *, #1899, .F. ) ;
#42530 = FACE_BOUND ( 'NONE', #61996, .T. ) ;
#42531 = CARTESIAN_POINT ( 'NONE',  ( -109.8295243780542876, -296.5460091089748857, -244.4524393790357237 ) ) ;
#42532 = CARTESIAN_POINT ( 'NONE',  ( 13.15015081751855597, -290.2605204887556738, -325.1293301925349510 ) ) ;
#42533 = DIRECTION ( 'NONE',  ( 1.000000000000000000, 0.000000000000000000, 0.000000000000000000 ) ) ;
#42534 = CARTESIAN_POINT ( 'NONE',  ( 21.26016509809543109, -288.8161046337660878, -314.0823504299175966 ) ) ;
#42535 = ORIENTED_EDGE ( 'NONE', *, *, #41498, .F. ) ;
#42536 = CARTESIAN_POINT ( 'NONE',  ( -14.28696721684780080, -279.4026026725536553, -197.0844904720465536 ) ) ;
#42537 = CARTESIAN_POINT ( 'NONE',  ( -13.80534638719844942, -295.4059249580225810, -343.5687189468729343 ) ) ;
#42538 = CARTESIAN_POINT ( 'NONE',  ( -73.85319858481622646, -287.6712070385224251, -336.7627981140441875 ) ) ;
#42539 = CARTESIAN_POINT ( 'NONE',  ( -104.5823670025761913, -296.3982141380537314, -307.9458956226947635 ) ) ;
#42540 = CARTESIAN_POINT ( 'NONE',  ( 32.36825079043457976, -294.1734330795222832, -292.1007184785422055 ) ) ;
#42541 = FACE_OUTER_BOUND ( 'NONE', #23189, .T. ) ;
#42542 = CARTESIAN_POINT ( 'NONE',  ( 196.4364563510924881, 72.07553028462349687, -11.29011490108475080 ) ) ;
#42543 = FACE_OUTER_BOUND ( 'NONE', #49886, .T. ) ;
#42544 = CARTESIAN_POINT ( 'NONE',  ( -57.09260349216318531, -290.8224297304331571, -344.1219610217855802 ) ) ;
#42545 = CARTESIAN_POINT ( 'NONE',  ( -55.56934967048407970, -295.3380690714490129, -190.3538533559490702 ) ) ;
#42546 = EDGE_LOOP ( 'NONE', ( #51648, #39510, #84338, #61742 ) ) ;
#42547 = CARTESIAN_POINT ( 'NONE',  ( -38.16048880506484409, -279.3907338161644134, -193.4674097080047375 ) ) ;
#42548 = CARTESIAN_POINT ( 'NONE',  ( -71.01769606448635841, -285.4976827002761297, -337.2032521700472785 ) ) ;
#42549 = CARTESIAN_POINT ( 'NONE',  ( -32.32682456429676421, -284.6889262500657196, -194.1020210459960254 ) ) ;
#42550 = CARTESIAN_POINT ( 'NONE',  ( 20.61961945506797633, -286.2796624455659753, -317.0708560901406372 ) ) ;
#42551 = CARTESIAN_POINT ( 'NONE',  ( -23.14671025493263556, -278.7330267318222923, -344.8376029907565226 ) ) ;
#42552 = VERTEX_POINT ( 'NONE', #26072 ) ;
#42554 = CARTESIAN_POINT ( 'NONE',  ( -92.27956894233068397, -278.5883127697608188, -222.1163255152069667 ) ) ;
#42553 = CARTESIAN_POINT ( 'NONE',  ( -76.35581941721268606, -277.5894237337617483, -332.1206373169924859 ) ) ;
#42555 = CARTESIAN_POINT ( 'NONE',  ( 24.22347928239249271, -276.0213114192907256, -224.6312459652183406 ) ) ;
#42556 = CARTESIAN_POINT ( 'NONE',  ( -90.77016909999454697, -278.1099401161383184, -215.3926723503662970 ) ) ;
#42557 = CARTESIAN_POINT ( 'NONE',  ( 197.5292130366077856, 288.3118105299622584, -96.80481239046156361 ) ) ;
#42558 = CARTESIAN_POINT ( 'NONE',  ( -87.89047171050665952, -274.3071897815528359, -212.5181075685498797 ) ) ;
#42559 = CARTESIAN_POINT ( 'NONE',  ( -37.62384221459190314, -299.4739495959235569, -193.9508654540946111 ) ) ;
#42560 = CARTESIAN_POINT ( 'NONE',  ( -106.6379572354042296, -286.6233781216988064, -303.7686719486574702 ) ) ;
#42561 = CARTESIAN_POINT ( 'NONE',  ( 82.66356608220550584, -298.4024577471378166, -193.1360764112615982 ) ) ;
#42562 = MECHANICAL_DESIGN_GEOMETRIC_PRESENTATION_REPRESENTATION (  '', ( #18373 ), #15346 ) ;
#42563 = CARTESIAN_POINT ( 'NONE',  ( -10.65018257429869308, -287.4883265503664234, -202.0702413516283684 ) ) ;
#42564 = CARTESIAN_POINT ( 'NONE',  ( -40.79318215999495578, -287.7695687098921553, -194.4013701814462536 ) ) ;
#42565 = CARTESIAN_POINT ( 'NONE',  ( 12.21882348805063501, -287.6893672464220799, -324.1667274881333469 ) ) ;
#42566 = CARTESIAN_POINT ( 'NONE',  ( -61.21853497581030012, -282.8615899978443622, -343.5565139582915890 ) ) ;
#42567 = CARTESIAN_POINT ( 'NONE',  ( -39.70667593311462440, -278.4218615285074634, -196.5863614139851165 ) ) ;
#42568 = CARTESIAN_POINT ( 'NONE',  ( 15.89914735725999151, -288.6769859940899323, -218.6283658915252204 ) ) ;
#42569 = CARTESIAN_POINT ( 'NONE',  ( 35.72280838892917387, -279.9015233371092108, -260.3744474690736865 ) ) ;
#42570 = EDGE_CURVE ( 'NONE', #13568, #49791, #3364, .T. ) ;
#42571 = CARTESIAN_POINT ( 'NONE',  ( 9.994378199043083555, -277.6988324975472437, -326.5797907277363947 ) ) ;
#42572 = CARTESIAN_POINT ( 'NONE',  ( 25.43164424310218763, -276.5580179711071196, -307.7442114608942916 ) ) ;
#42573 = CARTESIAN_POINT ( 'NONE',  ( -77.93905190224344892, -288.3793034123935399, -335.3834796541093510 ) ) ;
#42574 = CIRCLE ( 'NONE', #281, 5.025000000000002132 ) ;
#42575 = CARTESIAN_POINT ( 'NONE',  ( -33.05750822365979502, -283.8023386265159047, -347.0932224889459121 ) ) ;
#42576 = CARTESIAN_POINT ( 'NONE',  ( -61.20662319587470535, -283.8461257744933164, -343.5603980248732796 ) ) ;
#42577 = CARTESIAN_POINT ( 'NONE',  ( 11.30424099245688652, -280.9157324153339346, -215.9316000994883495 ) ) ;
#42578 = EDGE_LOOP ( 'NONE', ( #17509, #31513, #21283, #41007 ) ) ;
#42579 = EDGE_LOOP ( 'NONE', ( #23946, #24064, #39386, #44636 ) ) ;
#42580 = FACE_OUTER_BOUND ( 'NONE', #41493, .T. ) ;
#42581 = CARTESIAN_POINT ( 'NONE',  ( -86.56368792329394068, -291.5875671768767461, -328.0277636718988106 ) ) ;
#42582 = CARTESIAN_POINT ( 'NONE',  ( -67.87256616255660902, -288.1294418634895464, -340.5121300422136983 ) ) ;
#42583 = CARTESIAN_POINT ( 'NONE',  ( -99.47378243058825831, -272.1442836178328548, -231.5924089939479984 ) ) ;
#42584 = CARTESIAN_POINT ( 'NONE',  ( 37.66372760493411675, -292.6877388643204654, -253.3462670035110875 ) ) ;
#42585 = CARTESIAN_POINT ( 'NONE',  ( -64.09044247684056472, -287.8872571468643855, -339.0832292362473481 ) ) ;
#42586 = CARTESIAN_POINT ( 'NONE',  ( 34.75752506226930194, -292.0102569731087101, -287.1403857160945563 ) ) ;
#42587 = CARTESIAN_POINT ( 'NONE',  ( 34.67673903866996454, -288.9438535386589706, -284.5850729517826494 ) ) ;
#42588 = CARTESIAN_POINT ( 'NONE',  ( 31.98288692825981272, -296.4805209788415823, -303.7098442033569654 ) ) ;
#42589 = CARTESIAN_POINT ( 'NONE',  ( 9.012370294954282102, -290.4166657428516487, -329.3873684085881450 ) ) ;
#42590 = CARTESIAN_POINT ( 'NONE',  ( -112.5559253764166812, -288.5414624975909419, -271.1826781763828649 ) ) ;
#42591 = CARTESIAN_POINT ( 'NONE',  ( -48.27292950850284114, -293.9133395085021334, -196.1101237109748467 ) ) ;
#42592 = CARTESIAN_POINT ( 'NONE',  ( -93.59513383851965784, -284.8301283410953033, -317.2541840434030860 ) ) ;
#42593 = CARTESIAN_POINT ( 'NONE',  ( -33.65537278147974831, -294.0986121196559111, -195.2848939226211940 ) ) ;
#42594 = CARTESIAN_POINT ( 'NONE',  ( -114.1561780732172480, -273.4200912208958130, -270.3721689257164940 ) ) ;
#42595 = CARTESIAN_POINT ( 'NONE',  ( 222.4306832106270804, -141.7221692137691775, 21.50000000000000000 ) ) ;
#42596 = CARTESIAN_POINT ( 'NONE',  ( -66.91389818336824646, -275.6464130736508764, -201.0510039518020449 ) ) ;
#42597 = CARTESIAN_POINT ( 'NONE',  ( -32.14441068128075329, -282.1820803459872877, -343.3377574606344638 ) ) ;
#42598 = CARTESIAN_POINT ( 'NONE',  ( -0.2854021067749158425, -280.5591494292785342, -335.5671869221244492 ) ) ;
#42599 = CARTESIAN_POINT ( 'NONE',  ( -88.50554834642690594, -294.9449912121329476, -327.7597775610984172 ) ) ;
#42600 = CARTESIAN_POINT ( 'NONE',  ( 34.82678483088223231, -273.5776771163112926, -253.8823245216564999 ) ) ;
#42601 = CARTESIAN_POINT ( 'NONE',  ( -111.3960647627474003, -276.7362591262742626, -262.3012767681219657 ) ) ;
#42602 = CARTESIAN_POINT ( 'NONE',  ( -110.7055576525951039, -297.9244301265383683, -266.0036088324801540 ) ) ;
#42603 = CARTESIAN_POINT ( 'NONE',  ( 30.73363665616459883, -273.6765033344636322, -235.6573024427248697 ) ) ;
#42604 = CARTESIAN_POINT ( 'NONE',  ( -67.52038575554564659, -296.8812532099888131, -337.4914125938276470 ) ) ;
#42605 = DIRECTION ( 'NONE',  ( 0.000000000000000000, 0.000000000000000000, 1.000000000000000000 ) ) ;
#42606 = CARTESIAN_POINT ( 'NONE',  ( -96.53304938826724424, -296.7542684128148949, -313.3823332750778263 ) ) ;
#42607 = DIRECTION ( 'NONE',  ( -1.000000000000000000, -0.000000000000000000, -0.000000000000000000 ) ) ;
#42609 = CARTESIAN_POINT ( 'NONE',  ( -37.82251735037001339, -298.0459637686756764, -197.3627014600165239 ) ) ;
#42608 = CARTESIAN_POINT ( 'NONE',  ( 24.21634886488942939, -284.9843362706011476, -226.8760791316890959 ) ) ;
#42610 = CARTESIAN_POINT ( 'NONE',  ( -9.993960832771835001, -286.3994108159059806, -198.3244508398656478 ) ) ;
#42611 = CARTESIAN_POINT ( 'NONE',  ( 7.918650267466007087, -288.1195259727757048, -332.6943760447730369 ) ) ;
#42612 = CARTESIAN_POINT ( 'NONE',  ( -112.7201997012685837, -298.5053538625817851, -272.4499071714736829 ) ) ;
#42613 = CARTESIAN_POINT ( 'NONE',  ( 37.54242783184480459, -291.5575744174519741, -270.7953604001459098 ) ) ;
#42614 = CARTESIAN_POINT ( 'NONE',  ( -33.91222804012959813, -279.2914393933908173, -193.5991642423914811 ) ) ;
#42615 = CARTESIAN_POINT ( 'NONE',  ( 31.95455697924147387, -291.4809262143061801, -303.7686719486574134 ) ) ;
#42616 = DIRECTION ( 'NONE',  ( 0.000000000000000000, 0.000000000000000000, 1.000000000000000000 ) ) ;
#42617 = CARTESIAN_POINT ( 'NONE',  ( -1.981687420488145390, -285.3260362426477741, -205.9861276708301148 ) ) ;
#42618 = CARTESIAN_POINT ( 'NONE',  ( 196.8803347170859865, 73.40565171261611965, -12.50000000000000178 ) ) ;
#42619 = CARTESIAN_POINT ( 'NONE',  ( -103.4168970293110306, -288.0797640049244137, -305.9546600654516055 ) ) ;
#42620 = CARTESIAN_POINT ( 'NONE',  ( -37.84823625288498761, -299.6458330807033121, -196.5628535124512268 ) ) ;
#42621 = CARTESIAN_POINT ( 'NONE',  ( -3.931759451526023241, -281.9094486853182389, -201.6271221130625690 ) ) ;
#42623 = CARTESIAN_POINT ( 'NONE',  ( 9.908696275385604935, -282.3801926386418018, -326.0728993574523997 ) ) ;
#42622 = CARTESIAN_POINT ( 'NONE',  ( -92.44245509465827126, -295.2890533444373773, -218.8815948689192794 ) ) ;
#42624 = CARTESIAN_POINT ( 'NONE',  ( -91.63703121313025690, -297.4708200152910536, -215.7624272760778581 ) ) ;
#42625 = CARTESIAN_POINT ( 'NONE',  ( -33.78935643706599024, -299.6175343049769140, -196.6668402802768014 ) ) ;
#42626 = CARTESIAN_POINT ( 'NONE',  ( 37.70894528338921958, -283.5466024423273552, -269.9160369944169702 ) ) ;
#42627 = CARTESIAN_POINT ( 'NONE',  ( -110.3348058049926266, -295.5247977681781890, -276.9087912148806936 ) ) ;
#42628 = AXIS2_PLACEMENT_3D ( 'NONE', #52357, #32809, #90531 ) ;
#42629 = ORIENTED_EDGE ( 'NONE', *, *, #88532, .T. ) ;
#42630 = DIRECTION ( 'NONE',  ( 0.000000000000000000, 0.000000000000000000, 1.000000000000000000 ) ) ;
#42632 = CARTESIAN_POINT ( 'NONE',  ( -65.92267374842099059, -285.4078138589302966, -339.3313455811912149 ) ) ;
#42631 = AXIS2_PLACEMENT_3D ( 'NONE', #5378, #92445, #20025 ) ;
#42633 = CARTESIAN_POINT ( 'NONE',  ( 104.1717476309105166, -299.5541904835127980, -197.7570935515975350 ) ) ;
#42634 = CARTESIAN_POINT ( 'NONE',  ( 35.77081079830085031, -291.2666405000204577, -287.0812184334320705 ) ) ;
#42635 = CARTESIAN_POINT ( 'NONE',  ( 37.48002216566043643, -274.5294865096090575, -252.8147467647210931 ) ) ;
#42636 = CARTESIAN_POINT ( 'NONE',  ( -34.85515696084014081, -291.9175750985450009, -197.4034788513308456 ) ) ;
#42637 = AXIS2_PLACEMENT_3D ( 'NONE', #89058, #17119, #24207 ) ;
#42638 = CARTESIAN_POINT ( 'NONE',  ( 9.704430016058637420, -282.2331093358340013, -213.5727527777936245 ) ) ;
#42639 = CARTESIAN_POINT ( 'NONE',  ( -7.162059756873111915, -278.2496160505488092, -337.7082019881324868 ) ) ;
#42640 = CARTESIAN_POINT ( 'NONE',  ( -106.4648393807225233, -285.5570400589816700, -302.9279402276478095 ) ) ;
#42641 = CARTESIAN_POINT ( 'NONE',  ( 24.02290014644300342, -279.7907373501017787, -230.0013787271210504 ) ) ;
#42642 = CARTESIAN_POINT ( 'NONE',  ( -99.28672050622678569, -279.9796998016676639, -312.6436805779548536 ) ) ;
#42643 = CARTESIAN_POINT ( 'NONE',  ( -37.60766213542171954, -298.0489080631367074, -193.3615773072374679 ) ) ;
#42644 = CARTESIAN_POINT ( 'NONE',  ( 10.52439761362969683, -276.2454253879897124, -330.7436833701567025 ) ) ;
#42645 = CARTESIAN_POINT ( 'NONE',  ( 27.47663568408251322, -294.9796954283365835, -233.6513186969969809 ) ) ;
#42646 = DIRECTION ( 'NONE',  ( 0.000000000000000000, 1.000000000000000000, 0.000000000000000000 ) ) ;
#42647 = FACE_OUTER_BOUND ( 'NONE', #32199, .T. ) ;
#42648 = CARTESIAN_POINT ( 'NONE',  ( -100.6100759521699501, -294.1336626216511831, -312.1383907948717820 ) ) ;
#42649 = CARTESIAN_POINT ( 'NONE',  ( -59.48833213081312721, -273.2652893790467488, -200.6840547687569654 ) ) ;
#42650 = CARTESIAN_POINT ( 'NONE',  ( 37.64031465244426045, -294.8936142852089688, -256.2046631454692829 ) ) ;
#42651 = CARTESIAN_POINT ( 'NONE',  ( 27.77651910220412290, -295.2886875565050673, -310.8046546133618904 ) ) ;
#42652 = CARTESIAN_POINT ( 'NONE',  ( -69.52389536483657650, -291.4768901203700011, -337.9209784098173941 ) ) ;
#42653 =( REPRESENTATION_RELATIONSHIP ('NONE','NONE', #78428, #80896 ) REPRESENTATION_RELATIONSHIP_WITH_TRANSFORMATION ( #49212 )SHAPE_REPRESENTATION_RELATIONSHIP( ) );
#42654 = CARTESIAN_POINT ( 'NONE',  ( -65.03470287340681466, -275.4144774329361667, -339.9368454969134064 ) ) ;
#42655 = CARTESIAN_POINT ( 'NONE',  ( 18.53195299637424753, -278.1612296395080648, -319.5682515581325447 ) ) ;
#42656 = CARTESIAN_POINT ( 'NONE',  ( -53.48502648492690525, -293.3405400750720560, -343.0826061733354777 ) ) ;
#42657 = CARTESIAN_POINT ( 'NONE',  ( 38.17857347994645068, -283.3352610884610385, -264.2788689955200994 ) ) ;
#42658 = CARTESIAN_POINT ( 'NONE',  ( -62.65676387679056347, -284.6352500180802281, -201.5074682865840430 ) ) ;
#42659 = CARTESIAN_POINT ( 'NONE',  ( -105.3677979232747077, -263.0180028947901860, -317.1570552232428213 ) ) ;
#42660 = ORIENTED_EDGE ( 'NONE', *, *, #31148, .F. ) ;
#42661 = CARTESIAN_POINT ( 'NONE',  ( -108.9488684060140997, -284.4074610409488173, -256.0607355377569547 ) ) ;
#42662 = CARTESIAN_POINT ( 'NONE',  ( -14.33365010659369077, -281.4232006105839332, -197.1472461593778860 ) ) ;
#42663 = CARTESIAN_POINT ( 'NONE',  ( -69.61151350320699294, -284.4317125872794918, -200.8726032522603475 ) ) ;
#42664 = CARTESIAN_POINT ( 'NONE',  ( -112.7672430482424488, -279.6733725233076484, -256.0146379608212328 ) ) ;
#42665 = EDGE_CURVE ( 'NONE', #62986, #46709, #55444, .T. ) ;
#42666 = CARTESIAN_POINT ( 'NONE',  ( -110.7680358687956641, -279.8096234922635404, -291.1284233754840898 ) ) ;
#42667 = CARTESIAN_POINT ( 'NONE',  ( 17.36665895637873192, -273.6952119285918457, -314.0302885647153062 ) ) ;
#42668 = CARTESIAN_POINT ( 'NONE',  ( 85.80530294649854284, 82.61953402769070465, -302.2778766101830001 ) ) ;
#42669 = EDGE_LOOP ( 'NONE', ( #48391, #30450 ) ) ;
#42670 = CARTESIAN_POINT ( 'NONE',  ( -39.24390427567689699, -300.0284663726370127, -195.3724915477045556 ) ) ;
#42671 = CARTESIAN_POINT ( 'NONE',  ( -11.14275193769495864, -278.4152501914209097, -200.4103682797326371 ) ) ;
#42672 = CARTESIAN_POINT ( 'NONE',  ( -113.1779438795799138, -292.3728570457565183, -265.5821907631614067 ) ) ;
#42673 = CARTESIAN_POINT ( 'NONE',  ( -5.504603325692409399, -293.9705048623722519, -336.1799006659069846 ) ) ;
#42674 = CARTESIAN_POINT ( 'NONE',  ( -114.0516562745819158, -289.9774362787086375, -276.9420829750088160 ) ) ;
#42675 = CARTESIAN_POINT ( 'NONE',  ( -147.8070425842518034, -211.3363389866113664, 21.50000000000000000 ) ) ;
#42677 = CARTESIAN_POINT ( 'NONE',  ( -22.27683532998981519, -284.6480234467157970, -198.0626258528485266 ) ) ;
#42676 = CARTESIAN_POINT ( 'NONE',  ( 32.86793026969274223, -292.5154332909403365, -300.6478447484029175 ) ) ;
#42678 = CARTESIAN_POINT ( 'NONE',  ( -37.57725767459377408, -293.9096242184923540, -196.1136340414212782 ) ) ;
#42679 = CARTESIAN_POINT ( 'NONE',  ( -56.43096508852794813, -284.6185460907389029, -341.3318403965304242 ) ) ;
#42680 = ORIENTED_EDGE ( 'NONE', *, *, #42395, .F. ) ;
#42681 = CARTESIAN_POINT ( 'NONE',  ( -112.9423837617850381, -291.6604651000007493, -257.0435788917860123 ) ) ;
#42682 = CARTESIAN_POINT ( 'NONE',  ( -22.18775952995407863, -280.7437398214368613, -198.8365200227580942 ) ) ;
#42683 = CARTESIAN_POINT ( 'NONE',  ( 38.21208988301704323, -292.5069109098688500, -283.0751192075867948 ) ) ;
#42684 = CARTESIAN_POINT ( 'NONE',  ( -14.98943083880696037, -289.5727613191414207, -343.9322963618342897 ) ) ;
#42685 = CARTESIAN_POINT ( 'NONE',  ( -98.97607301728342577, -290.4310792291598773, -316.4342972827571430 ) ) ;
#42686 = CARTESIAN_POINT ( 'NONE',  ( 15.97301630148994001, -287.0012732660467236, -220.4774434567572712 ) ) ;
#42687 = EDGE_LOOP ( 'NONE', ( #11062, #3161, #35461, #81507 ) ) ;
#42688 = CARTESIAN_POINT ( 'NONE',  ( 195.7761921920649684, 26.31373072850298556, 13.59762452525894005 ) ) ;
#42689 = CARTESIAN_POINT ( 'NONE',  ( 35.19415262035013825, -295.6937470927641129, -292.4217990055070686 ) ) ;
#42690 = CARTESIAN_POINT ( 'NONE',  ( -104.8107636197279646, -295.7074362789515476, -234.1763010823696618 ) ) ;
#42691 = ADVANCED_FACE ( 'NONE', ( #86053 ), #25150, .T. ) ;
#42692 = CARTESIAN_POINT ( 'NONE',  ( -105.7297198731176451, -277.9613814299054866, -244.0182391773769837 ) ) ;
#42693 = CARTESIAN_POINT ( 'NONE',  ( -35.51895491348318501, -273.5820732781861579, -193.4311308773412463 ) ) ;
#42694 = CARTESIAN_POINT ( 'NONE',  ( -47.91143771770327220, -293.6687457674160555, -343.3442817792142137 ) ) ;
#42695 = CARTESIAN_POINT ( 'NONE',  ( 10.33365654855795945, -278.1437280896068955, -326.9741410137662569 ) ) ;
#42696 = CARTESIAN_POINT ( 'NONE',  ( -94.71821571352488434, -271.3481332440125016, -223.2370987455944373 ) ) ;
#42697 = AXIS2_PLACEMENT_3D ( 'NONE', #91112, #40452, #5925 ) ;
#42698 = CARTESIAN_POINT ( 'NONE',  ( 36.03958236762688472, -294.7982955396258262, -273.4906789686825732 ) ) ;
#42699 = CARTESIAN_POINT ( 'NONE',  ( -31.56433566922716594, -296.0573199253470875, -343.4925497855322760 ) ) ;
#42700 = CARTESIAN_POINT ( 'NONE',  ( 222.8344101925596306, 0.000000000000000000, 7.000000000000000000 ) ) ;
#42701 = AXIS2_PLACEMENT_3D ( 'NONE', #74183, #11184, #9301 ) ;
#42702 = CARTESIAN_POINT ( 'NONE',  ( -96.76848585895108101, -295.1817193915935036, -224.3133459985474758 ) ) ;
#42703 = CARTESIAN_POINT ( 'NONE',  ( -23.39113940076908094, -298.8739271444148358, -193.4615530850009577 ) ) ;
#42704 = CARTESIAN_POINT ( 'NONE',  ( -53.55587437105933191, -287.8389979442837898, -342.1418637924992368 ) ) ;
#42705 = CARTESIAN_POINT ( 'NONE',  ( -107.2905268654574229, -274.9058821284872351, -243.1592330861918470 ) ) ;
#42706 = CARTESIAN_POINT ( 'NONE',  ( -110.0457636035864653, -273.3621037239402654, -245.1887907697699518 ) ) ;
#42708 = CARTESIAN_POINT ( 'NONE',  ( -104.9798918036931781, -296.5169415369581998, -297.8777041362385489 ) ) ;
#42707 = CIRCLE ( 'NONE', #75959, 154.4364916446740210 ) ;
#42709 = AXIS2_PLACEMENT_3D ( 'NONE', #71060, #50194, #14708 ) ;
#42710 = CARTESIAN_POINT ( 'NONE',  ( -111.6195576906492448, -280.6942984741440341, -257.6643987142851984 ) ) ;
#42711 = CARTESIAN_POINT ( 'NONE',  ( -25.45558560918054880, -278.8854412896631629, -194.7832207286726316 ) ) ;
#42712 = CARTESIAN_POINT ( 'NONE',  ( -38.73902342481922290, -282.4178376508589281, -347.2464889879695420 ) ) ;
#42713 = CARTESIAN_POINT ( 'NONE',  ( 27.55833933201302699, -275.4431730433088887, -311.7068714345336389 ) ) ;
#42714 = CARTESIAN_POINT ( 'NONE',  ( 14.63074538973157424, -279.1687439922761769, -214.5637026863836638 ) ) ;
#42715 = CARTESIAN_POINT ( 'NONE',  ( -38.12463413549750868, -278.0422048580156797, -195.1985245915314522 ) ) ;
#42716 = CARTESIAN_POINT ( 'NONE',  ( -11.26457354804663069, -272.9733113944863021, -201.4926895191075289 ) ) ;
#42717 = CARTESIAN_POINT ( 'NONE',  ( 25.37001462644079197, -278.1084698181304589, -311.5902184319775756 ) ) ;
#42718 = CARTESIAN_POINT ( 'NONE',  ( 153.4734828627512400, 20.31592703335031658, 12.31730288665599637 ) ) ;
#42719 = CARTESIAN_POINT ( 'NONE',  ( -58.45319697019549920, -289.8006491648515066, -198.0236346052819840 ) ) ;
#42720 = CARTESIAN_POINT ( 'NONE',  ( -98.34826317967218756, -291.1792842460076258, -223.3589437731529870 ) ) ;
#42721 = CARTESIAN_POINT ( 'NONE',  ( -9.857859013599144404, -278.6941960407934289, -340.3230140734858082 ) ) ;
#42722 = CARTESIAN_POINT ( 'NONE',  ( -57.37190185508347895, -271.7936214766053240, -198.0311596538433321 ) ) ;
#42723 = DIRECTION ( 'NONE',  ( -0.000000000000000000, 0.000000000000000000, -1.000000000000000000 ) ) ;
#42724 = CARTESIAN_POINT ( 'NONE',  ( 208.8547504194143585, 36.42232975996840594, 14.79569954156338518 ) ) ;
#42725 = CARTESIAN_POINT ( 'NONE',  ( -95.39336738838214558, -283.2066959169408165, -222.8543224466426693 ) ) ;
#42726 =( BOUNDED_SURFACE ( )  B_SPLINE_SURFACE ( 3, 2, ( 
 ( #35129, #72523, #64051 ),
 ( #7643, #72078, #20930 ),
 ( #49799, #14316, #64530 ),
 ( #44080, #65443, #7194 ),
 ( #78696, #558, #29442 ),
 ( #36069, #87174, #51194 ),
 ( #15224, #13837, #57398 ),
 ( #72982, #8112, #42688 ),
 ( #36999, #6742, #1024 ),
 ( #29902, #58786, #49343 ),
 ( #92894, #28053, #71607 ),
 ( #35615, #93355, #38376 ),
 ( #30832, #73907, #67745 ),
 ( #74366, #75308, #24645 ) ),
 .UNSPECIFIED., .F., .F., .F. ) 
 B_SPLINE_SURFACE_WITH_KNOTS ( ( 4, 2, 2, 2, 2, 2, 4 ),
 ( 3, 3 ),
 ( -2.168404344971008868E-19, 0.001236320232021350003, 0.001854480348032025222, 0.002472640464042700440, 0.003090800580053375442, 0.003708960696064050877, 0.004945280928085400880 ),
 ( 0.000000000000000000, 1.000000000000000000 ),
 .UNSPECIFIED. ) 
 GEOMETRIC_REPRESENTATION_ITEM ( )  RATIONAL_B_SPLINE_SURFACE ( (
 ( 1.000000000000000000, 0.8108476219622871017, 1.000000000000000000),
 ( 1.000000000000000000, 0.8255659973200745183, 1.000000000000000000),
 ( 1.000000000000000000, 0.8395011523818814991, 1.000000000000000000),
 ( 1.000000000000000000, 0.8588211550372549796, 1.000000000000000000),
 ( 1.000000000000000000, 0.8649348442247967172, 1.000000000000000000),
 ( 1.000000000000000000, 0.8760455507362673311, 1.000000000000000000),
 ( 1.000000000000000000, 0.8810998449848480574, 1.000000000000000000),
 ( 1.000000000000000000, 0.8900036393291742565, 1.000000000000000000),
 ( 1.000000000000000000, 0.8938622710282666528, 1.000000000000000000),
 ( 1.000000000000000000, 0.8997338558213243687, 1.000000000000000000),
 ( 1.000000000000000000, 0.9018082123500091862, 1.000000000000000000),
 ( 1.000000000000000000, 0.9050182246960185584, 1.000000000000000000),
 ( 1.000000000000000000, 0.9029724514278080205, 1.000000000000000000),
 ( 1.000000000000000000, 0.8966167345234238306, 1.000000000000000000) ) ) 
 REPRESENTATION_ITEM ( '' )  SURFACE ( )  );
#42727 = CARTESIAN_POINT ( 'NONE',  ( 180.7287904564219332, 250.5000000000000568, -24.90000000000003411 ) ) ;
#42728 = CARTESIAN_POINT ( 'NONE',  ( 26.12838274646293257, -292.8500508480920530, -307.2213822781752697 ) ) ;
#42729 = CARTESIAN_POINT ( 'NONE',  ( 35.73348645255310174, -285.8613086429143095, -283.4333246870743892 ) ) ;
#42730 = DIRECTION ( 'NONE',  ( -0.09665007798479426093, -1.048651511008089408E-15, -0.9953184226294282677 ) ) ;
#42731 = CARTESIAN_POINT ( 'NONE',  ( 157.4851178187871312, 15.19241473665941378, -8.999999999999666045 ) ) ;
#42732 = CARTESIAN_POINT ( 'NONE',  ( -23.16509362626534241, -292.8708136334317942, -344.0621099610601163 ) ) ;
#42733 = CARTESIAN_POINT ( 'NONE',  ( -111.0464106232770831, -283.2839208396907225, -250.4061133829896164 ) ) ;
#42734 = CARTESIAN_POINT ( 'NONE',  ( -67.65329937286229267, -281.2478050768619937, -203.0595653792132396 ) ) ;
#42735 = CARTESIAN_POINT ( 'NONE',  ( -113.7569738163876849, -285.8334838231838262, -264.2950429750109151 ) ) ;
#42736 = CARTESIAN_POINT ( 'NONE',  ( -14.51058288484636094, -278.5838453107477903, -197.8303376636982307 ) ) ;
#42737 = CARTESIAN_POINT ( 'NONE',  ( 28.80995496453565607, -287.1353106951205518, -239.4910916057096699 ) ) ;
#42738 =( BOUNDED_CURVE ( )  B_SPLINE_CURVE ( 3, ( #80811, #88828, #89286, #51921 ),
 .UNSPECIFIED., .F., .F. ) 
 B_SPLINE_CURVE_WITH_KNOTS ( ( 4, 4 ),
 ( 3.141592653589793116, 4.712388980384689674 ),
 .UNSPECIFIED. ) 
 CURVE ( )  GEOMETRIC_REPRESENTATION_ITEM ( )  RATIONAL_B_SPLINE_CURVE ( ( 1.000000000000000000, 0.8047378541243649375, 0.8047378541243649375, 1.000000000000000000 ) ) 
 REPRESENTATION_ITEM ( '' )  );
#42739 = CARTESIAN_POINT ( 'NONE',  ( -59.35410140863530870, -278.7680755165813480, -340.5809805992865336 ) ) ;
#42740 = CARTESIAN_POINT ( 'NONE',  ( -109.0475500006786689, -279.5469551311566647, -255.7767043200873616 ) ) ;
#42741 = CARTESIAN_POINT ( 'NONE',  ( -40.76748788169187776, -287.9892841666302843, -195.0327482804862598 ) ) ;
#42742 = EDGE_LOOP ( 'NONE', ( #22898, #66355, #38503, #50016 ) ) ;
#42743 = CARTESIAN_POINT ( 'NONE',  ( -107.7721715813901255, -296.7840241410740418, -239.1077837069504426 ) ) ;
#42744 = CARTESIAN_POINT ( 'NONE',  ( -64.39399362766693002, -291.3867065957127807, -339.9867694047253508 ) ) ;
#42745 = CARTESIAN_POINT ( 'NONE',  ( 196.8803347170859865, 24.42324672360810212, 12.49999999999999289 ) ) ;
#42746 = CARTESIAN_POINT ( 'NONE',  ( -2.659677404128715672, -282.9805209788415823, -198.2697987213421698 ) ) ;
#42747 = ORIENTED_EDGE ( 'NONE', *, *, #47247, .T. ) ;
#42748 = CARTESIAN_POINT ( 'NONE',  ( -60.28666473558980954, -271.7553288441165478, -198.7277929964787120 ) ) ;
#42749 = CARTESIAN_POINT ( 'NONE',  ( 38.02228521017593721, -292.0942840304360288, -281.6176773778514644 ) ) ;
#42750 = CARTESIAN_POINT ( 'NONE',  ( -84.52261865440348743, -295.2298744072514296, -326.2123975259087842 ) ) ;
#42751 = CARTESIAN_POINT ( 'NONE',  ( 35.44706747601616570, -289.2237518526308691, -281.9526647420209429 ) ) ;
#42752 = CARTESIAN_POINT ( 'NONE',  ( 28.67524911578215097, -282.8628173275653808, -236.7850818899946148 ) ) ;
#42753 = CARTESIAN_POINT ( 'NONE',  ( -8.439059609532264972, -290.1064168208470164, -341.1088872307944939 ) ) ;
#42754 = CARTESIAN_POINT ( 'NONE',  ( -91.23915194801482187, -291.1138662782858546, -324.7344563100068626 ) ) ;
#42755 = CARTESIAN_POINT ( 'NONE',  ( -45.84150799167230872, -285.1599463806196582, -344.9303107361408820 ) ) ;
#42756 = CARTESIAN_POINT ( 'NONE',  ( -111.8269004374234186, -278.4739295689862502, -289.9309878473421804 ) ) ;
#42757 = CARTESIAN_POINT ( 'NONE',  ( 18.44959431718224963, -292.3387481116369031, -321.3945915641779720 ) ) ;
#42758 = CARTESIAN_POINT ( 'NONE',  ( 30.72280569084552937, -280.9192817435474581, -234.2443416742731301 ) ) ;
#42759 = CARTESIAN_POINT ( 'NONE',  ( -35.38105394294588990, -275.9374035450653082, -196.1390931051824396 ) ) ;
#42760 = CARTESIAN_POINT ( 'NONE',  ( 35.78497577281001440, -296.2662352645559167, -287.0191576251351080 ) ) ;
#42761 = CARTESIAN_POINT ( 'NONE',  ( 29.63910407537412794, -274.2632538661408717, -306.3545479852188009 ) ) ;
#42763 = AXIS2_PLACEMENT_3D ( 'NONE', #64202, #78373, #13978 ) ;
#42762 = PLANE ( 'NONE',  #10725 ) ;
#42764 = CARTESIAN_POINT ( 'NONE',  ( -1.930766155255069894, -280.0423880801637324, -206.4545127141937257 ) ) ;
#42765 = CIRCLE ( 'NONE', #39694, 5.603083949679982467 ) ;
#42766 = CARTESIAN_POINT ( 'NONE',  ( 19.59241879461066560, -277.4566347288656516, -321.6302877564377241 ) ) ;
#42767 = CARTESIAN_POINT ( 'NONE',  ( -73.14934157785657476, -298.9927627113842163, -206.0712452837533419 ) ) ;
#42768 = CARTESIAN_POINT ( 'NONE',  ( -110.0058332601304301, -283.2980626186882205, -295.1147837489177732 ) ) ;
#42769 = CARTESIAN_POINT ( 'NONE',  ( -85.32517614939537509, -291.4855762858202297, -326.7808552704847216 ) ) ;
#42770 = CARTESIAN_POINT ( 'NONE',  ( -2.937169867794221290, -276.0992200337769304, -202.3556237322580955 ) ) ;
#42771 = AXIS2_PLACEMENT_3D ( 'NONE', #11410, #47370, #89998 ) ;
#42772 = CARTESIAN_POINT ( 'NONE',  ( -111.9660026560661663, -274.0796304152542007, -253.4936419587741625 ) ) ;
#42774 = DIRECTION ( 'NONE',  ( -1.000000000000000000, -0.000000000000000000, -0.000000000000000000 ) ) ;
#42773 = TOROIDAL_SURFACE ( 'NONE', #54800, 24.50000000000000355, 0.5000000000000000000 ) ;
#42775 = CARTESIAN_POINT ( 'NONE',  ( 37.47595382155799371, -295.5932523172907622, -273.5421194629119555 ) ) ;
#42776 = CARTESIAN_POINT ( 'NONE',  ( -29.27164136142819473, -280.9496414992527775, -344.8098152834119787 ) ) ;
#42777 = AXIS2_PLACEMENT_3D ( 'NONE', #35889, #74072, #88273 ) ;
#42778 = CARTESIAN_POINT ( 'NONE',  ( -111.2106790195318951, -290.4906165075586841, -248.7019802093065834 ) ) ;
#42779 = CARTESIAN_POINT ( 'NONE',  ( 19.54593736581788832, -274.2443485069447888, -318.6896137785293490 ) ) ;
#42780 = CARTESIAN_POINT ( 'NONE',  ( 31.97572659130898387, -288.7420122456922513, -238.5871368303445479 ) ) ;
#42781 = CARTESIAN_POINT ( 'NONE',  ( -65.43274500006812389, -290.5964070528142429, -202.6340391450372067 ) ) ;
#42782 = VERTEX_POINT ( 'NONE', #3844 ) ;
#42783 = CARTESIAN_POINT ( 'NONE',  ( -107.2000967268968736, -288.7273052291942577, -301.4495338470833303 ) ) ;
#42784 = CARTESIAN_POINT ( 'NONE',  ( -74.98687117398149837, -291.2028263959568335, -207.7326972734991557 ) ) ;
#42785 = VERTEX_POINT ( 'NONE', #39792 ) ;
#42786 = CARTESIAN_POINT ( 'NONE',  ( 27.19215870989951611, -289.1786753810128516, -311.8942350472209455 ) ) ;
#42787 = AXIS2_PLACEMENT_3D ( 'NONE', #4152, #53872, #33022 ) ;
#42788 = CARTESIAN_POINT ( 'NONE',  ( 20.04171244583395506, -276.5224557371282117, -315.5391065248404061 ) ) ;
#42789 = CARTESIAN_POINT ( 'NONE',  ( -16.60373590580135073, -293.7107795455372639, -344.2499212861386582 ) ) ;
#42790 = CARTESIAN_POINT ( 'NONE',  ( -92.35501396645300076, -284.4655315012472556, -324.0905148431945122 ) ) ;
#42791 = EDGE_CURVE ( 'NONE', #70176, #74347, #54024, .T. ) ;
#42792 = CARTESIAN_POINT ( 'NONE',  ( -57.75441463760440541, -286.1289585621425431, -196.0827022284918542 ) ) ;
#42793 = CARTESIAN_POINT ( 'NONE',  ( 35.16130328111002257, -282.0053857146162954, -279.4566598182844359 ) ) ;
#42794 = CARTESIAN_POINT ( 'NONE',  ( -90.23014037448028546, -230.4905643893864351, -347.8797927120800750 ) ) ;
#42795 = CARTESIAN_POINT ( 'NONE',  ( 201.9871895515903475, 295.7236489450776276, -54.00000000003252865 ) ) ;
#42796 = CARTESIAN_POINT ( 'NONE',  ( -31.50900740967911418, -124.4314099722194271, -360.5826283136302095 ) ) ;
#42797 = CARTESIAN_POINT ( 'NONE',  ( -103.3463686406470856, -272.1751947359218775, -238.8018806508005412 ) ) ;
#42798 = CARTESIAN_POINT ( 'NONE',  ( -51.60821119650277211, -272.7858226493395932, -198.4015820285553104 ) ) ;
#42799 = CARTESIAN_POINT ( 'NONE',  ( -30.60259167333858699, -294.4767486070976474, -347.0038692408732572 ) ) ;
#42800 = CARTESIAN_POINT ( 'NONE',  ( 203.1405228849236551, 291.9636489450776367, -53.99999999998649258 ) ) ;
#42801 = CARTESIAN_POINT ( 'NONE',  ( -38.33410824516327153, -272.7247879510630924, -193.8607035990392546 ) ) ;
#42802 = CARTESIAN_POINT ( 'NONE',  ( -111.4467039188222230, -298.4695842586521621, -265.9663607470388342 ) ) ;
#42803 = CARTESIAN_POINT ( 'NONE',  ( 22.37209593357130544, -289.4621960586882778, -313.2039241313341904 ) ) ;
#42804 = CARTESIAN_POINT ( 'NONE',  ( -79.72055723569047814, -292.5441693620398951, -210.4803418033979483 ) ) ;
#42805 = ORIENTED_EDGE ( 'NONE', *, *, #78996, .T. ) ;
#42806 = CARTESIAN_POINT ( 'NONE',  ( -99.81002242625292808, -296.8995688722610566, -315.0659762124039958 ) ) ;
#42807 = CARTESIAN_POINT ( 'NONE',  ( 4.755710716422604456, -287.1299350248181668, -210.5849213593931779 ) ) ;
#42808 = CIRCLE ( 'NONE', #38186, 2.000000000000000000 ) ;
#42809 = CARTESIAN_POINT ( 'NONE',  ( 36.94308322083536211, -294.6014360958367888, -290.0062136488913893 ) ) ;
#42810 = CARTESIAN_POINT ( 'NONE',  ( -16.51750363910209529, -295.2825451050949823, -344.4830330095495015 ) ) ;
#42811 = CARTESIAN_POINT ( 'NONE',  ( -6.043555356203813567, -292.6420092850357264, -204.3971571384788604 ) ) ;
#42812 = VERTEX_POINT ( 'NONE', #69640 ) ;
#42813 = CARTESIAN_POINT ( 'NONE',  ( -4.474996219834001643, -276.4019684744186520, -202.3094381367092183 ) ) ;
#42814 = ADVANCED_FACE ( 'NONE', ( #11872 ), #57212, .T. ) ;
#42815 = ORIENTED_EDGE ( 'NONE', *, *, #68345, .T. ) ;
#42816 = CARTESIAN_POINT ( 'NONE',  ( -113.2394910484469364, -277.9019554826218155, -282.9727093455488216 ) ) ;
#42817 = CARTESIAN_POINT ( 'NONE',  ( -13.79106924338273465, -272.7628204906073961, -200.4196553217296355 ) ) ;
#42818 = CARTESIAN_POINT ( 'NONE',  ( -40.80324115540862095, -275.0874032860800185, -197.0838641461715497 ) ) ;
#42819 = CARTESIAN_POINT ( 'NONE',  ( 34.39746206246279314, -276.6870635009381090, -285.0886791179989928 ) ) ;
#42820 = CARTESIAN_POINT ( 'NONE',  ( -52.36746971907324166, -275.6225641846683629, -195.8211480651992815 ) ) ;
#42821 = CARTESIAN_POINT ( 'NONE',  ( 7.247075166880568631, -274.4684378754014915, -331.1731178007657945 ) ) ;
#42822 = CARTESIAN_POINT ( 'NONE',  ( -110.4859856808060954, -297.1889233751873007, -271.4729337633568775 ) ) ;
#42823 = CARTESIAN_POINT ( 'NONE',  ( 6.398713628329613989, -293.0198636074453589, -329.6035868868543730 ) ) ;
#42824 = DIRECTION ( 'NONE',  ( 0.000000000000000000, 0.000000000000000000, 1.000000000000000000 ) ) ;
#42825 = CARTESIAN_POINT ( 'NONE',  ( -91.01973036336205780, -279.8070895799918958, -215.1670064438016254 ) ) ;
#42826 = CARTESIAN_POINT ( 'NONE',  ( 28.03144986521090942, -276.1606934816746843, -302.9612503922536462 ) ) ;
#42827 = CARTESIAN_POINT ( 'NONE',  ( 36.22172509251311112, -285.9696824808132192, -249.1557035944968277 ) ) ;
#42828 = CARTESIAN_POINT ( 'NONE',  ( -74.88680563515852384, -299.5540184192034872, -205.1830680766852595 ) ) ;
#42829 = DIRECTION ( 'NONE',  ( -1.000000000000000000, 0.000000000000000000, 0.000000000000000000 ) ) ;
#42830 = AXIS2_PLACEMENT_3D ( 'NONE', #13627, #13169, #42478 ) ;
#42831 = CARTESIAN_POINT ( 'NONE',  ( 34.67885154054003038, -286.9187211272819127, -283.2313108570337477 ) ) ;
#42832 = CARTESIAN_POINT ( 'NONE',  ( -81.88003629483939960, -277.6761414321497341, -211.1840832710489053 ) ) ;
#42833 = CARTESIAN_POINT ( 'NONE',  ( -68.75850763232951124, -278.2055545331609778, -203.8152005624672540 ) ) ;
#42834 = CARTESIAN_POINT ( 'NONE',  ( 0.3791655890542534602, -284.5502087238114086, -335.2434396784627211 ) ) ;
#42835 = CARTESIAN_POINT ( 'NONE',  ( -81.04357185737369207, -278.8659958423166927, -329.3295579403575175 ) ) ;
#42836 = FACE_OUTER_BOUND ( 'NONE', #76659, .T. ) ;
#42837 = AXIS2_PLACEMENT_3D ( 'NONE', #80681, #73595, #38526 ) ;
#42838 = CARTESIAN_POINT ( 'NONE',  ( 32.98318290264681707, -273.5734388621735320, -240.8844823936609600 ) ) ;
#42839 = CONICAL_SURFACE ( 'NONE', #26206, 5.025000000000002132, 0.7853981633971707232 ) ;
#42840 = CARTESIAN_POINT ( 'NONE',  ( 27.94861120575786373, -275.7579375589231745, -237.4815207562887736 ) ) ;
#42841 = CARTESIAN_POINT ( 'NONE',  ( -1.233210700214557143, -284.5744958168110657, -336.3014604844067321 ) ) ;
#42842 = DIRECTION ( 'NONE',  ( 1.000000000000000000, 0.000000000000000000, 0.000000000000000000 ) ) ;
#42843 = CARTESIAN_POINT ( 'NONE',  ( -23.55030914826560107, -290.7974984251874844, -344.7049474779601610 ) ) ;
#42844 = AXIS2_PLACEMENT_3D ( 'NONE', #53556, #16631, #89983 ) ;
#42845 = CARTESIAN_POINT ( 'NONE',  ( 32.09350561450776240, -291.1807039559618033, -241.8749988525930519 ) ) ;
#42846 = CARTESIAN_POINT ( 'NONE',  ( 82.15178654341977449, -299.3244375900736713, -197.3535362759786835 ) ) ;
#42847 = CARTESIAN_POINT ( 'NONE',  ( 30.63731071160582076, -273.8635672787256112, -242.2971858316740281 ) ) ;
#42848 = CARTESIAN_POINT ( 'NONE',  ( 36.65378542668494788, -291.7690571875479009, -276.3221242687504287 ) ) ;
#42849 = CARTESIAN_POINT ( 'NONE',  ( -32.04911714649202992, -124.5213432794980974, -365.6788127701597659 ) ) ;
#42850 = DIRECTION ( 'NONE',  ( 1.000000000000000000, 0.000000000000000000, 0.000000000000000000 ) ) ;
#42851 = CARTESIAN_POINT ( 'NONE',  ( -82.45843028957040133, -288.1358173262731270, -331.9012545646234571 ) ) ;
#42852 = CARTESIAN_POINT ( 'NONE',  ( -110.2859365582050231, -286.0017888001420374, -281.8945940015221368 ) ) ;
#42853 = CARTESIAN_POINT ( 'NONE',  ( 23.90004626481771766, -285.1865775561024066, -225.3786490164402210 ) ) ;
#42854 = CIRCLE ( 'NONE', #56541, 1.000000000000000888 ) ;
#42855 = CARTESIAN_POINT ( 'NONE',  ( -71.66777297915450617, -284.9403834014049721, -335.4540948770547288 ) ) ;
#42856 = CARTESIAN_POINT ( 'NONE',  ( -56.35102821920244764, -284.1062871213039784, -341.0098771506539492 ) ) ;
#42857 = CARTESIAN_POINT ( 'NONE',  ( -109.6608862924576044, -292.8034163520489983, -249.1870272947481340 ) ) ;
#42858 = CARTESIAN_POINT ( 'NONE',  ( -60.86869637794331567, -274.0883946869938086, -197.0100400529091473 ) ) ;
#42859 = AXIS2_PLACEMENT_3D ( 'NONE', #81732, #10228, #89289 ) ;
#42860 = CARTESIAN_POINT ( 'NONE',  ( -96.18437910901727150, -287.9842961317706340, -317.7825145594953824 ) ) ;
#42861 = CARTESIAN_POINT ( 'NONE',  ( 10.52605788214132154, -276.4120786065170705, -330.7423672093166829 ) ) ;
#42862 = CARTESIAN_POINT ( 'NONE',  ( 24.30532809127641869, -296.1058158920566257, -312.5406284699500929 ) ) ;
#42863 = CARTESIAN_POINT ( 'NONE',  ( -48.18343439339132317, -256.9970711660894267, -450.6082928460614312 ) ) ;
#42864 = FACE_OUTER_BOUND ( 'NONE', #80784, .T. ) ;
#42865 = CARTESIAN_POINT ( 'NONE',  ( -108.2413029426609654, -282.9824654957402572, -289.7604109493443048 ) ) ;
#42866 = CARTESIAN_POINT ( 'NONE',  ( -100.2006986490436731, -277.1047367086743520, -229.3557369658782363 ) ) ;
#42867 = CARTESIAN_POINT ( 'NONE',  ( -73.59820918239149989, -272.0602176772786720, -203.1594538849116134 ) ) ;
#42868 = CARTESIAN_POINT ( 'NONE',  ( 3.183731583561480782, -275.8402037402388487, -331.2017462877410026 ) ) ;
#42869 = CARTESIAN_POINT ( 'NONE',  ( -34.85307546490108876, -293.6041043838564519, -196.7098145236149094 ) ) ;
#42870 = CIRCLE ( 'NONE', #62492, 7.500000000000012434 ) ;
#42871 = CARTESIAN_POINT ( 'NONE',  ( 23.13404728551412859, -295.0673433039234510, -311.7546906606428365 ) ) ;
#42872 = CARTESIAN_POINT ( 'NONE',  ( -93.31716609715077482, -297.1515798906043528, -322.5344633410979327 ) ) ;
#42873 = CARTESIAN_POINT ( 'NONE',  ( -88.50336334515367298, -295.6271232538553022, -322.5040731885257514 ) ) ;
#42874 = CARTESIAN_POINT ( 'NONE',  ( -2.412844464871696015, -290.5905754310778661, -336.7886395665131545 ) ) ;
#42875 = CARTESIAN_POINT ( 'NONE',  ( -111.1073664436834036, -284.4412001287362841, -292.4891653028661835 ) ) ;
#42876 = CARTESIAN_POINT ( 'NONE',  ( 17.21685270776070453, -272.9595542096821532, -217.7151634921682160 ) ) ;
#42877 = CARTESIAN_POINT ( 'NONE',  ( 36.69181147680444610, -287.1179910019855015, -249.0048385730078451 ) ) ;
#42878 = CARTESIAN_POINT ( 'NONE',  ( -43.31410954173887973, -279.1078519910307136, -344.7666092365767554 ) ) ;
#42879 = EDGE_CURVE ( 'NONE', #42461, #24392, #47432, .T. ) ;
#42880 = CARTESIAN_POINT ( 'NONE',  ( -81.61131448491130413, -284.4912235280290815, -212.0206543908765582 ) ) ;
#42881 = CARTESIAN_POINT ( 'NONE',  ( -6.473536761631635272, -286.6465964805590261, -338.7142974442743935 ) ) ;
#42882 = CARTESIAN_POINT ( 'NONE',  ( -79.37448608631180491, -205.8233151019928755, -350.8497528714748341 ) ) ;
#42883 = CARTESIAN_POINT ( 'NONE',  ( 35.69121543308865796, -287.1047188554355216, -273.7689465134058651 ) ) ;
#42884 = CARTESIAN_POINT ( 'NONE',  ( -30.22473844818456357, -283.9054366481393572, -346.7952011474077381 ) ) ;
#42885 = CARTESIAN_POINT ( 'NONE',  ( -110.5610600959339109, -289.3182681583547264, -293.5944727907153720 ) ) ;
#42886 = CARTESIAN_POINT ( 'NONE',  ( -88.41054561962432956, -280.9504540514101336, -213.8066006221476414 ) ) ;
#42887 = CARTESIAN_POINT ( 'NONE',  ( -111.9994805814217358, -279.6568818455803012, -287.0797929562136233 ) ) ;
#42888 = CARTESIAN_POINT ( 'NONE',  ( -102.1549058820770313, -278.8436013845753223, -236.6617011701434308 ) ) ;
#42889 = CARTESIAN_POINT ( 'NONE',  ( 3.816305524780818192, -276.5886482863444371, -208.0268477078438707 ) ) ;
#42890 = CARTESIAN_POINT ( 'NONE',  ( -66.92443877691647458, -295.4292553076091963, -341.4658364154426522 ) ) ;
#42891 = CARTESIAN_POINT ( 'NONE',  ( -48.32741492145277107, -287.2126116271723504, -344.2452685054324775 ) ) ;
#42892 = CARTESIAN_POINT ( 'NONE',  ( -58.73382057611257778, -293.3800933243644522, -197.2255069819435107 ) ) ;
#42893 = CARTESIAN_POINT ( 'NONE',  ( -86.70823585455920579, -294.6784618484621774, -324.5567933012786170 ) ) ;
#42894 = ORIENTED_EDGE ( 'NONE', *, *, #33978, .T. ) ;
#42895 = CARTESIAN_POINT ( 'NONE',  ( -48.52128163487829227, -285.1157406284925173, -343.9568458006870060 ) ) ;
#42896 = CARTESIAN_POINT ( 'NONE',  ( -82.37618502459633874, -295.3529007634854224, -327.9058686986957127 ) ) ;
#42897 = VECTOR ( 'NONE', #70810, 1000.000000000000000 ) ;
#42898 = CARTESIAN_POINT ( 'NONE',  ( -16.72298824514130544, -293.3921252007368139, -196.4939315650624962 ) ) ;
#42899 = CARTESIAN_POINT ( 'NONE',  ( -5.521611183031291503, -281.1335980485591790, -204.5479383897285572 ) ) ;
#42900 = CARTESIAN_POINT ( 'NONE',  ( 34.50576104723774762, -274.2678593768389419, -243.3284981473337609 ) ) ;
#42901 = CARTESIAN_POINT ( 'NONE',  ( -99.78264212630969610, -290.6076096185357756, -315.2662054179045867 ) ) ;
#42902 = CARTESIAN_POINT ( 'NONE',  ( -41.52501825401223812, -281.2437586226697022, -346.0618299537993607 ) ) ;
#42903 = CARTESIAN_POINT ( 'NONE',  ( -111.2130690139982363, -291.1570712332410267, -248.7101330057250550 ) ) ;
#42904 = CARTESIAN_POINT ( 'NONE',  ( 1.326375618783227850, -288.8532051437279620, -332.3035703458917851 ) ) ;
#42905 = DIRECTION ( 'NONE',  ( -1.000000000000000000, 0.000000000000000000, -5.880589007913310608E-16 ) ) ;
#42906 = AXIS2_PLACEMENT_3D ( 'NONE', #74615, #31531, #9744 ) ;
#42907 = CARTESIAN_POINT ( 'NONE',  ( 187.6632728099119163, 270.6806713873519925, -138.5576046993855641 ) ) ;
#42908 = CARTESIAN_POINT ( 'NONE',  ( 25.76221782734146259, -24.23989497703301410, -341.4211288899717260 ) ) ;
#42909 = CARTESIAN_POINT ( 'NONE',  ( -110.4542110544635705, -276.2666405000204009, -253.6410175316879361 ) ) ;
#42910 = CARTESIAN_POINT ( 'NONE',  ( -71.00689152637446000, -278.7932045549755458, -205.3911950726002829 ) ) ;
#42911 = ORIENTED_EDGE ( 'NONE', *, *, #42165, .T. ) ;
#42912 = CARTESIAN_POINT ( 'NONE',  ( -89.68469539043113059, -278.2130118908750092, -218.9624251354857449 ) ) ;
#42913 = CARTESIAN_POINT ( 'NONE',  ( -34.09983670283958190, -273.7586009658424473, -193.4505555537735404 ) ) ;
#42914 = CARTESIAN_POINT ( 'NONE',  ( 202.9506381746226964, 290.1764997590596522, -82.60574211335169537 ) ) ;
#42915 = CARTESIAN_POINT ( 'NONE',  ( -106.8753343450615603, -277.5364059179576088, -238.5528845538613325 ) ) ;
#42917 = VECTOR ( 'NONE', #50893, 1000.000000000000000 ) ;
#42916 = CARTESIAN_POINT ( 'NONE',  ( -64.68074490423430234, -281.4310051301540057, -339.8191875927582259 ) ) ;
#42918 = CARTESIAN_POINT ( 'NONE',  ( -107.4315582720668658, -297.9324548610582610, -299.8465788017890645 ) ) ;
#42919 = CARTESIAN_POINT ( 'NONE',  ( 21.85088651770049495, -293.4455971006245250, -227.5119796135670640 ) ) ;
#42920 = ORIENTED_EDGE ( 'NONE', *, *, #37853, .F. ) ;
#42921 = CARTESIAN_POINT ( 'NONE',  ( 3.877436323619794845, -287.1694396218067595, -331.2683967500805124 ) ) ;
#42922 = CARTESIAN_POINT ( 'NONE',  ( 39.45200817147964045, -276.1419123510364102, -265.4380250903752199 ) ) ;
#42923 = CARTESIAN_POINT ( 'NONE',  ( -65.57467526137273239, -297.8390559024335289, -203.0417365263949421 ) ) ;
#42924 = ORIENTED_EDGE ( 'NONE', *, *, #87369, .T. ) ;
#42925 =( LENGTH_UNIT ( ) NAMED_UNIT ( * ) SI_UNIT ( .MILLI., .METRE. ) );
#42926 = CARTESIAN_POINT ( 'NONE',  ( 196.7510731661265595, -142.7221692137691775, -21.50000000000000000 ) ) ;
#42927 = CIRCLE ( 'NONE', #8179, 24.00000000000001066 ) ;
#42928 = CIRCLE ( 'NONE', #86779, 5.000000000000004441 ) ;
#42929 = FACE_OUTER_BOUND ( 'NONE', #10544, .T. ) ;
#42930 = AXIS2_PLACEMENT_3D ( 'NONE', #15969, #8386, #8838 ) ;
#42931 = CARTESIAN_POINT ( 'NONE',  ( 33.75199499355257871, -282.3961663640185975, -252.4240552494830752 ) ) ;
#42932 = CARTESIAN_POINT ( 'NONE',  ( -36.78281895853255179, -281.8192216275961641, -194.3636298791198556 ) ) ;
#42933 = CARTESIAN_POINT ( 'NONE',  ( -71.52930925438678855, -282.5742416847735967, -335.1269718786251701 ) ) ;
#42934 = CARTESIAN_POINT ( 'NONE',  ( -54.80597981071409208, -281.6858450058968515, -198.1563566814682815 ) ) ;
#42935 = CARTESIAN_POINT ( 'NONE',  ( 27.25350221472448453, -273.5508280096681801, -234.7840550110153117 ) ) ;
#42936 = FACE_OUTER_BOUND ( 'NONE', #45567, .T. ) ;
#42937 = DIRECTION ( 'NONE',  ( 1.000000000000000000, 0.000000000000000000, -0.000000000000000000 ) ) ;
#42938 = CARTESIAN_POINT ( 'NONE',  ( -34.28725863740594093, -277.8174912846646407, -347.1389090946245801 ) ) ;
#42939 = AXIS2_PLACEMENT_3D ( 'NONE', #63412, #86074, #65274 ) ;
#42940 = ADVANCED_FACE ( 'NONE', ( #4768 ), #27813, .T. ) ;
#42941 = CARTESIAN_POINT ( 'NONE',  ( 195.4781563537916043, 27.48493576247232184, 15.50000000000000000 ) ) ;
#42942 = CARTESIAN_POINT ( 'NONE',  ( -25.87643237476757108, -275.4835837692420455, -345.9068255176592288 ) ) ;
#42943 = ORIENTED_EDGE ( 'NONE', *, *, #18516, .F. ) ;
#42944 = DIRECTION ( 'NONE',  ( 0.000000000000000000, 0.000000000000000000, -1.000000000000000000 ) ) ;
#42945 = CARTESIAN_POINT ( 'NONE',  ( -112.6832232484200489, -286.5723303095733741, -267.2089083834201801 ) ) ;
#42946 = CARTESIAN_POINT ( 'NONE',  ( 33.60013994905521884, -292.9848324578926508, -288.2456658919263077 ) ) ;
#42947 = ADVANCED_FACE ( 'NONE', ( #18504 ), #79449, .F. ) ;
#42948 = CARTESIAN_POINT ( 'NONE',  ( -26.16757483272246532, -288.2620413764751675, -346.4429930266928750 ) ) ;
#42949 = CARTESIAN_POINT ( 'NONE',  ( -39.98801080995787771, -284.2583033967503638, -196.3951051445042140 ) ) ;
#42951 = CARTESIAN_POINT ( 'NONE',  ( -37.28949761074304803, -287.2913482865603783, -344.3744363224035396 ) ) ;
#42950 = CARTESIAN_POINT ( 'NONE',  ( -108.6687875047125829, -282.8898179301163509, -288.4669602723273556 ) ) ;
#42952 = CARTESIAN_POINT ( 'NONE',  ( 33.71175347916113907, -282.9994086819663721, -288.8106028473095535 ) ) ;
#42953 = CARTESIAN_POINT ( 'NONE',  ( -46.60797950018415747, -271.9343522617085114, -195.9357411689216804 ) ) ;
#42954 = CARTESIAN_POINT ( 'NONE',  ( -105.9498827348500498, -283.3819235057654282, -237.2045546385099897 ) ) ;
#42955 = CARTESIAN_POINT ( 'NONE',  ( -91.24150544929607065, -297.8187481375996413, -322.5129313227120633 ) ) ;
#42956 = CARTESIAN_POINT ( 'NONE',  ( -68.99698313679613193, -283.6367567159081204, -202.1710632356213750 ) ) ;
#42957 = CARTESIAN_POINT ( 'NONE',  ( -104.6630564907187306, -279.8794624052123936, -241.5298255218714587 ) ) ;
#42958 = CARTESIAN_POINT ( 'NONE',  ( 32.35228777691182955, -289.9200825889580528, -298.6561603426944771 ) ) ;
#42959 = DIRECTION ( 'NONE',  ( 0.000000000000000000, 1.000000000000000000, -0.000000000000000000 ) ) ;
#42960 = CARTESIAN_POINT ( 'NONE',  ( 186.6539576904058890, 293.9636489450775230, -11.60392986742922261 ) ) ;
#42961 = CARTESIAN_POINT ( 'NONE',  ( 26.89486623655271913, -296.0036506589205487, -310.2461187141660730 ) ) ;
#42962 = PRODUCT_RELATED_PRODUCT_CATEGORY ( 'part', '', ( #83658 ) ) ;
#42963 = CARTESIAN_POINT ( 'NONE',  ( -96.87572181362651236, -275.9274016452608862, -315.9758186221450842 ) ) ;
#42964 = CARTESIAN_POINT ( 'NONE',  ( -110.6309313194398811, -289.4566652400316684, -293.6185062433973485 ) ) ;
#42965 = CARTESIAN_POINT ( 'NONE',  ( -76.09530833945771633, -293.9787772851444174, -333.2267423522411605 ) ) ;
#42966 = CARTESIAN_POINT ( 'NONE',  ( -22.07572759736078538, -278.9365094385113366, -198.4187589170627746 ) ) ;
#42967 = CARTESIAN_POINT ( 'NONE',  ( -109.3263870912830953, -270.8798442382307030, -251.2027108781749689 ) ) ;
#42968 = CARTESIAN_POINT ( 'NONE',  ( -107.4772215038594823, -292.1569183094522373, -248.3584528825911093 ) ) ;
#42969 = CARTESIAN_POINT ( 'NONE',  ( 39.58706461736020543, -284.0519495502702512, -270.3284710469133074 ) ) ;
#42970 = CARTESIAN_POINT ( 'NONE',  ( -66.67596205403893350, -293.9093788545202983, -340.8181409362580894 ) ) ;
#42971 = CARTESIAN_POINT ( 'NONE',  ( -53.56477480331713537, -290.8639117648802994, -342.3559251638833416 ) ) ;
#42972 = CARTESIAN_POINT ( 'NONE',  ( -64.01186305909970997, -289.9490158890015437, -199.1532044938730621 ) ) ;
#42973 = CARTESIAN_POINT ( 'NONE',  ( -5.521347270807003049, -290.0503953247497293, -336.7150181181185076 ) ) ;
#42974 = CARTESIAN_POINT ( 'NONE',  ( 138.6539576904058606, 132.0000000000000568, 10.50000000000000000 ) ) ;
#42975 = CARTESIAN_POINT ( 'NONE',  ( -100.4380457336314834, -290.8464015569286971, -307.4940090770277266 ) ) ;
#42976 = CYLINDRICAL_SURFACE ( 'NONE', #30896, 2.000000000000005329 ) ;
#42977 = CARTESIAN_POINT ( 'NONE',  ( -112.7397341039777956, -291.5861654050265770, -283.9682415960828052 ) ) ;
#42979 = CARTESIAN_POINT ( 'NONE',  ( -106.9520964504961853, -290.2587069915728080, -292.5145035144574308 ) ) ;
#42978 = CARTESIAN_POINT ( 'NONE',  ( 5.275257023345053753, -278.6457423904747088, -208.2145029204482967 ) ) ;
#42980 = AXIS2_PLACEMENT_3D ( 'NONE', #9632, #52261, #44688 ) ;
#42981 = CARTESIAN_POINT ( 'NONE',  ( -39.59089506606640185, -280.3579449401496504, -193.4020806963975758 ) ) ;
#42982 = CARTESIAN_POINT ( 'NONE',  ( 23.38362003892255103, -281.8513012658209504, -317.6918225101389339 ) ) ;
#42983 = CARTESIAN_POINT ( 'NONE',  ( 36.73057395195334607, -285.7040377109205451, -282.2028423213719179 ) ) ;
#42984 = CARTESIAN_POINT ( 'NONE',  ( 208.6364533529840912, 29.41061770585039881, 14.73339628615688568 ) ) ;
#42985 = CARTESIAN_POINT ( 'NONE',  ( 27.93003924501046242, -280.1662176731669547, -305.7230398334868369 ) ) ;
#42986 = CARTESIAN_POINT ( 'NONE',  ( -112.1547656182552544, -282.6287637653284719, -264.3816528938895090 ) ) ;
#42987 = DIRECTION ( 'NONE',  ( -1.000000000000000000, -0.000000000000000000, -0.000000000000000000 ) ) ;
#42988 = CARTESIAN_POINT ( 'NONE',  ( -109.0915178644586518, -276.6992410593323939, -296.4902368657858460 ) ) ;
#42989 = VECTOR ( 'NONE', #25137, 1000.000000000000000 ) ;
#42990 = CARTESIAN_POINT ( 'NONE',  ( -113.1796386647707209, -283.6201004365038898, -258.6052285045099666 ) ) ;
#42991 = CARTESIAN_POINT ( 'NONE',  ( -56.91462729414405430, -274.5961634143266110, -199.8135862455631866 ) ) ;
#42992 = CARTESIAN_POINT ( 'NONE',  ( 192.9182251362765328, 275.0000000000000568, 16.22085278731030300 ) ) ;
#42993 = CARTESIAN_POINT ( 'NONE',  ( -28.02533708165118043, -293.7723706814070397, -197.1002125915819363 ) ) ;
#42994 = CARTESIAN_POINT ( 'NONE',  ( 37.60797985208085947, -277.1648375924737024, -285.2322902752480331 ) ) ;
#42995 = CARTESIAN_POINT ( 'NONE',  ( -8.734304219170786254, -276.3339693611055736, -337.5587720912180316 ) ) ;
#42996 = CARTESIAN_POINT ( 'NONE',  ( 13.73507041340559987, -296.3369496267696377, -325.3519369297682715 ) ) ;
#42997 = CARTESIAN_POINT ( 'NONE',  ( -87.38282391052821652, -289.8941038545590914, -328.9536744273229942 ) ) ;
#42998 = AXIS2_PLACEMENT_3D ( 'NONE', #93164, #14113, #79888 ) ;
#42999 = CARTESIAN_POINT ( 'NONE',  ( 38.20202039902547142, -279.5909893032552986, -267.1435502085005282 ) ) ;
#43000 = AXIS2_PLACEMENT_3D ( 'NONE', #36056, #71592, #79155 ) ;
#43001 = CARTESIAN_POINT ( 'NONE',  ( 22.21060817566707613, -292.7300162469010161, -221.5500272323206730 ) ) ;
#43002 = CARTESIAN_POINT ( 'NONE',  ( -104.9155595301911177, -289.9899980931524510, -241.9947906946783860 ) ) ;
#43003 = CARTESIAN_POINT ( 'NONE',  ( -76.07183415066907628, -293.5689970976574728, -334.6475355771692648 ) ) ;
#43004 = ORIENTED_EDGE ( 'NONE', *, *, #60248, .F. ) ;
#43005 = LINE ( 'NONE', #14140, #84734 ) ;
#43006 = CARTESIAN_POINT ( 'NONE',  ( -70.24281893392146969, -291.1139922498899750, -205.1268875266394502 ) ) ;
#43007 = DIRECTION ( 'NONE',  ( 0.000000000000000000, 0.000000000000000000, -1.000000000000000000 ) ) ;
#43008 = CARTESIAN_POINT ( 'NONE',  ( 30.91033621190086578, -272.8380690714490129, -254.8156830097664738 ) ) ;
#43009 = CARTESIAN_POINT ( 'NONE',  ( -113.9996203384661442, -295.5487917682976331, -275.3122152630396613 ) ) ;
#43010 = CARTESIAN_POINT ( 'NONE',  ( -112.0399466478455395, -285.6591695094882652, -286.8980536679063675 ) ) ;
#43011 = CARTESIAN_POINT ( 'NONE',  ( 18.66312710380852735, -286.7206643520017906, -223.5179380335132464 ) ) ;
#43012 = CARTESIAN_POINT ( 'NONE',  ( 33.18551471823606391, -277.3530738039769403, -291.7735628420287526 ) ) ;
#43013 = CARTESIAN_POINT ( 'NONE',  ( 13.45615586511399364, -292.3575378159243883, -325.1258565047109528 ) ) ;
#43014 = CARTESIAN_POINT ( 'NONE',  ( 36.43631108011300057, -295.3890312197223693, -276.2584965499544865 ) ) ;
#43015 = AXIS2_PLACEMENT_3D ( 'NONE', #80494, #20885, #86199 ) ;
#43016 = CARTESIAN_POINT ( 'NONE',  ( 35.98454281686093026, -274.2915732756347325, -266.1313019239624964 ) ) ;
#43017 = ORIENTED_EDGE ( 'NONE', *, *, #29167, .T. ) ;
#43018 = CARTESIAN_POINT ( 'NONE',  ( 194.5467258271157220, 40.92429273362547093, 14.24314089363953961 ) ) ;
#43019 = CARTESIAN_POINT ( 'NONE',  ( -110.3270113682650191, -295.9106256597181641, -294.8333192457906762 ) ) ;
#43020 = CARTESIAN_POINT ( 'NONE',  ( -20.78575138063733618, -290.7581399825188555, -342.9366975940424140 ) ) ;
#43021 = CARTESIAN_POINT ( 'NONE',  ( 201.0378816431136215, 294.4824024966172828, -54.00000000000627409 ) ) ;
#43022 = CARTESIAN_POINT ( 'NONE',  ( -36.91288064764863464, -299.1370683167476159, -193.6701508778304799 ) ) ;
#43023 = CARTESIAN_POINT ( 'NONE',  ( -0.9334829628409744284, -289.2068616029832242, -333.8097212761984451 ) ) ;
#43024 = VERTEX_POINT ( 'NONE', #1746 ) ;
#43025 = CARTESIAN_POINT ( 'NONE',  ( -84.41316979716314961, -278.4811890448138456, -209.6547865246078572 ) ) ;
#43026 = CARTESIAN_POINT ( 'NONE',  ( 26.43185067494878382, -294.7704193162263095, -313.3290944831168190 ) ) ;
#43027 = CARTESIAN_POINT ( 'NONE',  ( -77.50208864386091534, -287.7240688354767144, -334.6675509583748749 ) ) ;
#43028 = CARTESIAN_POINT ( 'NONE',  ( -53.28072217516110243, -295.5843197245558258, -345.7262813025665764 ) ) ;
#43029 = CARTESIAN_POINT ( 'NONE',  ( 19.35952538546157342, -293.2344275275639234, -224.3298394215769918 ) ) ;
#43030 = DIRECTION ( 'NONE',  ( -0.000000000000000000, -0.000000000000000000, -1.000000000000000000 ) ) ;
#43031 = DIRECTION ( 'NONE',  ( 0.000000000000000000, 0.000000000000000000, 1.000000000000000000 ) ) ;
#43032 = DIRECTION ( 'NONE',  ( -1.000000000000000000, 0.000000000000000000, 0.000000000000000000 ) ) ;
#43033 = CARTESIAN_POINT ( 'NONE',  ( 39.00903594524251616, -289.0869142496551945, -271.5212520357966923 ) ) ;
#43034 = CARTESIAN_POINT ( 'NONE',  ( -19.11405058567864046, -286.3380690714489560, -350.3683826091709648 ) ) ;
#43035 = VERTEX_POINT ( 'NONE', #51008 ) ;
#43036 = CARTESIAN_POINT ( 'NONE',  ( -19.77144108156758762, -279.6207711645471363, -195.4425501615428118 ) ) ;
#43037 = CARTESIAN_POINT ( 'NONE',  ( -1.529447730817133699, -284.5764642505654933, -336.0835382243644744 ) ) ;
#43038 = CARTESIAN_POINT ( 'NONE',  ( -113.6214010409390198, -283.0601168966554724, -275.6587063939135760 ) ) ;
#43039 = CARTESIAN_POINT ( 'NONE',  ( 15.08045641260617131, -286.3852148179146297, -323.2121510886523197 ) ) ;
#43040 = CARTESIAN_POINT ( 'NONE',  ( 7.528913281278284408, -278.3081279420530905, -331.4747033965260812 ) ) ;
#43041 = CARTESIAN_POINT ( 'NONE',  ( -65.82530665041743134, -274.0022405054091905, -203.1244341982884407 ) ) ;
#43042 = ORIENTED_EDGE ( 'NONE', *, *, #85122, .F. ) ;
#43044 = CARTESIAN_POINT ( 'NONE',  ( -110.4528495135877080, -277.9332010092538781, -267.8965625832013302 ) ) ;
#43043 = CARTESIAN_POINT ( 'NONE',  ( -99.46773070686191431, -279.0818708372468109, -231.9325004426448800 ) ) ;
#43045 = CARTESIAN_POINT ( 'NONE',  ( 17.85751899607230087, -275.8991674616297018, -217.0445142784453765 ) ) ;
#43046 = CARTESIAN_POINT ( 'NONE',  ( -113.9802245218702268, -277.3676166370366332, -268.7273205219454439 ) ) ;
#43047 = CARTESIAN_POINT ( 'NONE',  ( -95.96838508513684474, -238.3309465572374393, -339.6183069132351875 ) ) ;
#43048 = CARTESIAN_POINT ( 'NONE',  ( -81.51615232335547034, -297.0651251487017817, -332.7733388738899976 ) ) ;
#43049 = CARTESIAN_POINT ( 'NONE',  ( -37.37352853689063892, -288.5519495502701943, -195.3611179825600175 ) ) ;
#43050 = ORIENTED_EDGE ( 'NONE', *, *, #40194, .F. ) ;
#43051 = DIRECTION ( 'NONE',  ( -0.000000000000000000, -0.000000000000000000, -1.000000000000000000 ) ) ;
#43052 = CARTESIAN_POINT ( 'NONE',  ( -39.99883305194413197, -287.0976569310942068, -197.1001753257822031 ) ) ;
#43053 = CARTESIAN_POINT ( 'NONE',  ( -75.61595190626032092, -287.3093675063864794, -204.6571186150938502 ) ) ;
#43054 = CARTESIAN_POINT ( 'NONE',  ( -3.326323417341269906, -287.9394320132768712, -335.1230247582908532 ) ) ;
#43055 = CARTESIAN_POINT ( 'NONE',  ( -114.0899685434597757, -284.1363342471523765, -264.2468811833574023 ) ) ;
#43056 = CARTESIAN_POINT ( 'NONE',  ( 0.8310072182383487771, -278.9699686352900585, -207.1411680245042817 ) ) ;
#43057 = CARTESIAN_POINT ( 'NONE',  ( -37.30363014210946915, -287.9130126734615374, -196.1132745426634472 ) ) ;
#43058 = CARTESIAN_POINT ( 'NONE',  ( 5.340325040149338065, -279.1214896391054481, -210.2865603197639075 ) ) ;
#43059 = CARTESIAN_POINT ( 'NONE',  ( -54.04987631655905744, -278.5862322817555992, -341.9823189662692471 ) ) ;
#43060 = CARTESIAN_POINT ( 'NONE',  ( 26.82379824955405567, -276.5222960395601035, -305.4065193446833746 ) ) ;
#43061 = CARTESIAN_POINT ( 'NONE',  ( -1.997644142801269229, -287.3895289439580552, -338.3229192107883705 ) ) ;
#43062 = CARTESIAN_POINT ( 'NONE',  ( -94.27262595806554657, -284.6522828767522810, -321.9851690422206048 ) ) ;
#43063 = CARTESIAN_POINT ( 'NONE',  ( -1.657110631631045328, -283.0843707216288294, -338.5236955151176517 ) ) ;
#43064 = ORIENTED_EDGE ( 'NONE', *, *, #67705, .F. ) ;
#43065 = ORIENTED_EDGE ( 'NONE', *, *, #71361, .T. ) ;
#43066 = FACE_BOUND ( 'NONE', #6007, .T. ) ;
#43067 = CARTESIAN_POINT ( 'NONE',  ( -88.63751928321207174, -291.6232937575563824, -326.1199237050473698 ) ) ;
#43068 = CARTESIAN_POINT ( 'NONE',  ( -109.9574927611636639, -289.5440281105414897, -246.1071680132189385 ) ) ;
#43069 = AXIS2_PLACEMENT_3D ( 'NONE', #32683, #18942, #61569 ) ;
#43070 = CARTESIAN_POINT ( 'NONE',  ( -108.7617064387818147, -271.8239779507147773, -254.1564536063076787 ) ) ;
#43071 = CARTESIAN_POINT ( 'NONE',  ( 36.26969031211439898, -293.1823233105158124, -292.7827458807917083 ) ) ;
#43072 = CARTESIAN_POINT ( 'NONE',  ( -23.67540736367092435, -287.3543498106038214, -342.8283602820863507 ) ) ;
#43073 = CARTESIAN_POINT ( 'NONE',  ( 36.63486155438262415, -291.7616501970875902, -268.0282372174906413 ) ) ;
#43074 = CARTESIAN_POINT ( 'NONE',  ( -8.045972640272154308, -289.8648491861502521, -337.7124921573010283 ) ) ;
#43075 = CARTESIAN_POINT ( 'NONE',  ( -110.4542110544635705, -298.8376638359844719, -287.0812184334320705 ) ) ;
#43076 = CARTESIAN_POINT ( 'NONE',  ( 35.87812805681895867, -289.7616302273697215, -286.6635252069625039 ) ) ;
#43077 = CARTESIAN_POINT ( 'NONE',  ( -72.55183474986085912, -289.5870430541191354, -203.9366749534805479 ) ) ;
#43078 = CARTESIAN_POINT ( 'NONE',  ( -101.7150847837339143, -293.0686206528743014, -231.7766073015210111 ) ) ;
#43079 = CARTESIAN_POINT ( 'NONE',  ( -108.5972248506468389, -285.7164599226876476, -253.3938026246506183 ) ) ;
#43080 = CARTESIAN_POINT ( 'NONE',  ( 35.63574586544919498, -295.3215238158265947, -252.3522088893608952 ) ) ;
#43081 = CARTESIAN_POINT ( 'NONE',  ( -112.3417001281054723, -270.5523139186827279, -270.3356821209761165 ) ) ;
#43082 = CARTESIAN_POINT ( 'NONE',  ( 180.2288731078812702, 250.5000000000000568, -24.90909090909093848 ) ) ;
#43083 = CARTESIAN_POINT ( 'NONE',  ( -89.05288204568653043, -275.3098263147451235, -215.4777901952105026 ) ) ;
#43084 = CIRCLE ( 'NONE', #2259, 3.342139515347647638 ) ;
#43085 = CARTESIAN_POINT ( 'NONE',  ( -8.439839163762631102, -281.8610033199269651, -337.5718623625680266 ) ) ;
#43086 = CARTESIAN_POINT ( 'NONE',  ( -51.41756448579535999, -281.2318447457062121, -344.0814075003600010 ) ) ;
#43087 = CARTESIAN_POINT ( 'NONE',  ( -56.04090144877764601, -294.4842382318693694, -344.8896272254696100 ) ) ;
#43088 = CARTESIAN_POINT ( 'NONE',  ( 12.24178478955131588, -272.9929214192598579, -215.3425482218490572 ) ) ;
#43089 = CARTESIAN_POINT ( 'NONE',  ( -101.8425540965401268, -276.1311249352486925, -307.6258920054404484 ) ) ;
#43090 = CARTESIAN_POINT ( 'NONE',  ( -104.1739781119986645, -298.2783209675659464, -239.6658634530940617 ) ) ;
#43091 = CARTESIAN_POINT ( 'NONE',  ( 34.64775987874817531, -295.1779223414953321, -285.6824479857635311 ) ) ;
#43092 = CARTESIAN_POINT ( 'NONE',  ( 208.6208076322478746, 32.98517505407394168, 13.99999999999999822 ) ) ;
#43093 = CARTESIAN_POINT ( 'NONE',  ( -39.68398696466171316, -295.8851181770038465, -343.4975490098863702 ) ) ;
#43094 = CARTESIAN_POINT ( 'NONE',  ( 152.4536156746142410, 276.0000000000000568, 11.99999999999999289 ) ) ;
#43096 = CARTESIAN_POINT ( 'NONE',  ( -84.07483455525556337, -297.3891023827070512, -214.2146934236563709 ) ) ;
#43095 = CARTESIAN_POINT ( 'NONE',  ( -5.446708689715258345, -284.4897839715625310, -202.0887492806195382 ) ) ;
#43097 = CARTESIAN_POINT ( 'NONE',  ( -94.39915396130795955, -283.8495799133680180, -322.0860597705161581 ) ) ;
#43098 = CARTESIAN_POINT ( 'NONE',  ( 32.84385895012785284, -287.6228605759146149, -301.9796503380684953 ) ) ;
#43099 = CARTESIAN_POINT ( 'NONE',  ( 22.73330092127427449, -296.1512816504139209, -315.8517879605568623 ) ) ;
#43100 = CARTESIAN_POINT ( 'NONE',  ( 36.52767371428124932, -291.3968879094392150, -258.3081852475582423 ) ) ;
#43101 = CARTESIAN_POINT ( 'NONE',  ( -77.39959017020464671, -278.7268106503487957, -204.7287682977936072 ) ) ;
#43102 = CARTESIAN_POINT ( 'NONE',  ( -95.95921662488163406, -294.6952119285919025, -223.5744983911110353 ) ) ;
#43103 = DIRECTION ( 'NONE',  ( -1.000000000000000000, 0.000000000000000000, 0.000000000000000000 ) ) ;
#43104 = CARTESIAN_POINT ( 'NONE',  ( 32.22179632868873256, -286.0377678056952959, -246.9506402988595823 ) ) ;
#43105 = CARTESIAN_POINT ( 'NONE',  ( 200.2349812190172713, 66.43136063442170780, -7.741079165001064410 ) ) ;
#43106 = CARTESIAN_POINT ( 'NONE',  ( 183.0442525570908288, 293.9636489450775230, 0.000000000000000000 ) ) ;
#43107 = CARTESIAN_POINT ( 'NONE',  ( -108.6135127068038315, -298.4030657779300668, -251.1611522022819543 ) ) ;
#43108 = CARTESIAN_POINT ( 'NONE',  ( -22.69702909277681258, -281.6611815316325647, -195.3130139600934001 ) ) ;
#43110 = CARTESIAN_POINT ( 'NONE',  ( 30.33452865869570303, -281.9186277349919578, -297.7276679514509965 ) ) ;
#43109 = CARTESIAN_POINT ( 'NONE',  ( -80.94103828022655023, -293.6605088080333417, -331.8862703230191755 ) ) ;
#43111 = CARTESIAN_POINT ( 'NONE',  ( -105.2546098419397396, -297.1890518288208796, -233.9597594180537214 ) ) ;
#43112 = CARTESIAN_POINT ( 'NONE',  ( -80.14634731296082748, -298.9808505886986154, -210.3738699193686728 ) ) ;
#43113 = CARTESIAN_POINT ( 'NONE',  ( 31.41209627129236992, -285.2222962678480940, -238.8945313818403520 ) ) ;
#43114 = CARTESIAN_POINT ( 'NONE',  ( -109.8054437565513837, -280.8014833013458542, -250.9722235702734849 ) ) ;
#43115 = CARTESIAN_POINT ( 'NONE',  ( -102.7370592014746080, -296.0582745058885052, -237.2807484572368253 ) ) ;
#43116 = ORIENTED_EDGE ( 'NONE', *, *, #18686, .F. ) ;
#43117 = CYLINDRICAL_SURFACE ( 'NONE', #45313, 1.499999999999998002 ) ;
#43118 = CARTESIAN_POINT ( 'NONE',  ( -64.63379755445335206, -285.3901504232107413, -339.8376479859867345 ) ) ;
#43119 = CARTESIAN_POINT ( 'NONE',  ( 41.08708295871279859, -296.0521521680024080, -472.6442049081569508 ) ) ;
#43120 = CARTESIAN_POINT ( 'NONE',  ( -20.19161114001082069, -283.7666405000204009, -195.3683826091709363 ) ) ;
#43121 = CARTESIAN_POINT ( 'NONE',  ( 33.56848811359044760, -274.3706063330832876, -240.6279754453531154 ) ) ;
#43122 = EDGE_CURVE ( 'NONE', #57485, #51305, #30845, .T. ) ;
#43123 = EDGE_CURVE ( 'NONE', #307, #12757, #48055, .T. ) ;
#43124 = CARTESIAN_POINT ( 'NONE',  ( 23.34242617102849238, -292.8219737722124023, -229.7848093798835976 ) ) ;
#43125 = CARTESIAN_POINT ( 'NONE',  ( 34.12324776698246609, -282.8365456831581923, -252.3246610363836737 ) ) ;
#43126 = CARTESIAN_POINT ( 'NONE',  ( 32.02057755700564456, -277.4862305546627681, -295.7151879516842996 ) ) ;
#43127 = CARTESIAN_POINT ( 'NONE',  ( 31.67653161100110637, -283.5715295707567520, -302.7798371038574601 ) ) ;
#43128 = CARTESIAN_POINT ( 'NONE',  ( 13.62179459227293776, -279.5800448321840577, -217.4712203547014155 ) ) ;
#43129 = CARTESIAN_POINT ( 'NONE',  ( -86.82225947929823917, -281.3639507526208945, -213.9991193285531779 ) ) ;
#43130 = CARTESIAN_POINT ( 'NONE',  ( 99.18597135844251511, -299.7172817242040992, -193.3609922739482556 ) ) ;
#43131 = CARTESIAN_POINT ( 'NONE',  ( 33.71436872516444794, -275.0066564734262329, -240.5580124021094832 ) ) ;
#43132 = CARTESIAN_POINT ( 'NONE',  ( 36.32943497150740342, -295.3342596619310143, -259.6897520325212554 ) ) ;
#43133 = CARTESIAN_POINT ( 'NONE',  ( 199.6702811234769968, 65.52214591209386185, -9.100946541886345997 ) ) ;
#43134 = LINE ( 'NONE', #6699, #88922 ) ;
#43135 = CARTESIAN_POINT ( 'NONE',  ( 28.48949586576387105, -292.1879562902235534, -307.9711640323280335 ) ) ;
#43136 = CARTESIAN_POINT ( 'NONE',  ( -21.91492666388166199, -273.7628683894821506, -198.9468119792075811 ) ) ;
#43137 =( GEOMETRIC_REPRESENTATION_CONTEXT ( 3 ) GLOBAL_UNCERTAINTY_ASSIGNED_CONTEXT ( ( #11601 ) ) GLOBAL_UNIT_ASSIGNED_CONTEXT ( ( #72501, #21849, #14750 ) ) REPRESENTATION_CONTEXT ( 'NONE', 'WORKASPACE' ) );
#43138 = CARTESIAN_POINT ( 'NONE',  ( 20.76974850472888789, -294.3992066522878872, -220.8864631929152722 ) ) ;
#43140 = CARTESIAN_POINT ( 'NONE',  ( -40.63081006024501107, -293.2167509284273024, -193.8157199773786772 ) ) ;
#43139 = CARTESIAN_POINT ( 'NONE',  ( -112.3452863284742875, -275.1604526064900824, -261.9424758988611188 ) ) ;
#43141 = CARTESIAN_POINT ( 'NONE',  ( -42.77214904491643210, -291.1208601627756138, -345.0490337553362679 ) ) ;
#43142 = CARTESIAN_POINT ( 'NONE',  ( -90.40330567983866672, -275.8047274803942628, -323.2030369195602475 ) ) ;
#43143 = CARTESIAN_POINT ( 'NONE',  ( -43.29841267956833661, -279.0481235032263498, -344.5624102469091099 ) ) ;
#43144 = CARTESIAN_POINT ( 'NONE',  ( 2.316716786032549713, -292.5966299899486671, -333.4183780738695759 ) ) ;
#43145 = CARTESIAN_POINT ( 'NONE',  ( 34.98932837053446576, -283.1246450727509227, -247.8105570810429299 ) ) ;
#43146 = CIRCLE ( 'NONE', #17400, 0.4999999999999991118 ) ;
#43147 = CARTESIAN_POINT ( 'NONE',  ( -109.7241501330076119, -283.6261508395967894, -258.6624437431430010 ) ) ;
#43148 = ORIENTED_EDGE ( 'NONE', *, *, #50173, .F. ) ;
#43149 = CARTESIAN_POINT ( 'NONE',  ( 3.398499492847016690, -282.1547360494830059, -331.0219785869745124 ) ) ;
#43150 = CARTESIAN_POINT ( 'NONE',  ( -39.59202080859100192, -281.1042144791311443, -193.6902528982587626 ) ) ;
#43151 = CARTESIAN_POINT ( 'NONE',  ( -111.3336391416264775, -283.5989161604972537, -250.3325926131205108 ) ) ;
#43152 = CARTESIAN_POINT ( 'NONE',  ( -94.79367732475492403, -280.1852755811136149, -219.4485406614516876 ) ) ;
#43153 = SHAPE_REPRESENTATION_RELATIONSHIP ( 'NONE' , 'NONE' ,  #49383, #12545 ) ;
#43154 = CARTESIAN_POINT ( 'NONE',  ( -98.23830774821144018, -279.4540776291964335, -316.3641934583372404 ) ) ;
#43155 = CARTESIAN_POINT ( 'NONE',  ( -37.37352853689063181, -274.5523547857346784, -340.3611179825599606 ) ) ;
#43156 = ORIENTED_EDGE ( 'NONE', *, *, #3235, .T. ) ;
#43157 = ORIENTED_EDGE ( 'NONE', *, *, #40105, .F. ) ;
#43158 = CARTESIAN_POINT ( 'NONE',  ( -40.63048489267862351, -300.0109735804684306, -195.4203633066897794 ) ) ;
#43159 = CARTESIAN_POINT ( 'NONE',  ( -110.0949494014835466, -276.3561144569253543, -287.1154956881167095 ) ) ;
#43160 = CARTESIAN_POINT ( 'NONE',  ( -111.3357030163400054, -292.5313809838983730, -253.0735052437564434 ) ) ;
#43161 = CARTESIAN_POINT ( 'NONE',  ( 35.52537832964075193, -292.9778651859134015, -276.2161623890235660 ) ) ;
#43162 = CARTESIAN_POINT ( 'NONE',  ( -112.5784700627718991, -290.2619637076062986, -254.2068949525582582 ) ) ;
#43163 = CARTESIAN_POINT ( 'NONE',  ( 208.6208076322478746, 32.98517505407394168, 10.50000000000000000 ) ) ;
#43165 = CARTESIAN_POINT ( 'NONE',  ( -75.11223442820546836, -283.9396528411556346, -206.9590111263654251 ) ) ;
#43164 = CARTESIAN_POINT ( 'NONE',  ( 37.20503191951331701, -292.3390388943843163, -287.1948284796106918 ) ) ;
#43166 = CARTESIAN_POINT ( 'NONE',  ( -91.67919673014479542, -293.1278624160604522, -219.7626570154602632 ) ) ;
#43167 = CARTESIAN_POINT ( 'NONE',  ( 9.485835014756968775, -285.1896870155832175, -213.4586601889024848 ) ) ;
#43168 = CARTESIAN_POINT ( 'NONE',  ( -21.26412956754484895, -284.1569110213982299, -342.1264904004002574 ) ) ;
#43169 = CARTESIAN_POINT ( 'NONE',  ( -43.15249233114293048, -290.0650829187710542, -346.9055815769275455 ) ) ;
#43170 = CARTESIAN_POINT ( 'NONE',  ( 22.15997060491829629, -281.4527292910796632, -227.9637168623945058 ) ) ;
#43171 = CARTESIAN_POINT ( 'NONE',  ( 38.84046996665242801, -292.4539969654507559, -278.8661077269548514 ) ) ;
#43172 = CARTESIAN_POINT ( 'NONE',  ( -36.07922049771882200, -289.8395626299993069, -347.2023528754664312 ) ) ;
#43173 = CARTESIAN_POINT ( 'NONE',  ( -112.8064066322788079, -290.8560805461020777, -285.4146964588423430 ) ) ;
#43174 = CARTESIAN_POINT ( 'NONE',  ( -108.0291923993588341, -284.9594647674005046, -252.1326117100746274 ) ) ;
#43175 = ORIENTED_EDGE ( 'NONE', *, *, #59326, .T. ) ;
#43176 = CARTESIAN_POINT ( 'NONE',  ( 189.9243309297870610, 250.5000000000000568, 20.22542485937349355 ) ) ;
#43177 = CARTESIAN_POINT ( 'NONE',  ( -25.08392384678993636, -296.7580026720443698, -345.1809718579603441 ) ) ;
#43178 = CARTESIAN_POINT ( 'NONE',  ( -74.38238042461829025, -294.2185329525826774, -337.3628643076092430 ) ) ;
#43179 = CARTESIAN_POINT ( 'NONE',  ( -94.96859516353185882, -278.2462975274661403, -225.1463653065975734 ) ) ;
#43180 = CARTESIAN_POINT ( 'NONE',  ( -70.09986567011543457, -273.1397759288119573, -200.7304146571214005 ) ) ;
#43181 = CARTESIAN_POINT ( 'NONE',  ( -41.09370002469045602, -293.5800674306174187, -343.9715643559873115 ) ) ;
#43182 = CARTESIAN_POINT ( 'NONE',  ( 35.16168541606742082, -277.5058202653120247, -285.2350246849453015 ) ) ;
#43183 = CARTESIAN_POINT ( 'NONE',  ( -103.1140283917687839, -271.1537135675578156, -235.8279615827835869 ) ) ;
#43184 = CARTESIAN_POINT ( 'NONE',  ( 15.14880353323818518, -294.0182675175411759, -218.9865118218939699 ) ) ;
#43185 = CARTESIAN_POINT ( 'NONE',  ( -93.30952029014373750, -296.9615348438026103, -317.7285187922821024 ) ) ;
#43186 = DIRECTION ( 'NONE',  ( 0.000000000000000000, 1.000000000000000000, 0.000000000000000000 ) ) ;
#43187 = CARTESIAN_POINT ( 'NONE',  ( -100.7557193666334996, -295.0938930831584344, -230.0040790715417245 ) ) ;
#43188 = CARTESIAN_POINT ( 'NONE',  ( -36.90591992003509603, -298.7088833530352758, -193.4630033034831627 ) ) ;
#43189 = CARTESIAN_POINT ( 'NONE',  ( 34.58274047468821522, -286.3312780081349729, -285.9845234415230948 ) ) ;
#43190 = CARTESIAN_POINT ( 'NONE',  ( -36.74506159037600383, -276.0598066130880284, -195.3507321840570228 ) ) ;
#43191 = CARTESIAN_POINT ( 'NONE',  ( -78.29610070260136467, -290.5590415597208676, -331.1357981330311873 ) ) ;
#43192 = CARTESIAN_POINT ( 'NONE',  ( -106.7903684750227740, -273.4693186665585358, -237.2490451406089562 ) ) ;
#43193 = CARTESIAN_POINT ( 'NONE',  ( -75.66554140224893388, -295.9118751780163166, -332.5760849177794967 ) ) ;
#43194 = CARTESIAN_POINT ( 'NONE',  ( -99.10266487916675260, -279.9488245874191534, -313.5350688882363102 ) ) ;
#43195 = CARTESIAN_POINT ( 'NONE',  ( -113.8840718870465025, -277.2575360720655908, -268.7279513365879779 ) ) ;
#43196 = CARTESIAN_POINT ( 'NONE',  ( -71.70064926505257574, -282.8428543491347682, -339.1562878804249976 ) ) ;
#43197 = CARTESIAN_POINT ( 'NONE',  ( 23.55720624841553956, -274.2730564956050330, -223.3861306643977969 ) ) ;
#43198 = CARTESIAN_POINT ( 'NONE',  ( -35.33644442437506683, -278.4767734867814397, -194.1745045521862210 ) ) ;
#43199 = CARTESIAN_POINT ( 'NONE',  ( 21.45751705949315991, -278.9096077347263076, -223.5145792692347300 ) ) ;
#43200 = CARTESIAN_POINT ( 'NONE',  ( -93.98298991252788426, -295.8966078572881884, -223.5119845526984079 ) ) ;
#43201 = CARTESIAN_POINT ( 'NONE',  ( 4.028684547046823106, -278.4954588719372168, -332.9805170302796000 ) ) ;
#43202 = CARTESIAN_POINT ( 'NONE',  ( 154.0637704119390321, 19.72112694978655512, 13.30738029212319340 ) ) ;
#43203 = CARTESIAN_POINT ( 'NONE',  ( 7.884347619584023192, -290.6862075724064880, -210.0215106034997632 ) ) ;
#43204 = CARTESIAN_POINT ( 'NONE',  ( -3.321352055266363124, -292.4889651421707981, -201.2696962055109395 ) ) ;
#43205 = CARTESIAN_POINT ( 'NONE',  ( 14.73801679728006953, -276.7838768352112311, -216.1602738029803277 ) ) ;
#43206 = CARTESIAN_POINT ( 'NONE',  ( -47.49694680946925018, -295.9227495756036888, -196.1675456646217128 ) ) ;
#43207 = CARTESIAN_POINT ( 'NONE',  ( -89.76858360487166522, -284.5322756325821842, -214.1142050115937252 ) ) ;
#43208 =( NAMED_UNIT ( * ) SI_UNIT ( $, .STERADIAN. ) SOLID_ANGLE_UNIT ( ) );
#43209 = CARTESIAN_POINT ( 'NONE',  ( -101.3525388959677542, -282.0267410142292306, -309.5440909481995959 ) ) ;
#43210 = VECTOR ( 'NONE', #7861, 1000.000000000000000 ) ;
#43211 = LINE ( 'NONE', #29004, #58810 ) ;
#43212 = CARTESIAN_POINT ( 'NONE',  ( -9.563045460428373445, -291.2181804358820614, -202.3697337995337193 ) ) ;
#43213 = CARTESIAN_POINT ( 'NONE',  ( -37.25605685649913568, -284.1927833791692137, -196.1133150158942442 ) ) ;
#43214 = CARTESIAN_POINT ( 'NONE',  ( 196.1554417525619272, 24.76049057409047549, 13.68028117252083042 ) ) ;
#43215 = LINE ( 'NONE', #27139, #92647 ) ;
#43216 = CARTESIAN_POINT ( 'NONE',  ( 22.09296495084021217, -292.1788802303631769, -316.1262207855465931 ) ) ;
#43217 = CARTESIAN_POINT ( 'NONE',  ( -108.6619060583244618, -282.6838120222776638, -297.6402818262262713 ) ) ;
#43218 = CARTESIAN_POINT ( 'NONE',  ( -26.88827593870426114, -278.5171435650348712, -343.4170303822178880 ) ) ;
#43219 = CARTESIAN_POINT ( 'NONE',  ( -111.1049538694434062, -285.4969461246036531, -291.0248813545133544 ) ) ;
#43220 = CARTESIAN_POINT ( 'NONE',  ( -5.798649145682235329, -286.4787492498483630, -204.5139387041926113 ) ) ;
#43221 = CARTESIAN_POINT ( 'NONE',  ( -94.90266296159016690, -279.3348759963886891, -316.2300187250377803 ) ) ;
#43222 = CARTESIAN_POINT ( 'NONE',  ( -89.59605644901319010, -280.0952124059233483, -219.0830218228622925 ) ) ;
#43223 = EDGE_CURVE ( 'NONE', #55107, #38347, #36339, .T. ) ;
#43224 = CARTESIAN_POINT ( 'NONE',  ( -60.03904446582659205, -287.7394642787486418, -198.4510519825464883 ) ) ;
#43225 = ORIENTED_EDGE ( 'NONE', *, *, #79581, .F. ) ;
#43226 = CARTESIAN_POINT ( 'NONE',  ( 19.39083834128441808, -298.5773980873777305, -193.3626504022654160 ) ) ;
#43227 = CARTESIAN_POINT ( 'NONE',  ( -69.44299170516677577, -291.4566251049550942, -337.7506860642808988 ) ) ;
#43228 = FACE_OUTER_BOUND ( 'NONE', #1517, .T. ) ;
#43229 = CARTESIAN_POINT ( 'NONE',  ( -19.11405058567862625, -288.7662352645559167, -190.3538533559490702 ) ) ;
#43230 = ORIENTED_EDGE ( 'NONE', *, *, #66684, .F. ) ;
#43231 = CARTESIAN_POINT ( 'NONE',  ( 3.879575505991686324, -272.6051628109363492, -207.4436833820658705 ) ) ;
#43232 = ADVANCED_FACE ( 'NONE', ( #71890 ), #83737, .T. ) ;
#43233 = CARTESIAN_POINT ( 'NONE',  ( 25.83694142330487864, -292.5192410161683370, -312.9627572360799945 ) ) ;
#43234 = CARTESIAN_POINT ( 'NONE',  ( 32.92894111148237357, -288.7802857845354083, -248.1210532869659460 ) ) ;
#43235 = CARTESIAN_POINT ( 'NONE',  ( -8.878075120584858482, -282.1898331116839245, -202.0398470186532052 ) ) ;
#43236 = CARTESIAN_POINT ( 'NONE',  ( 24.21771394611131711, -288.3714762427218830, -225.0947415768949043 ) ) ;
#43237 = CARTESIAN_POINT ( 'NONE',  ( 37.34719363658153668, -289.0767546778642441, -287.0001107046767288 ) ) ;
#43238 = CARTESIAN_POINT ( 'NONE',  ( -72.31965602083955957, -285.5151786706056782, -336.7052454764717595 ) ) ;
#43239 = CARTESIAN_POINT ( 'NONE',  ( -107.4200032711850668, -279.1281020763574929, -238.3261315319869311 ) ) ;
#43240 = ORIENTED_EDGE ( 'NONE', *, *, #37019, .T. ) ;
#43241 = CARTESIAN_POINT ( 'NONE',  ( -25.16444040404978466, -292.9780412936349308, -344.9864740904712903 ) ) ;
#43242 = CARTESIAN_POINT ( 'NONE',  ( 26.72070855840134840, -281.9477855309365850, -313.0812279752951781 ) ) ;
#43243 = CARTESIAN_POINT ( 'NONE',  ( 53.85457608967112719, -301.1225409177318966, -195.8910045484337559 ) ) ;
#43244 = CARTESIAN_POINT ( 'NONE',  ( 10.59707575819634329, -295.1948066931273615, -210.1954327657594490 ) ) ;
#43245 = CARTESIAN_POINT ( 'NONE',  ( -24.31103652693491313, -272.4560338893585367, -195.4466184879564423 ) ) ;
#43246 = DIRECTION ( 'NONE',  ( 1.000000000000000000, 0.000000000000000000, 0.000000000000000000 ) ) ;
#43247 = CARTESIAN_POINT ( 'NONE',  ( -68.54388738667908854, -279.1383285948262483, -204.2974218086809515 ) ) ;
#43248 = CARTESIAN_POINT ( 'NONE',  ( 39.22725684168179328, -276.8030930094064956, -274.0096683686523420 ) ) ;
#43249 = CARTESIAN_POINT ( 'NONE',  ( -69.53153403600639137, -299.0451586492719116, -204.1856730493908287 ) ) ;
#43250 = CARTESIAN_POINT ( 'NONE',  ( -76.64775181619921796, -282.6230497585922308, -336.3610164745032307 ) ) ;
#43251 = CARTESIAN_POINT ( 'NONE',  ( -110.6231407632999719, -292.1760253294439735, -280.8347428600993680 ) ) ;
#43252 = CARTESIAN_POINT ( 'NONE',  ( -55.16645527656131520, -275.4267189769729498, -196.2752318955378144 ) ) ;
#43253 = CARTESIAN_POINT ( 'NONE',  ( -98.78319446693210182, -298.3690761968088054, -224.5904332186586885 ) ) ;
#43254 = CARTESIAN_POINT ( 'NONE',  ( 18.46433878467093237, -296.2481679967467016, -320.2373853464923741 ) ) ;
#43255 = CARTESIAN_POINT ( 'NONE',  ( -105.8004833355823990, -282.1552425038193519, -300.5840136956837796 ) ) ;
#43256 = CARTESIAN_POINT ( 'NONE',  ( -70.88466519850025804, -291.2883631443361310, -201.0746562027783568 ) ) ;
#43257 = CARTESIAN_POINT ( 'NONE',  ( -86.37198171729069429, -271.3881392679651299, -214.0083393153563236 ) ) ;
#43258 = CARTESIAN_POINT ( 'NONE',  ( -32.37908468025877795, -287.7138385185117500, -194.3098555151815106 ) ) ;
#43259 = CARTESIAN_POINT ( 'NONE',  ( -72.76430206339378515, -290.4919619211961503, -206.1210174028015274 ) ) ;
#43260 = ORIENTED_EDGE ( 'NONE', *, *, #80560, .F. ) ;
#43261 = CARTESIAN_POINT ( 'NONE',  ( -106.7177755994177062, -289.5411533969804054, -238.2106539605180728 ) ) ;
#43262 = CARTESIAN_POINT ( 'NONE',  ( -53.41731125654033008, -288.9308133339569054, -341.5907621872297568 ) ) ;
#43263 = VERTEX_POINT ( 'NONE', #14585 ) ;
#43264 = CARTESIAN_POINT ( 'NONE',  ( -2.376156507956105557, -287.5834482175696394, -202.0902664909766600 ) ) ;
#43265 = CARTESIAN_POINT ( 'NONE',  ( -9.976501702364563684, -277.0180184902516771, -338.0742699716790298 ) ) ;
#43266 = CARTESIAN_POINT ( 'NONE',  ( 36.78735426201755843, -292.2248304585155552, -250.6539726117766236 ) ) ;
#43267 = CARTESIAN_POINT ( 'NONE',  ( -61.19216622462478483, -284.0051661692461380, -343.5225951486555687 ) ) ;
#43268 = CARTESIAN_POINT ( 'NONE',  ( -111.0865003937758360, -284.6077743733175680, -292.4851232668260081 ) ) ;
#43269 = CARTESIAN_POINT ( 'NONE',  ( -59.74415356586015946, -280.0872254151739185, -200.8080299144439778 ) ) ;
#43270 = CARTESIAN_POINT ( 'NONE',  ( 200.1467820935076247, 289.4019165369547864, -97.55132449765557112 ) ) ;
#43271 = CARTESIAN_POINT ( 'NONE',  ( -113.1125314665755326, -270.0723479569915071, -296.1281988589327625 ) ) ;
#43272 = CARTESIAN_POINT ( 'NONE',  ( -112.7804352628385942, -270.4057570101002170, -283.7043318166019503 ) ) ;
#43273 = CARTESIAN_POINT ( 'NONE',  ( -81.15956189548737143, -272.6368720216149768, -211.7091883079189643 ) ) ;
#43274 = CARTESIAN_POINT ( 'NONE',  ( 23.31579562908844849, -273.9021136340691669, -229.1695016566848153 ) ) ;
#43275 = CARTESIAN_POINT ( 'NONE',  ( -4.534469127212947370, -294.1390577145843395, -339.9687685013685154 ) ) ;
#43276 = CARTESIAN_POINT ( 'NONE',  ( -46.41228527574025264, -155.8298051699933637, -361.8999249830316671 ) ) ;
#43277 = CARTESIAN_POINT ( 'NONE',  ( -92.80305917252677261, -271.9620699616363595, -217.6415687889847277 ) ) ;
#43278 = CARTESIAN_POINT ( 'NONE',  ( -103.6460653980246605, -298.8594916326841258, -236.8610153399096419 ) ) ;
#43279 = CARTESIAN_POINT ( 'NONE',  ( -21.00352826219625868, -290.1532573003599964, -342.0152010249061050 ) ) ;
#43280 = ORIENTED_EDGE ( 'NONE', *, *, #43123, .T. ) ;
#43281 = CARTESIAN_POINT ( 'NONE',  ( 1.660245709109334111, -295.4851653861246064, -336.4797116896423859 ) ) ;
#43282 = AXIS2_PLACEMENT_3D ( 'NONE', #83645, #18809, #47666 ) ;
#43283 = CARTESIAN_POINT ( 'NONE',  ( 16.93213062955296877, -287.3445431787742450, -221.4308924556462728 ) ) ;
#43284 = CARTESIAN_POINT ( 'NONE',  ( -18.61210145447150310, -273.2081048368760889, -195.9376663295639105 ) ) ;
#43285 = CARTESIAN_POINT ( 'NONE',  ( -22.11951685482733865, -295.6647449400144296, -345.6767468812231527 ) ) ;
#43286 = CARTESIAN_POINT ( 'NONE',  ( -30.59010156213546949, -295.4612841546360755, -347.0027699742334448 ) ) ;
#43287 = CARTESIAN_POINT ( 'NONE',  ( -93.44119962011100711, -291.3817306201440260, -223.6313666735525203 ) ) ;
#43288 = EDGE_LOOP ( 'NONE', ( #54099, #11126 ) ) ;
#43289 = CARTESIAN_POINT ( 'NONE',  ( -60.45435088872834939, -275.6750119947716939, -198.3682175567925583 ) ) ;
#43290 = CARTESIAN_POINT ( 'NONE',  ( 28.74559755987726817, -274.8539148956148210, -309.0971193516192557 ) ) ;
#43291 = ORIENTED_EDGE ( 'NONE', *, *, #23628, .T. ) ;
#43292 = CARTESIAN_POINT ( 'NONE',  ( -111.6699499877698543, -278.3093785009016869, -250.4397351406170174 ) ) ;
#43293 = CARTESIAN_POINT ( 'NONE',  ( -31.25362233522507793, -272.5301614271577932, -196.7998713559981638 ) ) ;
#43294 = CARTESIAN_POINT ( 'NONE',  ( -105.7094784867675372, -273.9855412800620229, -243.7621276016092224 ) ) ;
#43295 = CARTESIAN_POINT ( 'NONE',  ( 35.07251602293275283, -276.3485031598098089, -259.3411214982757542 ) ) ;
#43296 = CARTESIAN_POINT ( 'NONE',  ( 26.07238527888006274, -276.7544003094457139, -228.4967203951786985 ) ) ;
#43297 = CARTESIAN_POINT ( 'NONE',  ( 26.24702249500338880, -274.1149082048291916, -310.8917261157436087 ) ) ;
#43298 = CARTESIAN_POINT ( 'NONE',  ( -7.939707988022100871, -295.3079015963584197, -337.3031510345140873 ) ) ;
#43299 = CARTESIAN_POINT ( 'NONE',  ( 35.88355451779958116, -292.0247527485320234, -262.5573234989684011 ) ) ;
#43300 = LINE ( 'NONE', #72197, #27577 ) ;
#43301 = CARTESIAN_POINT ( 'NONE',  ( -74.98330416502069795, -280.0569413540614505, -203.2594298606140057 ) ) ;
#43302 = CARTESIAN_POINT ( 'NONE',  ( -61.78782538194374041, -277.5454475925818656, -339.1999360838503321 ) ) ;
#43303 = ADVANCED_FACE ( 'NONE', ( #86513 ), #48810, .T. ) ;
#43304 =( BOUNDED_SURFACE ( )  B_SPLINE_SURFACE ( 3, 2, ( 
 ( #1829, #17446, #29795 ),
 ( #24065, #81353, #16503 ),
 ( #31193, #65804, #59614 ),
 ( #916, #23612, #46296 ),
 ( #51539, #38263, #22666 ),
 ( #87980, #67176, #30716 ),
 ( #31646, #60536, #2309 ),
 ( #53412, #37342, #60078 ),
 ( #16048, #45355, #74257 ),
 ( #88465, #88915, #30246 ) ),
 .UNSPECIFIED., .F., .F., .F. ) 
 B_SPLINE_SURFACE_WITH_KNOTS ( ( 4, 2, 2, 2, 4 ),
 ( 3, 3 ),
 ( 3.665191429188113137, 3.926990816987257382, 4.188790204786401183, 4.450589592585545873, 4.712388980384689674 ),
 ( 0.000000000000000000, 1.000000000000000000 ),
 .UNSPECIFIED. ) 
 GEOMETRIC_REPRESENTATION_ITEM ( )  RATIONAL_B_SPLINE_SURFACE ( (
 ( 1.000000000000000000, 0.7905694150420956579, 1.000000000000000000),
 ( 1.000000000000000000, 0.8144940228940678040, 1.000000000000000000),
 ( 1.000000000000000000, 0.8408337462336906709, 1.000000000000000000),
 ( 1.000000000000000000, 0.8912170613351929616, 1.000000000000000000),
 ( 1.000000000000000000, 0.9152160855742275114, 1.000000000000000000),
 ( 1.000000000000000000, 0.9556126078127453738, 1.000000000000000000),
 ( 1.000000000000000000, 0.9720148405105977218, 1.000000000000000000),
 ( 1.000000000000000000, 0.9942062568699685521, 1.000000000000000000),
 ( 1.000000000000000000, 1.000000000000000000, 1.000000000000000000),
 ( 1.000000000000000000, 1.000000000000000000, 1.000000000000000000) ) ) 
 REPRESENTATION_ITEM ( '' )  SURFACE ( )  );
#43305 = CARTESIAN_POINT ( 'NONE',  ( -43.60905962804377367, -284.6595001588505625, -194.0584888816471789 ) ) ;
#43306 = CARTESIAN_POINT ( 'NONE',  ( -76.11419864232016153, -297.5686729812242106, -334.8167050964337363 ) ) ;
#43307 = CARTESIAN_POINT ( 'NONE',  ( 82.65653505821647684, -298.9546730799231682, -197.7944811758501658 ) ) ;
#43308 = CARTESIAN_POINT ( 'NONE',  ( 35.79093094395190633, -286.7942834391931228, -273.7775422583916338 ) ) ;
#43309 = CARTESIAN_POINT ( 'NONE',  ( -70.93245602562748786, -275.7415489234395523, -336.3128816752575858 ) ) ;
#43310 = CARTESIAN_POINT ( 'NONE',  ( -107.6851990893781732, -276.8408554166956037, -292.1459412301165912 ) ) ;
#43311 = CARTESIAN_POINT ( 'NONE',  ( -107.4488627061712549, -286.2044010744293701, -297.1507758768117924 ) ) ;
#43312 = CARTESIAN_POINT ( 'NONE',  ( -64.46568126181904290, -278.6191963512717962, -338.6164074463517295 ) ) ;
#43313 = DIRECTION ( 'NONE',  ( -1.000000000000000000, 0.000000000000000000, 0.000000000000000000 ) ) ;
#43314 = CARTESIAN_POINT ( 'NONE',  ( 35.72054554733345810, -274.2269137257707712, -292.0484766116023252 ) ) ;
#43315 = CARTESIAN_POINT ( 'NONE',  ( 35.68832738967930851, -276.1477633948825314, -266.1248067559043875 ) ) ;
#43316 = CARTESIAN_POINT ( 'NONE',  ( 34.83207928417526489, -283.2820090341699597, -249.3156487456021750 ) ) ;
#43317 = CARTESIAN_POINT ( 'NONE',  ( 222.8344101925596306, -44.55766379199612004, 22.50000000000000000 ) ) ;
#43318 = CARTESIAN_POINT ( 'NONE',  ( -15.34759292839868472, -290.6899029083019741, -342.7039601795158319 ) ) ;
#43319 = CARTESIAN_POINT ( 'NONE',  ( 21.63712020873050790, -290.9157949897243043, -224.0104072398715971 ) ) ;
#43320 = DIRECTION ( 'NONE',  ( 1.000000000000000000, 0.000000000000000000, 0.000000000000000000 ) ) ;
#43321 = CARTESIAN_POINT ( 'NONE',  ( -37.80973136786009547, -296.8410831529566281, -196.9655360109972833 ) ) ;
#43322 = CARTESIAN_POINT ( 'NONE',  ( -55.28842110563833501, -289.9584019965592461, -198.3279264411563929 ) ) ;
#43323 = CARTESIAN_POINT ( 'NONE',  ( -75.10193482699480683, -210.9688814900462432, -359.8487438039043127 ) ) ;
#43324 = CARTESIAN_POINT ( 'NONE',  ( 208.4306832106270804, -124.2391364535881024, -6.500000000000033751 ) ) ;
#43325 = CARTESIAN_POINT ( 'NONE',  ( -112.6786424774967941, -288.8789971993604695, -282.4876537846278666 ) ) ;
#43326 = CARTESIAN_POINT ( 'NONE',  ( -110.8997504895301063, -282.5497265266225213, -289.4702356246036743 ) ) ;
#43327 = CARTESIAN_POINT ( 'NONE',  ( 5.953282685238336924, -283.8771274236851241, -329.8667427487080204 ) ) ;
#43328 = CARTESIAN_POINT ( 'NONE',  ( -104.2568765402012048, -284.9577844238124840, -299.9408558479933049 ) ) ;
#43329 = EDGE_CURVE ( 'NONE', #8082, #63051, #11152, .T. ) ;
#43330 = CARTESIAN_POINT ( 'NONE',  ( -96.19511238494023075, -293.1761275810710572, -223.3007028383269983 ) ) ;
#43331 = CARTESIAN_POINT ( 'NONE',  ( -5.126979291058860966, -274.7979943101187814, -200.4471991034898792 ) ) ;
#43332 = CARTESIAN_POINT ( 'NONE',  ( -88.53417205081933616, -287.8433325724970473, -325.9366972801727229 ) ) ;
#43333 = CARTESIAN_POINT ( 'NONE',  ( -82.54628190410252842, -277.6509575971571167, -332.6952642144208880 ) ) ;
#43334 = CARTESIAN_POINT ( 'NONE',  ( 29.88666486062728822, -295.9627297293893662, -302.9179393708922134 ) ) ;
#43335 = CARTESIAN_POINT ( 'NONE',  ( -48.18343439339133738, -275.2947406849379490, -436.6688341897501573 ) ) ;
#43336 = CARTESIAN_POINT ( 'NONE',  ( 208.6466510127238507, 37.28161665985707884, 12.02378101520594100 ) ) ;
#43337 = CARTESIAN_POINT ( 'NONE',  ( -103.4636256423404319, -282.8042152529550890, -302.5581743686024652 ) ) ;
#43338 = CARTESIAN_POINT ( 'NONE',  ( -45.04201984405015935, -277.9546122620739652, -195.7058468397716240 ) ) ;
#43339 = CARTESIAN_POINT ( 'NONE',  ( -76.06404202801982706, -272.0249580168496095, -204.5483572420409644 ) ) ;
#43340 = CARTESIAN_POINT ( 'NONE',  ( 18.38073660658709585, -275.5726126801830560, -317.6781626157851974 ) ) ;
#43341 = CARTESIAN_POINT ( 'NONE',  ( 35.39518030445368879, -294.9166019605768270, -258.4478949576399600 ) ) ;
#43342 = CARTESIAN_POINT ( 'NONE',  ( -9.649584533061148051, -293.3641616281943243, -202.5092646401708407 ) ) ;
#43343 = CARTESIAN_POINT ( 'NONE',  ( 38.94805206123166386, -294.7948292798829470, -264.6016056227712738 ) ) ;
#43344 = CARTESIAN_POINT ( 'NONE',  ( -108.4765597226606531, -296.6017643412727125, -253.9650283572826766 ) ) ;
#43345 = CARTESIAN_POINT ( 'NONE',  ( -40.00409389572237728, -291.0856444169626229, -345.3647856263623339 ) ) ;
#43346 = CARTESIAN_POINT ( 'NONE',  ( -30.21277951589942035, -283.1309896249060785, -347.0303979805375434 ) ) ;
#43347 = CARTESIAN_POINT ( 'NONE',  ( 8.777517695267203379, -272.8165299731578557, -210.2501936411803456 ) ) ;
#43348 = CARTESIAN_POINT ( 'NONE',  ( 38.10786404863083732, -287.5777474754362402, -285.7352283656842928 ) ) ;
#43349 = CARTESIAN_POINT ( 'NONE',  ( -96.56291439218715311, -279.9068103850914326, -315.8000284812546852 ) ) ;
#43350 = EDGE_CURVE ( 'NONE', #50260, #33465, #17182, .T. ) ;
#43351 = CARTESIAN_POINT ( 'NONE',  ( -22.40015596388471764, -285.3067938223641136, -198.6141681104379302 ) ) ;
#43352 = CARTESIAN_POINT ( 'NONE',  ( -104.7280414750854192, -288.1165675280980736, -303.4046435690154340 ) ) ;
#43353 = CARTESIAN_POINT ( 'NONE',  ( -115.8664652629750549, -267.0802710791712116, -295.7299871733738996 ) ) ;
#43354 = CARTESIAN_POINT ( 'NONE',  ( -108.7815577518589265, -283.8572520999057360, -285.7285719363633234 ) ) ;
#43355 = CARTESIAN_POINT ( 'NONE',  ( 24.26322914733271929, -282.1490045742972370, -224.8326498721849021 ) ) ;
#43356 = CARTESIAN_POINT ( 'NONE',  ( -107.5211435740363868, -289.2112476431066170, -301.5992326614872354 ) ) ;
#43357 = CARTESIAN_POINT ( 'NONE',  ( -45.21123133330947752, -281.5543207393445186, -194.5161261155256796 ) ) ;
#43358 = CARTESIAN_POINT ( 'NONE',  ( -61.90525397699875754, -281.0547061122641708, -197.8488397926061850 ) ) ;
#43359 = CARTESIAN_POINT ( 'NONE',  ( -34.31120346350135719, -279.9245943571611406, -197.4115050792045736 ) ) ;
#43360 = CARTESIAN_POINT ( 'NONE',  ( -8.354870553190677285, -276.4132869994372186, -201.5192985566135917 ) ) ;
#43361 = CARTESIAN_POINT ( 'NONE',  ( 39.50214713631897467, -293.6231637474240301, -276.0391462781040559 ) ) ;
#43362 = CARTESIAN_POINT ( 'NONE',  ( -40.04234839696056270, -287.1062376042696656, -345.0077492016332599 ) ) ;
#43363 = CARTESIAN_POINT ( 'NONE',  ( -40.61862575140684584, -293.6117397404952385, -194.2185636389559136 ) ) ;
#43364 = CARTESIAN_POINT ( 'NONE',  ( -96.66662287155928368, -294.8720686276568017, -313.4497018574463141 ) ) ;
#43365 = CARTESIAN_POINT ( 'NONE',  ( -37.51988987875960646, -284.9745879434625522, -344.8135828466392923 ) ) ;
#43366 = CARTESIAN_POINT ( 'NONE',  ( -55.81275597118737863, -294.9631699522789745, -341.0598731621005300 ) ) ;
#43367 = CARTESIAN_POINT ( 'NONE',  ( -86.32620317555371514, -292.4705895245837155, -211.2835870222715187 ) ) ;
#43368 = CARTESIAN_POINT ( 'NONE',  ( 33.20978049366844687, -281.9504969847442908, -251.1721590282433567 ) ) ;
#43369 = CARTESIAN_POINT ( 'NONE',  ( -107.8566035761110129, -272.0000889936525823, -239.8875109574228759 ) ) ;
#43370 = CARTESIAN_POINT ( 'NONE',  ( -69.30735587525889230, -290.1131813351529445, -340.3148499007525629 ) ) ;
#43371 = CARTESIAN_POINT ( 'NONE',  ( -37.33847804324527431, -281.1916664934377650, -346.1387768952744750 ) ) ;
#43372 = CARTESIAN_POINT ( 'NONE',  ( -99.19013785467485889, -291.4951141064793774, -224.5076586840816617 ) ) ;
#43373 = CARTESIAN_POINT ( 'NONE',  ( 19.52898507467300249, -287.2378303648362703, -224.5394234360309724 ) ) ;
#43374 = DIRECTION ( 'NONE',  ( -0.000000000000000000, 1.000000000000000000, 0.000000000000000000 ) ) ;
#43375 = CARTESIAN_POINT ( 'NONE',  ( -78.93342798129256721, -207.3472289075424726, -354.9948781244794986 ) ) ;
#43376 = CARTESIAN_POINT ( 'NONE',  ( -62.72819003750708333, -182.7653398274297842, -358.6004343349099486 ) ) ;
#43377 = CARTESIAN_POINT ( 'NONE',  ( -99.31730995789541794, -277.2124897904703289, -309.3353976584218117 ) ) ;
#43378 = CARTESIAN_POINT ( 'NONE',  ( -81.46300260621561051, -278.3565017537416111, -211.7522160558771986 ) ) ;
#43379 = CARTESIAN_POINT ( 'NONE',  ( -38.35287593860172706, -273.7065218918179994, -193.3889034170015861 ) ) ;
#43380 = CARTESIAN_POINT ( 'NONE',  ( -87.43554566246351101, -230.9673987827994210, -345.9252775359201451 ) ) ;
#43381 = CARTESIAN_POINT ( 'NONE',  ( -99.75712166490203003, -277.7146594378781970, -226.2825353398110906 ) ) ;
#43382 = CARTESIAN_POINT ( 'NONE',  ( -40.32477459187423108, -281.1099505302134958, -344.9462912529492087 ) ) ;
#43383 = CARTESIAN_POINT ( 'NONE',  ( -110.2368565160181078, -298.0390585385410418, -291.8608737959810924 ) ) ;
#43384 = CARTESIAN_POINT ( 'NONE',  ( -0.06494025528746319442, -293.0551079096751437, -207.5245711721255759 ) ) ;
#43385 = CARTESIAN_POINT ( 'NONE',  ( -13.14117805953388007, -287.4158688506900035, -339.7554852554226841 ) ) ;
#43386 = CARTESIAN_POINT ( 'NONE',  ( -32.69705956757077558, -274.7606237578257833, -193.5903134513877148 ) ) ;
#43387 = CARTESIAN_POINT ( 'NONE',  ( -92.01815984315234687, -273.2432029712903727, -221.9928974961060817 ) ) ;
#43388 = ORIENTED_EDGE ( 'NONE', *, *, #77420, .F. ) ;
#43389 = DIRECTION ( 'NONE',  ( 0.000000000000000000, 1.000000000000000000, 0.000000000000000000 ) ) ;
#43390 = DIRECTION ( 'NONE',  ( -1.000000000000000000, 0.000000000000000000, 0.000000000000000000 ) ) ;
#43391 = CARTESIAN_POINT ( 'NONE',  ( -102.1885730148448630, -280.9888025511481828, -231.4753474475529913 ) ) ;
#43392 = CARTESIAN_POINT ( 'NONE',  ( -16.84842264494902508, -281.4028238013963232, -199.9746729037055104 ) ) ;
#43393 = CARTESIAN_POINT ( 'NONE',  ( -22.78258808288043369, -281.9959965722508173, -195.7287196729666050 ) ) ;
#43394 = CARTESIAN_POINT ( 'NONE',  ( -61.62400858236756562, -282.4341501583178342, -339.5070612325035313 ) ) ;
#43395 = CARTESIAN_POINT ( 'NONE',  ( -98.65590310181080724, -279.8399778066235513, -312.2112553115475180 ) ) ;
#43396 = CARTESIAN_POINT ( 'NONE',  ( -16.42551273587970684, -272.8071510119688696, -199.6451780863918657 ) ) ;
#43397 = LINE ( 'NONE', #28739, #92650 ) ;
#43398 = CARTESIAN_POINT ( 'NONE',  ( 200.2349812190172713, 66.43136063442170780, -7.741079165001072404 ) ) ;
#43399 = CARTESIAN_POINT ( 'NONE',  ( 34.56703283253786196, -276.0116629786900262, -243.2817357121049042 ) ) ;
#43400 = CARTESIAN_POINT ( 'NONE',  ( 199.0061125298537377, 275.0000000000000568, -7.725424859374024678 ) ) ;
#43401 = CARTESIAN_POINT ( 'NONE',  ( 23.68432002420183835, -276.9591021982989218, -226.7406999239534571 ) ) ;
#43402 = CARTESIAN_POINT ( 'NONE',  ( -54.02045038036295210, -275.8368251194293066, -344.9836039973096717 ) ) ;
#43403 = VERTEX_POINT ( 'NONE', #43893 ) ;
#43404 = CARTESIAN_POINT ( 'NONE',  ( 189.9243309297870610, 275.0000000000000568, 20.22542485937349355 ) ) ;
#43405 = CARTESIAN_POINT ( 'NONE',  ( -105.5068348888408281, -286.1115707025226129, -302.4846483425838528 ) ) ;
#43406 = EDGE_CURVE ( 'NONE', #56036, #68290, #41351, .T. ) ;
#43407 = CARTESIAN_POINT ( 'NONE',  ( 13.02170408912212274, -291.9749491666452741, -217.2939036000848887 ) ) ;
#43408 = CARTESIAN_POINT ( 'NONE',  ( -10.02240465606981523, -285.7481026732858140, -198.4227586823534466 ) ) ;
#43409 = CARTESIAN_POINT ( 'NONE',  ( -91.49800515898722608, -282.0765132019558337, -320.8097912973016719 ) ) ;
#43411 = CARTESIAN_POINT ( 'NONE',  ( 18.87950669965240280, -284.9499527188662569, -221.5708515069829616 ) ) ;
#43410 = CARTESIAN_POINT ( 'NONE',  ( -99.53868827011000064, -282.5866061869135706, -309.7873220949351207 ) ) ;
#43412 = CARTESIAN_POINT ( 'NONE',  ( -48.37330104161164712, -284.4007774608808745, -342.9244302366724924 ) ) ;
#43413 = CARTESIAN_POINT ( 'NONE',  ( -65.45331386515763938, -271.6845087390630056, -200.8150391709323799 ) ) ;
#43414 = CARTESIAN_POINT ( 'NONE',  ( -99.15163841191592553, -282.3539584491877577, -315.0135724021374699 ) ) ;
#43415 = CARTESIAN_POINT ( 'NONE',  ( -111.2289657237812435, -298.3832841288626696, -283.5254160638536973 ) ) ;
#43416 = CARTESIAN_POINT ( 'NONE',  ( -62.56175086624408976, -283.7245651211972586, -199.5516732280953534 ) ) ;
#43417 = CARTESIAN_POINT ( 'NONE',  ( -109.3656735607848987, -279.6678302470750737, -257.0962885614056290 ) ) ;
#43418 = CARTESIAN_POINT ( 'NONE',  ( 37.74472285456480591, -289.4951776745472785, -265.9011675192144253 ) ) ;
#43419 = CARTESIAN_POINT ( 'NONE',  ( 195.5690041525305105, 26.62290662055165669, 13.81123227693192135 ) ) ;
#43420 = FACE_BOUND ( 'NONE', #81899, .T. ) ;
#43421 = CARTESIAN_POINT ( 'NONE',  ( 18.48263136099120274, -296.1784363810049854, -321.3584557497873107 ) ) ;
#43422 = CARTESIAN_POINT ( 'NONE',  ( -88.47725723244910512, -275.7689532948882629, -325.2260015257643886 ) ) ;
#43423 = CARTESIAN_POINT ( 'NONE',  ( -99.74511591218792717, -289.1535987420851370, -315.2163816133560772 ) ) ;
#43424 = CARTESIAN_POINT ( 'NONE',  ( -28.82365413389263864, -293.3423726761366197, -343.7194648805318593 ) ) ;
#43425 = CARTESIAN_POINT ( 'NONE',  ( -106.9061215607682271, -277.5517736839869940, -246.4976734086177999 ) ) ;
#43426 = CARTESIAN_POINT ( 'NONE',  ( -93.08048571575984909, -271.3233591039005432, -221.0204453008902590 ) ) ;
#43427 = CARTESIAN_POINT ( 'NONE',  ( -17.31418827951640793, -293.6311327765207579, -199.5964903536095392 ) ) ;
#43428 = CARTESIAN_POINT ( 'NONE',  ( -54.49178911615188525, -282.3376638359844719, -195.3683826091709363 ) ) ;
#43429 = CARTESIAN_POINT ( 'NONE',  ( 20.82645875388856282, -292.7038562863409652, -319.7491028241295794 ) ) ;
#43430 = CARTESIAN_POINT ( 'NONE',  ( -64.09207112628276093, -291.0070040632829205, -339.1971234759729441 ) ) ;
#43431 = CARTESIAN_POINT ( 'NONE',  ( -97.37302182073817391, -288.1616190127863888, -316.9466783307221931 ) ) ;
#43432 = CARTESIAN_POINT ( 'NONE',  ( 29.97132445528106359, -289.3759147627188213, -300.2253297965915522 ) ) ;
#43433 = DIRECTION ( 'NONE',  ( -0.000000000000000000, -0.000000000000000000, 1.000000000000000000 ) ) ;
#43434 = CARTESIAN_POINT ( 'NONE',  ( -75.94528405702773455, -290.3850811402107297, -332.5090466261805773 ) ) ;
#43435 = EDGE_CURVE ( 'NONE', #93199, #38700, #77682, .T. ) ;
#43436 = CARTESIAN_POINT ( 'NONE',  ( 209.1374487190023501, 30.94653725228601715, 12.00000000000000000 ) ) ;
#43437 = CARTESIAN_POINT ( 'NONE',  ( -5.776024410489380756, -289.8513142760285177, -340.1580866586363072 ) ) ;
#43438 = CARTESIAN_POINT ( 'NONE',  ( -47.86363211020864128, -277.9392164427554803, -195.6914320520579338 ) ) ;
#43439 = CARTESIAN_POINT ( 'NONE',  ( -67.35812943433514022, -280.0023844680056300, -199.4755886886987355 ) ) ;
#43440 = CARTESIAN_POINT ( 'NONE',  ( 26.70193986459174695, -281.7812112698554756, -313.0712627727609174 ) ) ;
#43441 = CARTESIAN_POINT ( 'NONE',  ( 12.48118591435941482, -284.7456518849382974, -214.2317021613211807 ) ) ;
#43442 = CARTESIAN_POINT ( 'NONE',  ( 196.0351550650565002, 41.34106363718652233, 11.96389409883856381 ) ) ;
#43443 = CARTESIAN_POINT ( 'NONE',  ( -5.524678771183688220, -280.7687758078539559, -337.4462752216025478 ) ) ;
#43444 = CARTESIAN_POINT ( 'NONE',  ( -110.5777956472695536, -282.3443717226074341, -286.5313055646341809 ) ) ;
#43445 = CARTESIAN_POINT ( 'NONE',  ( 156.4851178187871312, 15.00000000000000000, 7.000000000000000888 ) ) ;
#43446 = CARTESIAN_POINT ( 'NONE',  ( -99.10011729990263518, -276.4317910522534589, -315.2008141437713107 ) ) ;
#43447 = CARTESIAN_POINT ( 'NONE',  ( -105.1523238591232428, -283.9381583100451394, -234.4255049019193962 ) ) ;
#43448 = CARTESIAN_POINT ( 'NONE',  ( 9.104247122874012277, -299.5888637825325418, -197.1181713360114713 ) ) ;
#43449 = CARTESIAN_POINT ( 'NONE',  ( -107.3364329621977049, -292.4595799038322070, -246.9692862814247860 ) ) ;
#43450 = CARTESIAN_POINT ( 'NONE',  ( -44.00956919143204971, -275.3948251415978348, -194.1889303908548072 ) ) ;
#43451 = CARTESIAN_POINT ( 'NONE',  ( 35.12652270509740760, -275.3424674864635335, -279.7332566004096179 ) ) ;
#43452 = CARTESIAN_POINT ( 'NONE',  ( -87.81770607290447117, -297.7577978263153113, -325.8333945734870554 ) ) ;
#43453 = CARTESIAN_POINT ( 'NONE',  ( 5.559083387748535721, -288.6550865633099647, -334.3026755036227655 ) ) ;
#43454 = CARTESIAN_POINT ( 'NONE',  ( 37.97827302712818209, -279.5553000099262704, -264.3431582021373174 ) ) ;
#43455 = CARTESIAN_POINT ( 'NONE',  ( -4.602216920455489912, -292.3049943157915891, -200.6680319278289915 ) ) ;
#43456 = EDGE_CURVE ( 'NONE', #34721, #92061, #57163, .T. ) ;
#43457 = CARTESIAN_POINT ( 'NONE',  ( -109.5065327083319744, -289.7787481143462287, -257.5960518501238425 ) ) ;
#43458 = CARTESIAN_POINT ( 'NONE',  ( -17.07252644415595810, -292.7904386113723945, -342.6240595373823226 ) ) ;
#43459 = EDGE_LOOP ( 'NONE', ( #7706, #69578 ) ) ;
#43460 = CARTESIAN_POINT ( 'NONE',  ( 152.9410204041312795, 20.82809642979767872, 8.928152258827880772 ) ) ;
#43461 = CARTESIAN_POINT ( 'NONE',  ( 30.88809663704017439, -292.7111455752344114, -244.2329095684307276 ) ) ;
#43462 = FACE_OUTER_BOUND ( 'NONE', #49691, .T. ) ;
#43463 = CARTESIAN_POINT ( 'NONE',  ( -3.603613472001642393, -287.4277866820104350, -201.3933057632786472 ) ) ;
#43464 = CARTESIAN_POINT ( 'NONE',  ( -92.08974858914540107, -275.4094976428775681, -313.9805196606274080 ) ) ;
#43465 = CARTESIAN_POINT ( 'NONE',  ( -56.02465264753779195, -294.3458410997327519, -344.8175985429817842 ) ) ;
#43466 = CARTESIAN_POINT ( 'NONE',  ( -97.20506964720831888, -286.5092331376041557, -222.7200090002236266 ) ) ;
#43467 = CARTESIAN_POINT ( 'NONE',  ( -109.6119255445987193, -284.5212970642943446, -260.0647825785431451 ) ) ;
#43468 = CARTESIAN_POINT ( 'NONE',  ( 32.71494593002077522, -276.7697930191113755, -247.3328422661348043 ) ) ;
#43469 = CARTESIAN_POINT ( 'NONE',  ( 0.04449511879383971635, -292.5724611573358516, -335.0275253664256638 ) ) ;
#43470 = CARTESIAN_POINT ( 'NONE',  ( 34.43417773083176314, -295.5473916441992515, -288.4220529946449005 ) ) ;
#43471 = CARTESIAN_POINT ( 'NONE',  ( -26.98054600509038181, -275.7123912716060659, -343.0231919231287634 ) ) ;
#43472 = EDGE_LOOP ( 'NONE', ( #55575, #68637, #35121, #53128, #16688 ) ) ;
#43473 = CARTESIAN_POINT ( 'NONE',  ( 195.0026807809657612, 40.76696999206299665, 13.61341101255641206 ) ) ;
#43474 = CARTESIAN_POINT ( 'NONE',  ( -50.46809359016861407, -294.8819516350542926, -346.2664960106724266 ) ) ;
#43475 = CARTESIAN_POINT ( 'NONE',  ( 33.69501238127471510, -289.7635006161941646, -292.7836949668480315 ) ) ;
#43476 = CARTESIAN_POINT ( 'NONE',  ( 2.197429475817664013, -229.5268262511776527, 25.50000000000000000 ) ) ;
#43477 = CARTESIAN_POINT ( 'NONE',  ( -48.93688340976666495, -298.9875598468339035, -194.4984038835194156 ) ) ;
#43478 = EDGE_CURVE ( 'NONE', #72750, #1023, #40164, .T. ) ;
#43479 = CARTESIAN_POINT ( 'NONE',  ( -14.54207697897043872, -287.0069175899264451, -200.8525035688566902 ) ) ;
#43480 = EDGE_LOOP ( 'NONE', ( #69013, #5333, #30300, #12459, #29563, #5575 ) ) ;
#43481 = CARTESIAN_POINT ( 'NONE',  ( -99.23104185823777357, -278.2161651401011682, -224.9238565318159431 ) ) ;
#43482 = CARTESIAN_POINT ( 'NONE',  ( -0.7473656586055850148, -295.2306030980432183, -338.0085760740752789 ) ) ;
#43483 = CARTESIAN_POINT ( 'NONE',  ( -10.03103973441768026, -286.8389096837565830, -341.0324226925332027 ) ) ;
#43484 = CARTESIAN_POINT ( 'NONE',  ( -88.58819105861471144, -296.0809220854289379, -327.8742298937423243 ) ) ;
#43485 = CARTESIAN_POINT ( 'NONE',  ( 35.31591808069838834, -293.7830228634124410, -262.5954492359664414 ) ) ;
#43486 = CARTESIAN_POINT ( 'NONE',  ( 165.2494399300530290, 8.542400036368780647, 25.74970488511327815 ) ) ;
#43487 = DIRECTION ( 'NONE',  ( -0.000000000000000000, 1.000000000000000000, -0.000000000000000000 ) ) ;
#43488 = CARTESIAN_POINT ( 'NONE',  ( -82.08642841125383427, -219.1949203529638623, -349.1242040296363598 ) ) ;
#43489 = CARTESIAN_POINT ( 'NONE',  ( -35.18738530977717005, -287.5988232182348270, -194.0718402913028910 ) ) ;
#43490 = CARTESIAN_POINT ( 'NONE',  ( -88.52914483777347243, -293.1952119285919025, -334.4957818155094174 ) ) ;
#43491 = ORIENTED_EDGE ( 'NONE', *, *, #37797, .F. ) ;
#43492 = CARTESIAN_POINT ( 'NONE',  ( -107.3229105242246106, -278.3101404745816012, -238.3590844367061266 ) ) ;
#43493 = CARTESIAN_POINT ( 'NONE',  ( -56.77095638343554640, -285.3034222921888841, -342.6282088674892066 ) ) ;
#43494 = CARTESIAN_POINT ( 'NONE',  ( -70.79178560055378000, -284.1942628544149443, -201.6610591947422222 ) ) ;
#43495 = CARTESIAN_POINT ( 'NONE',  ( -5.192225229086207428, -286.7055107458209591, -337.5007148370161758 ) ) ;
#43496 = CARTESIAN_POINT ( 'NONE',  ( -8.335256994194917723, -278.5368422520412537, -340.3675447722445142 ) ) ;
#43497 = CARTESIAN_POINT ( 'NONE',  ( -72.88229652963883609, -298.0599882713836450, -206.5265313608019540 ) ) ;
#43498 = ORIENTED_EDGE ( 'NONE', *, *, #32642, .F. ) ;
#43499 = CARTESIAN_POINT ( 'NONE',  ( 34.25204703431068509, -292.4551521410048736, -287.0170711653544231 ) ) ;
#43501 = CARTESIAN_POINT ( 'NONE',  ( -81.34262857331447094, -278.7846910316441154, -211.9211021829239030 ) ) ;
#43500 = CARTESIAN_POINT ( 'NONE',  ( -104.2713891148673895, -278.1587637744920016, -299.6325371492179670 ) ) ;
#43502 = CARTESIAN_POINT ( 'NONE',  ( 38.42008636018527312, -276.4813143978914809, -258.3751275733171155 ) ) ;
#43503 = CARTESIAN_POINT ( 'NONE',  ( -45.62993176495204750, -276.0750550011469500, -346.6556697337338164 ) ) ;
#43504 = CARTESIAN_POINT ( 'NONE',  ( -23.51153694099567915, -107.8100564029413704, -360.1567311266264824 ) ) ;
#43505 = CARTESIAN_POINT ( 'NONE',  ( -108.8794380750494213, -297.6334543093705634, -297.3609688603785344 ) ) ;
#43506 = CARTESIAN_POINT ( 'NONE',  ( -37.37352853689063892, -276.5519495502701943, -195.3611179825600175 ) ) ;
#43507 = VERTEX_POINT ( 'NONE', #10703 ) ;
#43508 = CARTESIAN_POINT ( 'NONE',  ( -147.8070425842518034, -211.3363389866113664, 22.50000000000000000 ) ) ;
#43509 = CARTESIAN_POINT ( 'NONE',  ( -38.64413161842912814, -287.1151491696821836, -197.0510410699282886 ) ) ;
#43510 = CARTESIAN_POINT ( 'NONE',  ( -10.37482758168705388, -288.1592681364655846, -199.2645073152849875 ) ) ;
#43511 = CARTESIAN_POINT ( 'NONE',  ( -31.87199579458728493, -288.3300365010234714, -343.3088282413960997 ) ) ;
#43512 = CARTESIAN_POINT ( 'NONE',  ( -44.41980399959960835, -282.6469378582092986, -347.0266209547609151 ) ) ;
#43513 = CARTESIAN_POINT ( 'NONE',  ( -105.1694075032272764, -277.3384911008652125, -241.2777460070076643 ) ) ;
#43514 = CARTESIAN_POINT ( 'NONE',  ( -111.6262676631040165, -286.4050373414812043, -270.9422197182587411 ) ) ;
#43515 = CARTESIAN_POINT ( 'NONE',  ( -57.28240059536676654, -278.2699859010681962, -199.4169412261406649 ) ) ;
#43516 = CARTESIAN_POINT ( 'NONE',  ( -89.42355889430436378, -279.1195276500897648, -322.2862689286160389 ) ) ;
#43517 = CARTESIAN_POINT ( 'NONE',  ( 11.58308369440831953, -275.2450472520770859, -216.0311002410117283 ) ) ;
#43518 = CARTESIAN_POINT ( 'NONE',  ( -51.62638300111430567, -288.0259101326500968, -345.6203802214030816 ) ) ;
#43519 = CARTESIAN_POINT ( 'NONE',  ( -5.513057092220508437, -283.4468357167801287, -340.2974912342566540 ) ) ;
#43520 = CARTESIAN_POINT ( 'NONE',  ( -47.24222819239442117, -283.6670915203624190, -346.6599151367047966 ) ) ;
#43521 = EDGE_LOOP ( 'NONE', ( #93558, #21920 ) ) ;
#43522 = ORIENTED_EDGE ( 'NONE', *, *, #54191, .T. ) ;
#43523 = DIRECTION ( 'NONE',  ( 0.000000000000000000, 0.000000000000000000, -1.000000000000000000 ) ) ;
#43524 = CARTESIAN_POINT ( 'NONE',  ( -29.08781290339920389, -290.8091620183986947, -345.7276551782750289 ) ) ;
#43525 = CARTESIAN_POINT ( 'NONE',  ( -101.8942289069071734, -288.6941554437736386, -311.5228501339166201 ) ) ;
#43526 = EDGE_CURVE ( 'NONE', #47679, #42209, #72901, .T. ) ;
#43527 = CARTESIAN_POINT ( 'NONE',  ( -59.53557361278180338, -272.8164568751031425, -200.5166226242758398 ) ) ;
#43528 = CARTESIAN_POINT ( 'NONE',  ( 39.60962277385706187, -292.9002039593197537, -270.3183063866856628 ) ) ;
#43529 = CARTESIAN_POINT ( 'NONE',  ( -58.91037137977332350, -287.8160346317469021, -340.8807337726425999 ) ) ;
#43530 = CARTESIAN_POINT ( 'NONE',  ( 0.4454132180781383843, -290.8029828628548898, -206.7206585370008156 ) ) ;
#43531 = CARTESIAN_POINT ( 'NONE',  ( 26.04667951827650185, -289.2635271134293475, -307.4622218789428985 ) ) ;
#43532 = CARTESIAN_POINT ( 'NONE',  ( 21.31550574532285580, -290.6948066931273615, -317.0979686699210447 ) ) ;
#43533 = CARTESIAN_POINT ( 'NONE',  ( 19.97742372891767815, -290.2212647443581091, -318.7296893090459093 ) ) ;
#43534 = CARTESIAN_POINT ( 'NONE',  ( -58.40006995558686498, -289.7803841335240804, -198.2045279563109830 ) ) ;
#43535 = CARTESIAN_POINT ( 'NONE',  ( -76.66686770079212465, -293.5264245113584138, -206.4381724166781567 ) ) ;
#43536 = CARTESIAN_POINT ( 'NONE',  ( -108.3183126739273661, -285.2559594128039180, -288.4090796484070438 ) ) ;
#43537 = CARTESIAN_POINT ( 'NONE',  ( -47.52094747803085539, -293.9233500542866864, -195.8343694083687296 ) ) ;
#43538 = CARTESIAN_POINT ( 'NONE',  ( -113.3425974752031493, -270.8076308035728061, -270.3389060467516174 ) ) ;
#43539 = CARTESIAN_POINT ( 'NONE',  ( -15.35796352212545912, -300.2454598573677345, -194.7939833255516078 ) ) ;
#43540 = CARTESIAN_POINT ( 'NONE',  ( 35.84916290400889238, -280.7260000434499716, -268.5898457665853130 ) ) ;
#43541 = CARTESIAN_POINT ( 'NONE',  ( -84.05991212271342761, -281.6935959886387195, -329.0998267559237433 ) ) ;
#43542 = CARTESIAN_POINT ( 'NONE',  ( -50.45005498846544612, -294.4124758169335792, -346.1271020356829240 ) ) ;
#43543 = CARTESIAN_POINT ( 'NONE',  ( 22.31101732609832666, -273.1866000526096627, -226.5487074624397792 ) ) ;
#43544 = CARTESIAN_POINT ( 'NONE',  ( -111.7905492138154671, -276.6646643336296165, -267.8354834178849728 ) ) ;
#43545 = CARTESIAN_POINT ( 'NONE',  ( -68.27022746863505631, -298.9523956380553500, -203.6790041995958518 ) ) ;
#43546 = CARTESIAN_POINT ( 'NONE',  ( -34.10981224036434156, -272.6667863161680430, -194.0187235045170553 ) ) ;
#43547 = CARTESIAN_POINT ( 'NONE',  ( 34.52131233576097458, -294.7693090364884370, -254.4573361343793181 ) ) ;
#43548 = CARTESIAN_POINT ( 'NONE',  ( -83.63170945779074827, -296.0521521680024080, -521.1711561948568487 ) ) ;
#43549 = CARTESIAN_POINT ( 'NONE',  ( 19.82633579470533647, -294.9986640864898959, -316.0365131792631814 ) ) ;
#43550 = CARTESIAN_POINT ( 'NONE',  ( 200.7065524281625812, 64.16053070461664731, 8.800381594953616826 ) ) ;
#43552 = CARTESIAN_POINT ( 'NONE',  ( -103.9366167652389095, -296.1478869058889813, -300.3864741894257691 ) ) ;
#43551 = CARTESIAN_POINT ( 'NONE',  ( -29.60616973671221785, -284.1697682403773797, -195.4040077689209056 ) ) ;
#43553 = CARTESIAN_POINT ( 'NONE',  ( -109.0284809337596101, -284.9100685495209859, -242.1090782600143427 ) ) ;
#43554 = CARTESIAN_POINT ( 'NONE',  ( 23.84721203567875847, -286.5957326044330671, -223.6312468062063203 ) ) ;
#43555 = CARTESIAN_POINT ( 'NONE',  ( 0.8664747166047355176, -290.5630023237768569, -206.0170133456105930 ) ) ;
#43556 = CARTESIAN_POINT ( 'NONE',  ( -101.7502699662694994, -278.3018715467194397, -228.3638444514133141 ) ) ;
#43557 = CARTESIAN_POINT ( 'NONE',  ( 10.64812456238590599, -278.1952119285918457, -210.2361428286349394 ) ) ;
#43558 = FACE_OUTER_BOUND ( 'NONE', #15507, .T. ) ;
#43559 = CARTESIAN_POINT ( 'NONE',  ( 35.95014289420876707, -286.2842879673328866, -265.5760246650050362 ) ) ;
#43561 = DIRECTION ( 'NONE',  ( 0.000000000000000000, 0.000000000000000000, 1.000000000000000000 ) ) ;
#43560 = CARTESIAN_POINT ( 'NONE',  ( -82.68101052597201317, -288.5761969922439789, -332.2144884773866238 ) ) ;
#43562 = DIRECTION ( 'NONE',  ( -0.4999999999999951705, -0.8660254037844413721, 0.000000000000000000 ) ) ;
#43563 = CARTESIAN_POINT ( 'NONE',  ( -100.8445759073984647, -297.6400093711162071, -308.0625622008096229 ) ) ;
#43564 = CARTESIAN_POINT ( 'NONE',  ( -56.42716089895206721, -281.2362843987488645, -196.3176743493169738 ) ) ;
#43566 = CARTESIAN_POINT ( 'NONE',  ( 31.99802314604900744, -280.9131540185737208, -247.3087051468501443 ) ) ;
#43565 = CARTESIAN_POINT ( 'NONE',  ( -104.5034437540514887, -294.1213101860024040, -304.6478662851592958 ) ) ;
#43567 = CARTESIAN_POINT ( 'NONE',  ( 1.771263359367746260, -294.7107183991899433, -336.6874030566929150 ) ) ;
#43568 = CARTESIAN_POINT ( 'NONE',  ( 11.17209960989293727, -284.7974003236965359, -212.3642015460783625 ) ) ;
#43569 = CARTESIAN_POINT ( 'NONE',  ( -70.37720994900570304, -281.6168532604185089, -203.0286908453328749 ) ) ;
#43570 = CARTESIAN_POINT ( 'NONE',  ( -106.9266027588686683, -295.9148765568199337, -247.3673440217181962 ) ) ;
#43571 = ORIENTED_EDGE ( 'NONE', *, *, #52823, .F. ) ;
#43572 = LINE ( 'NONE', #35559, #61973 ) ;
#43573 = CARTESIAN_POINT ( 'NONE',  ( -83.79914694217985982, -285.6730082613418062, -328.8530403068154442 ) ) ;
#43574 = DIRECTION ( 'NONE',  ( 1.000000000000000000, 0.000000000000000000, 0.000000000000000000 ) ) ;
#43575 = CARTESIAN_POINT ( 'NONE',  ( -37.30987171927208834, -289.5523547857347353, -195.3611179825600175 ) ) ;
#43576 = CARTESIAN_POINT ( 'NONE',  ( 8.137242795908855797, -275.6453080563344429, -332.3610216312295620 ) ) ;
#43577 = CARTESIAN_POINT ( 'NONE',  ( -107.7513244488335573, -290.6401191635279702, -251.0871768305287901 ) ) ;
#43578 = CARTESIAN_POINT ( 'NONE',  ( 26.16627646168965882, -283.5820830503559478, -307.8444095038620958 ) ) ;
#43579 = CARTESIAN_POINT ( 'NONE',  ( -49.02192600409640022, -275.5011472350892632, -197.4395479601549539 ) ) ;
#43580 = CARTESIAN_POINT ( 'NONE',  ( 8.741356655557691369, -284.0322707069191779, -331.0471319471915308 ) ) ;
#43581 = CARTESIAN_POINT ( 'NONE',  ( 20.48437603630994275, -280.9807989981646301, -315.5637221284270026 ) ) ;
#43582 = CARTESIAN_POINT ( 'NONE',  ( -108.3462206651810789, -280.8665737772173543, -246.0486506677223701 ) ) ;
#43583 = CARTESIAN_POINT ( 'NONE',  ( -108.0783415563494714, -273.1078427050683217, -239.8070697769145454 ) ) ;
#43584 = CARTESIAN_POINT ( 'NONE',  ( 16.02856474352110183, -274.6173854097442586, -214.8578313048464281 ) ) ;
#43585 = CARTESIAN_POINT ( 'NONE',  ( 31.17170886458801959, -295.0875115833463269, -241.1221824460717755 ) ) ;
#43586 = CARTESIAN_POINT ( 'NONE',  ( 210.3152560301384142, 38.32590481451375553, 9.000000000000001776 ) ) ;
#43587 = EDGE_CURVE ( 'NONE', #52690, #29052, #26232, .T. ) ;
#43588 = CARTESIAN_POINT ( 'NONE',  ( 139.6925840978351516, -43.55766379199612004, 21.50000000000000000 ) ) ;
#43589 = CARTESIAN_POINT ( 'NONE',  ( -2.556030035352807150, -292.7365998118771131, -337.6683437417710252 ) ) ;
#43590 = AXIS2_PLACEMENT_3D ( 'NONE', #42173, #28466, #36029 ) ;
#43591 = CARTESIAN_POINT ( 'NONE',  ( -6.497303379122718603, -273.9761888997055053, -204.1296176895979784 ) ) ;
#43592 = CARTESIAN_POINT ( 'NONE',  ( -70.61305118522868440, -293.1414661854296924, -201.6899817264562387 ) ) ;
#43594 = CARTESIAN_POINT ( 'NONE',  ( -2.251474464674564580, -293.7111353148000035, -202.2532112226196830 ) ) ;
#43593 = CARTESIAN_POINT ( 'NONE',  ( -37.37352853689063892, -276.5519495502701943, -195.3611179825600175 ) ) ;
#43595 = CARTESIAN_POINT ( 'NONE',  ( -26.17682149680866743, -290.9099957426690821, -344.4092206530166891 ) ) ;
#43596 = CARTESIAN_POINT ( 'NONE',  ( -86.32402219903653418, -275.7331791068950224, -327.0050453120750831 ) ) ;
#43597 = CARTESIAN_POINT ( 'NONE',  ( -92.00906063858325012, -279.7599515512611674, -320.9612480495015916 ) ) ;
#43598 = CARTESIAN_POINT ( 'NONE',  ( 36.33643088854014991, -291.4945711850214707, -259.7381613320289944 ) ) ;
#43599 = CARTESIAN_POINT ( 'NONE',  ( 22.44309122558506076, -284.0446433533261370, -316.9233007567825666 ) ) ;
#43600 = EDGE_LOOP ( 'NONE', ( #14048, #53166, #44308, #33846 ) ) ;
#43601 = CARTESIAN_POINT ( 'NONE',  ( -29.44658400780438967, -282.6162521331363564, -343.0047117862945925 ) ) ;
#43602 = CARTESIAN_POINT ( 'NONE',  ( -19.84018028442471504, -281.3515772202551375, -195.6393795387294574 ) ) ;
#43603 = CARTESIAN_POINT ( 'NONE',  ( -92.16035567197184264, -282.6093419098990580, -323.8674140848385719 ) ) ;
#43604 = CARTESIAN_POINT ( 'NONE',  ( -111.9436626716666723, -279.2657329460377014, -288.5094373461789132 ) ) ;
#43605 = CARTESIAN_POINT ( 'NONE',  ( 0.000000000000000000, 0.000000000000000000, 0.000000000000000000 ) ) ;
#43606 = CARTESIAN_POINT ( 'NONE',  ( 34.06606036054898823, -276.7288368117229993, -243.4605697820171315 ) ) ;
#43607 = CARTESIAN_POINT ( 'NONE',  ( -53.28691492658256834, -285.7662352645559736, -340.3683826091709079 ) ) ;
#43608 = ORIENTED_EDGE ( 'NONE', *, *, #22861, .F. ) ;
#43609 = CARTESIAN_POINT ( 'NONE',  ( -111.7104903519865076, -274.6594503043100985, -262.0357671750476811 ) ) ;
#43610 = CARTESIAN_POINT ( 'NONE',  ( -106.8074949376054690, -276.2149762292806372, -297.6805277849293248 ) ) ;
#43611 = CARTESIAN_POINT ( 'NONE',  ( -71.73393836630971521, -293.3641723441973568, -202.5886988391316663 ) ) ;
#43612 = CARTESIAN_POINT ( 'NONE',  ( 20.59892986062730813, -293.5274092912360402, -314.9548765204012284 ) ) ;
#43613 = CARTESIAN_POINT ( 'NONE',  ( -105.1047351766068800, -289.5883302215836466, -306.7987082442656401 ) ) ;
#43614 = DIRECTION ( 'NONE',  ( -1.000000000000000000, 0.000000000000000000, 0.000000000000000000 ) ) ;
#43616 = CARTESIAN_POINT ( 'NONE',  ( -102.9402803234467711, -283.4067058632400062, -236.5488910603832551 ) ) ;
#43615 = CARTESIAN_POINT ( 'NONE',  ( 39.01738692413017162, -292.1622951732381921, -273.1711208145893011 ) ) ;
#43617 = CARTESIAN_POINT ( 'NONE',  ( -99.34403851998186497, -292.9703891159703062, -229.4439881997940347 ) ) ;
#43618 = CARTESIAN_POINT ( 'NONE',  ( -5.806240482724225771, -283.9438512781578652, -336.7583809588232953 ) ) ;
#43619 = CARTESIAN_POINT ( 'NONE',  ( -111.6911374074538088, -291.2529879756687592, -289.5181570182043629 ) ) ;
#43620 = CARTESIAN_POINT ( 'NONE',  ( -35.66767023911081225, -280.5660321961086652, -197.3063466177145244 ) ) ;
#43621 = CARTESIAN_POINT ( 'NONE',  ( 37.93788804169939510, -292.1688570614683158, -256.1839418016618311 ) ) ;
#43622 = CARTESIAN_POINT ( 'NONE',  ( 30.22558105768289138, -288.8305560230214155, -307.0623292242091793 ) ) ;
#43623 = CARTESIAN_POINT ( 'NONE',  ( -5.646114155181704675, -289.1387010115369662, -340.4675851114491252 ) ) ;
#43624 = CARTESIAN_POINT ( 'NONE',  ( -17.17391338219007935, -286.4863944786068828, -200.1494481451148886 ) ) ;
#43625 = EDGE_LOOP ( 'NONE', ( #50959, #20224, #17425, #31615 ) ) ;
#43626 = FACE_OUTER_BOUND ( 'NONE', #51024, .T. ) ;
#43627 = CARTESIAN_POINT ( 'NONE',  ( 38.41994344512264092, -295.3756935967861637, -267.4598827907016698 ) ) ;
#43628 = CARTESIAN_POINT ( 'NONE',  ( -113.8733620336338532, -295.2108179121724447, -272.4395755413561346 ) ) ;
#43629 = CARTESIAN_POINT ( 'NONE',  ( -110.1392859604227539, -277.4998633469374454, -278.8050807163190257 ) ) ;
#43630 = CARTESIAN_POINT ( 'NONE',  ( -114.2801616667020426, -272.0598842126317436, -270.3548630465568863 ) ) ;
#43631 = CARTESIAN_POINT ( 'NONE',  ( -37.01170354081605751, -293.5277905846670023, -344.0662568071866190 ) ) ;
#43632 = CARTESIAN_POINT ( 'NONE',  ( 21.65808797953431863, -277.9316511720170411, -315.0489129504841230 ) ) ;
#43633 = CARTESIAN_POINT ( 'NONE',  ( -111.1106114664330136, -270.7994961627850898, -262.0536996530543092 ) ) ;
#43634 = CARTESIAN_POINT ( 'NONE',  ( 30.21524673366255342, -294.3725483484116694, -241.5398772946525980 ) ) ;
#43635 = CARTESIAN_POINT ( 'NONE',  ( -66.16205118845314814, -296.5181744713414105, -337.7674488349387616 ) ) ;
#43636 = CARTESIAN_POINT ( 'NONE',  ( -43.52154907986207633, -250.2679838637678529, -453.2970318977559145 ) ) ;
#43637 = CARTESIAN_POINT ( 'NONE',  ( -109.0584444128670185, -294.2617360925467551, -292.9150670596690702 ) ) ;
#43638 = CARTESIAN_POINT ( 'NONE',  ( -40.44446316366844485, -298.6656514654368380, -193.4736156261150199 ) ) ;
#43639 = CARTESIAN_POINT ( 'NONE',  ( -65.33838767548951409, -275.6864015268652679, -200.7686337656099624 ) ) ;
#43640 = CARTESIAN_POINT ( 'NONE',  ( -96.74246357129482021, -290.8962459674995671, -313.1975248219093260 ) ) ;
#43641 = EDGE_CURVE ( 'NONE', #50260, #65076, #88838, .T. ) ;
#43642 = CARTESIAN_POINT ( 'NONE',  ( -53.14982046604436761, -295.5936127400568125, -341.7026030798606371 ) ) ;
#43643 = EDGE_CURVE ( 'NONE', #63355, #26085, #23988, .T. ) ;
#43644 = CARTESIAN_POINT ( 'NONE',  ( -112.4376424708388100, -280.4445564808393101, -277.2072799755403594 ) ) ;
#43645 = CARTESIAN_POINT ( 'NONE',  ( -40.96815612640321547, -278.6922769042372465, -193.9271518185306888 ) ) ;
#43646 = CARTESIAN_POINT ( 'NONE',  ( -74.23438386492938434, -282.8775414476518790, -337.8908435394645835 ) ) ;
#43647 = CARTESIAN_POINT ( 'NONE',  ( 19.79589733069168744, -275.6004455508007709, -321.8454475181493990 ) ) ;
#43648 = CARTESIAN_POINT ( 'NONE',  ( -65.89012771356068754, -281.5083974963083620, -339.1230886815364443 ) ) ;
#43649 = CARTESIAN_POINT ( 'NONE',  ( -90.48547601151642539, -277.7149511082502613, -215.6782426686201291 ) ) ;
#43650 = CARTESIAN_POINT ( 'NONE',  ( 17.83219048080842484, -278.8397325095853034, -219.3133930364245998 ) ) ;
#43651 = CARTESIAN_POINT ( 'NONE',  ( -110.4692925581305190, -271.2345696613039081, -262.1312855415619083 ) ) ;
#43652 = CARTESIAN_POINT ( 'NONE',  ( 37.67935169415434871, -277.5796564973703084, -272.4903740196975264 ) ) ;
#43653 = CIRCLE ( 'NONE', #26970, 4.025000000000000355 ) ;
#43654 = DIRECTION ( 'NONE',  ( -0.9531768234071980039, 0.3024135303179465994, 0.000000000000000000 ) ) ;
#43655 = CARTESIAN_POINT ( 'NONE',  ( 36.16263112649134825, -291.3594750460984528, -253.7043780236438693 ) ) ;
#43656 = CARTESIAN_POINT ( 'NONE',  ( -60.02727588881297294, -289.3382643250567412, -343.9434844327096812 ) ) ;
#43657 = CARTESIAN_POINT ( 'NONE',  ( 20.42517514356521247, -276.8896176595218321, -222.2672872807908675 ) ) ;
#43658 = CARTESIAN_POINT ( 'NONE',  ( -112.1826874425679534, -270.6241775051232707, -264.7388320909179811 ) ) ;
#43659 = CARTESIAN_POINT ( 'NONE',  ( -113.6580699775909693, -283.8613967212689317, -261.4184945825661543 ) ) ;
#43660 = CARTESIAN_POINT ( 'NONE',  ( -23.68628624284178130, -43.55766379199612004, -22.50000000000000000 ) ) ;
#43661 = CARTESIAN_POINT ( 'NONE',  ( -14.19407528283623954, -284.3520576625339800, -198.9689922327230533 ) ) ;
#43662 = DIRECTION ( 'NONE',  ( 0.000000000000000000, 0.000000000000000000, 1.000000000000000000 ) ) ;
#43663 = CARTESIAN_POINT ( 'NONE',  ( 34.34090954822816855, -292.1393868670133429, -254.5316463890218017 ) ) ;
#43664 = CARTESIAN_POINT ( 'NONE',  ( -110.4045761650569233, -282.8631250384627265, -257.1488925995913633 ) ) ;
#43665 = CARTESIAN_POINT ( 'NONE',  ( 208.9116897969394984, 35.81612620979493755, 14.28025116719392074 ) ) ;
#43666 = CARTESIAN_POINT ( 'NONE',  ( 138.6539576904058606, 275.0000000000000568, -10.49999999999999822 ) ) ;
#43667 = CARTESIAN_POINT ( 'NONE',  ( -31.98982391747703957, -290.1194948912177551, -195.5393417737136872 ) ) ;
#43668 = CARTESIAN_POINT ( 'NONE',  ( -52.79628683705556114, -281.7264674402689479, -345.1403757092297155 ) ) ;
#43669 = CARTESIAN_POINT ( 'NONE',  ( -79.06771080223433046, -279.2250859809200279, -331.2951700798008687 ) ) ;
#43670 = CARTESIAN_POINT ( 'NONE',  ( -107.8555923669468513, -285.3727384739846116, -300.4266659618969015 ) ) ;
#43671 = CARTESIAN_POINT ( 'NONE',  ( -19.81585606849540682, -286.2838178161671863, -199.4961422187944606 ) ) ;
#43672 = CARTESIAN_POINT ( 'NONE',  ( -109.6186008093691981, -279.7955041535999499, -284.2632406269470380 ) ) ;
#43673 = CARTESIAN_POINT ( 'NONE',  ( -95.74682072007331612, -279.9727837907842627, -226.2785036770897591 ) ) ;
#43674 = CARTESIAN_POINT ( 'NONE',  ( -108.0990636987140192, -286.8743724093508263, -245.4935457620753709 ) ) ;
#43675 = VERTEX_POINT ( 'NONE', #16889 ) ;
#43676 = CARTESIAN_POINT ( 'NONE',  ( -111.9691736048615098, -296.1475384528994255, -289.3811718663810097 ) ) ;
#43677 = CARTESIAN_POINT ( 'NONE',  ( 2.203871065978271204, -290.4995507143703435, -333.6698425052862831 ) ) ;
#43678 = DIRECTION ( 'NONE',  ( 0.000000000000000000, 1.000000000000000000, 0.000000000000000000 ) ) ;
#43679 = CARTESIAN_POINT ( 'NONE',  ( 40.65961533371913106, -278.2662352645559167, -288.1317622949166548 ) ) ;
#43680 = ORIENTED_EDGE ( 'NONE', *, *, #75213, .T. ) ;
#43681 = CARTESIAN_POINT ( 'NONE',  ( 18.92504472999706522, -292.6587221314950966, -321.8236852042995224 ) ) ;
#43682 = CARTESIAN_POINT ( 'NONE',  ( 16.46761851056848869, -288.3544968016658459, -219.9910868476462156 ) ) ;
#43683 = CARTESIAN_POINT ( 'NONE',  ( -110.1327145725718850, -280.4865871400288029, -256.9655130582736433 ) ) ;
#43684 = CARTESIAN_POINT ( 'NONE',  ( 39.01646439208190742, -289.0279936721215108, -274.3737557109511727 ) ) ;
#43685 = CARTESIAN_POINT ( 'NONE',  ( 14.28337524769959543, -289.6601126252392646, -326.8966267918951871 ) ) ;
#43686 = CARTESIAN_POINT ( 'NONE',  ( -110.6244322515243397, -286.7579729804272120, -254.3435671289555557 ) ) ;
#43687 = CARTESIAN_POINT ( 'NONE',  ( -114.3848676737361814, -278.7032064466724819, -271.6105149549125031 ) ) ;
#43688 = CARTESIAN_POINT ( 'NONE',  ( -11.57174894206314519, -292.7991117062976514, -341.4463610709558452 ) ) ;
#43689 = CARTESIAN_POINT ( 'NONE',  ( 37.86506954685553694, -281.5928518065873618, -286.9429516643293141 ) ) ;
#43690 = CARTESIAN_POINT ( 'NONE',  ( -72.51352105934813608, -275.4422111857547293, -204.9294611848308136 ) ) ;
#43691 = CARTESIAN_POINT ( 'NONE',  ( 199.3264250992830569, 299.0883425075165292, -6.145502011509054618 ) ) ;
#43692 = CARTESIAN_POINT ( 'NONE',  ( 31.98288692825981272, -290.4805209788416391, -303.7098442033569654 ) ) ;
#43693 = CARTESIAN_POINT ( 'NONE',  ( -80.65414666818847422, -271.7138339291482794, -207.8633558666442411 ) ) ;
#43694 = FACE_OUTER_BOUND ( 'NONE', #77824, .T. ) ;
#43695 = CARTESIAN_POINT ( 'NONE',  ( -108.3479958752068910, -278.2866447170324022, -253.1537240446308203 ) ) ;
#43696 = CARTESIAN_POINT ( 'NONE',  ( 27.32192974589782253, -277.2993627368304601, -311.5282727642073155 ) ) ;
#43697 = CARTESIAN_POINT ( 'NONE',  ( -68.31191880699030605, -299.0624760743460229, -203.5924135421674350 ) ) ;
#43698 = CARTESIAN_POINT ( 'NONE',  ( -52.88173496771922544, -282.3052442659360963, -345.5907572744412164 ) ) ;
#43699 = CARTESIAN_POINT ( 'NONE',  ( -109.3308917424071325, -292.0886000120624999, -287.5521129261514375 ) ) ;
#43700 = CARTESIAN_POINT ( 'NONE',  ( -104.6512379963110959, -298.5422759200166638, -234.3027117457391455 ) ) ;
#43701 = CARTESIAN_POINT ( 'NONE',  ( -34.08346385356971808, -299.2971614199084343, -193.7575374131689898 ) ) ;
#43702 = CARTESIAN_POINT ( 'NONE',  ( -9.791947028515874507, -296.6916292587238786, -339.9386972112981766 ) ) ;
#43703 = CARTESIAN_POINT ( 'NONE',  ( -34.80939034443976965, -281.0201362934014355, -345.1643467824383720 ) ) ;
#43704 = CARTESIAN_POINT ( 'NONE',  ( -81.91468632816209094, -291.1295882377192470, -207.5997190764420850 ) ) ;
#43705 = CARTESIAN_POINT ( 'NONE',  ( -4.563534688456956978, -272.5062558468840166, -203.2840338853002038 ) ) ;
#43706 = CARTESIAN_POINT ( 'NONE',  ( -37.99623278272093074, -287.6442016318833339, -194.1639263970458273 ) ) ;
#43707 = CARTESIAN_POINT ( 'NONE',  ( -98.37561611982357590, -288.9108841644597305, -310.9929316632356517 ) ) ;
#43708 = CARTESIAN_POINT ( 'NONE',  ( -93.98250134251853183, -240.8842209496550595, -341.6624768569019466 ) ) ;
#43709 = ORIENTED_EDGE ( 'NONE', *, *, #17514, .T. ) ;
#43710 = CARTESIAN_POINT ( 'NONE',  ( -95.95087428743453017, -288.4618411036333328, -319.4076465295094636 ) ) ;
#43711 = CARTESIAN_POINT ( 'NONE',  ( -26.47593335298036266, -288.5769298078166116, -342.6203711738583593 ) ) ;
#43712 = VERTEX_POINT ( 'NONE', #4088 ) ;
#43713 = CARTESIAN_POINT ( 'NONE',  ( -29.50823570249005456, -287.2288385172611811, -194.0713457680148792 ) ) ;
#43714 = CARTESIAN_POINT ( 'NONE',  ( -83.01667858534520406, -278.0302404586508942, -327.3988506369762490 ) ) ;
#43715 = CARTESIAN_POINT ( 'NONE',  ( 39.13385699784925720, -292.4003695617886365, -264.6181508617400482 ) ) ;
#43716 = CARTESIAN_POINT ( 'NONE',  ( -93.35159915019727350, -284.4832558853427145, -323.0701152733925596 ) ) ;
#43717 = CARTESIAN_POINT ( 'NONE',  ( 29.16717837900045751, -283.5632175286992833, -307.8757635461401492 ) ) ;
#43718 = CARTESIAN_POINT ( 'NONE',  ( -37.30999888295170308, -283.3850083620802138, -347.3530293155156983 ) ) ;
#43720 = CARTESIAN_POINT ( 'NONE',  ( -9.243131624974672889, -280.7632035454689117, -202.9626169985295689 ) ) ;
#43719 = AXIS2_PLACEMENT_3D ( 'NONE', #27136, #75917, #18161 ) ;
#43721 = CARTESIAN_POINT ( 'NONE',  ( -83.97320365025282740, -219.6140998129361321, -352.5802664969301645 ) ) ;
#43722 = CARTESIAN_POINT ( 'NONE',  ( -90.97752918039822134, -229.6550970709923263, -347.1063063428075566 ) ) ;
#43723 = CARTESIAN_POINT ( 'NONE',  ( 24.24861201465908422, -23.26907645984904605, -341.8364469676749877 ) ) ;
#43724 = CARTESIAN_POINT ( 'NONE',  ( -97.97128717005418252, -272.3182944487887767, -229.3237794709698392 ) ) ;
#43725 = CARTESIAN_POINT ( 'NONE',  ( -37.69499331564374245, -294.5640847617744953, -347.3118364924222874 ) ) ;
#43726 = CARTESIAN_POINT ( 'NONE',  ( 194.0023159067837923, 275.6218090567761010, -124.1595538786234272 ) ) ;
#43727 = CARTESIAN_POINT ( 'NONE',  ( -93.77014500029007138, -271.9444184519718419, -218.6781672612716818 ) ) ;
#43728 = CARTESIAN_POINT ( 'NONE',  ( -108.6523958401421197, -298.6809050814571265, -249.7298272196343873 ) ) ;
#43729 = CARTESIAN_POINT ( 'NONE',  ( 24.66333943354051783, -289.4091649891917086, -309.8151234404397769 ) ) ;
#43730 = EDGE_LOOP ( 'NONE', ( #73569, #37230, #68179, #91880, #45925, #10736 ) ) ;
#43731 = CARTESIAN_POINT ( 'NONE',  ( -30.59964104961693820, -295.9101165365055977, -346.8291822462352343 ) ) ;
#43732 = CARTESIAN_POINT ( 'NONE',  ( -39.98241614098324703, -286.5104276740514138, -197.3473175010811076 ) ) ;
#43733 = CARTESIAN_POINT ( 'NONE',  ( -85.60300669407659768, -272.3224516986533104, -210.7596180231304857 ) ) ;
#43734 = CARTESIAN_POINT ( 'NONE',  ( -16.54074434826786089, -295.5929805137505468, -344.3856840888263946 ) ) ;
#43735 = CARTESIAN_POINT ( 'NONE',  ( 34.39637747893767994, -294.3970498302081182, -298.1671447456228634 ) ) ;
#43736 = CARTESIAN_POINT ( 'NONE',  ( -65.32892295345830291, -291.8425571907436620, -202.9256831570402539 ) ) ;
#43737 = ORIENTED_EDGE ( 'NONE', *, *, #13861, .F. ) ;
#43738 = CARTESIAN_POINT ( 'NONE',  ( -21.67762877955538414, -276.1715921763665165, -196.4425745448380383 ) ) ;
#43739 = CARTESIAN_POINT ( 'NONE',  ( 37.78991065937461968, -274.5349149004036349, -285.3026634259592242 ) ) ;
#43740 = VERTEX_POINT ( 'NONE', #32027 ) ;
#43741 = CARTESIAN_POINT ( 'NONE',  ( -111.2763734306744823, -278.3269299897797850, -249.0728351266827190 ) ) ;
#43742 = CARTESIAN_POINT ( 'NONE',  ( 36.17707836545140054, -273.8607265000895268, -263.3649551639949777 ) ) ;
#43743 = CARTESIAN_POINT ( 'NONE',  ( -48.93783186929407947, -274.9807740408643895, -197.9235692558317794 ) ) ;
#43744 = CARTESIAN_POINT ( 'NONE',  ( 17.45365612282845547, -275.8006207662948555, -221.6971292762044925 ) ) ;
#43745 = CARTESIAN_POINT ( 'NONE',  ( -37.62534918568967868, -299.6487773713902811, -194.1616431679639447 ) ) ;
#43746 = CARTESIAN_POINT ( 'NONE',  ( -9.836181847668704847, -274.7147857051502342, -340.5170390964740363 ) ) ;
#43747 = CARTESIAN_POINT ( 'NONE',  ( -41.03608490611206605, -295.7512518029748207, -343.3822242119767907 ) ) ;
#43748 = CARTESIAN_POINT ( 'NONE',  ( -15.43458616841937925, -293.3378237969102429, -340.6674952301746657 ) ) ;
#43749 = CARTESIAN_POINT ( 'NONE',  ( 199.0061125298537377, 250.0000000000000568, -7.725424859374024678 ) ) ;
#43750 = CARTESIAN_POINT ( 'NONE',  ( -93.28493400725571405, -278.3220086836903420, -323.2568890638909238 ) ) ;
#43751 = EDGE_CURVE ( 'NONE', #78013, #29264, #570, .T. ) ;
#43752 = CARTESIAN_POINT ( 'NONE',  ( 22.27960606024607415, -275.1306188513710254, -228.2170412931611736 ) ) ;
#43753 = CARTESIAN_POINT ( 'NONE',  ( -102.0921358743618867, -283.7740724592304105, -229.6096843534307084 ) ) ;
#43754 = CARTESIAN_POINT ( 'NONE',  ( -111.3931695871596474, -298.3832841303209307, -283.5546141073987769 ) ) ;
#43755 = DIRECTION ( 'NONE',  ( -0.000000000000000000, -0.000000000000000000, -1.000000000000000000 ) ) ;
#43756 = CARTESIAN_POINT ( 'NONE',  ( -96.69986180757408079, -284.3463487260885358, -227.5704808760709739 ) ) ;
#43757 = CARTESIAN_POINT ( 'NONE',  ( -108.1907348321117865, -277.0715952243014044, -248.9511134139237072 ) ) ;
#43758 = CARTESIAN_POINT ( 'NONE',  ( -87.51038438886374138, -276.3437488854533512, -324.1986331141633855 ) ) ;
#43760 = EDGE_CURVE ( 'NONE', #44986, #71244, #33810, .T. ) ;
#43759 = CARTESIAN_POINT ( 'NONE',  ( 15.73214179078694031, -284.3014756628151645, -323.4251477768797827 ) ) ;
#43761 = CARTESIAN_POINT ( 'NONE',  ( 35.99953040875986687, -276.8091609505043493, -274.3188249778099816 ) ) ;
#43762 = CARTESIAN_POINT ( 'NONE',  ( 155.8658175007603859, 19.96629232096135098, 14.32310887264949528 ) ) ;
#43763 = CARTESIAN_POINT ( 'NONE',  ( 38.34051367161838186, -274.0696763626419283, -279.6705962231586113 ) ) ;
#43764 = CARTESIAN_POINT ( 'NONE',  ( -70.45057094878701776, -281.6168532638089346, -202.8790381081299472 ) ) ;
#43765 = CARTESIAN_POINT ( 'NONE',  ( 152.4536156746142410, 129.7208004331680797, 12.50000000000000000 ) ) ;
#43766 = CARTESIAN_POINT ( 'NONE',  ( 11.50391496486480136, -290.3008337343053427, -328.0102296968251494 ) ) ;
#43767 = CARTESIAN_POINT ( 'NONE',  ( -35.84621781830518472, -290.0707210140669758, -195.3633988938459254 ) ) ;
#43768 = CARTESIAN_POINT ( 'NONE',  ( 165.2494399300530290, 8.542400036368780647, 9.000000000000001776 ) ) ;
#43769 = CARTESIAN_POINT ( 'NONE',  ( -50.00743799356180119, -296.6818433214320976, -198.0651320073855572 ) ) ;
#43770 = CARTESIAN_POINT ( 'NONE',  ( -88.76950513434790935, -289.4608596972686883, -216.7546326809274149 ) ) ;
#43771 = CARTESIAN_POINT ( 'NONE',  ( -114.4693872376281121, -273.8646567567205921, -270.3778293100139649 ) ) ;
#43772 = CARTESIAN_POINT ( 'NONE',  ( 209.8595557040737845, 37.94592279361958731, 12.09245862095555601 ) ) ;
#43773 = CARTESIAN_POINT ( 'NONE',  ( -17.91964510196394045, -287.2860126728338059, -344.1546917510391950 ) ) ;
#43774 = CARTESIAN_POINT ( 'NONE',  ( -40.74830541753437529, -284.2498549853416989, -194.3993411138964689 ) ) ;
#43775 = CARTESIAN_POINT ( 'NONE',  ( -15.94397345712669711, -284.1951816980555918, -340.7707210863141540 ) ) ;
#43776 = CARTESIAN_POINT ( 'NONE',  ( -82.88727644386374038, -284.4961380497286996, -327.6817052116827540 ) ) ;
#43777 = CARTESIAN_POINT ( 'NONE',  ( -100.9000991719601785, -291.9886904965841268, -310.9384064725188068 ) ) ;
#43778 = CIRCLE ( 'NONE', #51349, 6.154241149514405151 ) ;
#43779 = CARTESIAN_POINT ( 'NONE',  ( -24.16740299958334504, -274.5491193215861472, -194.4638250408869453 ) ) ;
#43780 = CARTESIAN_POINT ( 'NONE',  ( -100.4672205133025500, -289.1894175438212073, -228.7403770448274543 ) ) ;
#43781 = CARTESIAN_POINT ( 'NONE',  ( -104.9755861778273527, -278.0758623858064311, -307.1667895266301116 ) ) ;
#43783 = CARTESIAN_POINT ( 'NONE',  ( 7.061155533618573621, -296.4244801106389673, -330.4274920493517698 ) ) ;
#43782 = CIRCLE ( 'NONE', #86165, 4.000000000000003553 ) ;
#43784 = CARTESIAN_POINT ( 'NONE',  ( -48.18343439339131606, -259.2349860071790317, -447.3766206888182069 ) ) ;
#43785 = CARTESIAN_POINT ( 'NONE',  ( -69.85430415644619018, -291.9805209788416391, -337.9475929042657754 ) ) ;
#43786 = CARTESIAN_POINT ( 'NONE',  ( -68.00529112903117834, -282.1482339243575552, -337.1517435699443013 ) ) ;
#43787 = CARTESIAN_POINT ( 'NONE',  ( -103.3774047792883835, -276.0760238957922184, -306.2681386755523363 ) ) ;
#43788 = CARTESIAN_POINT ( 'NONE',  ( -69.81892380619837013, -272.1121676740978614, -201.2965808681847193 ) ) ;
#43789 = CARTESIAN_POINT ( 'NONE',  ( 35.70334259924545961, -274.9529708153341971, -274.3264179702936758 ) ) ;
#43790 = CARTESIAN_POINT ( 'NONE',  ( -3.333343410057451717, -294.0299275527530654, -204.9842151243176147 ) ) ;
#43791 = CARTESIAN_POINT ( 'NONE',  ( 35.87769660338809530, -294.5345142554991185, -273.4870979987965143 ) ) ;
#43792 = CARTESIAN_POINT ( 'NONE',  ( -34.99681943398362449, -293.5062945300277875, -193.9732830840702036 ) ) ;
#43793 = CARTESIAN_POINT ( 'NONE',  ( 39.11467311429223059, -294.9023003633832900, -273.1398338931202261 ) ) ;
#43794 = CARTESIAN_POINT ( 'NONE',  ( -110.2417807778729610, -296.3351033581044476, -274.1792648812389075 ) ) ;
#43795 = CARTESIAN_POINT ( 'NONE',  ( -73.29585713263305990, -291.5291735445060795, -336.1813219064975442 ) ) ;
#43796 = CARTESIAN_POINT ( 'NONE',  ( -86.10073152399561991, -283.8737515159365898, -329.9560578836664604 ) ) ;
#43797 = CARTESIAN_POINT ( 'NONE',  ( -92.26023765429999912, -271.4169159960144952, -218.1477504421173705 ) ) ;
#43798 = CARTESIAN_POINT ( 'NONE',  ( -29.46082735709656220, -285.9826880334969701, -193.7654794065425392 ) ) ;
#43799 = CARTESIAN_POINT ( 'NONE',  ( -97.40175962688509514, -279.9242146781659244, -314.7067488803897390 ) ) ;
#43800 = CARTESIAN_POINT ( 'NONE',  ( -94.42120560891630987, -283.9963229609776931, -224.1994599312868388 ) ) ;
#43801 = CARTESIAN_POINT ( 'NONE',  ( -9.012805263682816204, -286.6815371362696396, -339.8190490488023556 ) ) ;
#43802 = CARTESIAN_POINT ( 'NONE',  ( -66.85903145171967310, -277.8090417662626805, -200.5826640474423073 ) ) ;
#43803 = CARTESIAN_POINT ( 'NONE',  ( -71.74250447947856912, -195.9422791308210492, -360.7315132586310824 ) ) ;
#43804 = CARTESIAN_POINT ( 'NONE',  ( -73.58071125799985168, -285.0649747014736590, -206.9059095468134899 ) ) ;
#43805 = CARTESIAN_POINT ( 'NONE',  ( 37.75931178895508111, -282.9469798533269795, -285.4557106854428525 ) ) ;
#43806 = CARTESIAN_POINT ( 'NONE',  ( -12.31181026184407656, -287.7932266541396871, -342.9862634846128344 ) ) ;
#43807 = CARTESIAN_POINT ( 'NONE',  ( -56.70090291831119345, -278.8976790862839721, -344.1154021804333638 ) ) ;
#43808 = CARTESIAN_POINT ( 'NONE',  ( -41.34180558713192255, -278.4166650084789012, -346.7764505700321251 ) ) ;
#43809 = CARTESIAN_POINT ( 'NONE',  ( -67.30434741400488008, -279.4812824095527048, -203.7799539836873635 ) ) ;
#43810 = CARTESIAN_POINT ( 'NONE',  ( -54.61611036000540764, -275.8089637426986656, -197.7426523508493119 ) ) ;
#43811 = CARTESIAN_POINT ( 'NONE',  ( 37.09656688678564507, -293.7987332985782700, -290.0574223014764357 ) ) ;
#43812 = CARTESIAN_POINT ( 'NONE',  ( 30.91920072636273176, -285.9712982299749910, -300.6935030813089611 ) ) ;
#43813 = CARTESIAN_POINT ( 'NONE',  ( -98.57402308712372019, -292.7617565300981255, -224.9846160179839387 ) ) ;
#43814 = CARTESIAN_POINT ( 'NONE',  ( -103.9939258800449551, -295.8838608825694223, -239.7151103725387031 ) ) ;
#43815 = CARTESIAN_POINT ( 'NONE',  ( 34.92927226068994173, -293.0811880218096235, -259.9210970647380918 ) ) ;
#43816 = ADVANCED_FACE ( 'NONE', ( #53810 ), #82678, .T. ) ;
#43817 = CARTESIAN_POINT ( 'NONE',  ( -44.88039979122734024, -293.0386417588241557, -193.9889443561916380 ) ) ;
#43818 = CARTESIAN_POINT ( 'NONE',  ( 33.75122589752545821, -282.4284805786579113, -287.4346365581382088 ) ) ;
#43819 = CARTESIAN_POINT ( 'NONE',  ( -20.58003824011520777, -297.1777206810681946, -193.6732168222712289 ) ) ;
#43820 = CARTESIAN_POINT ( 'NONE',  ( -97.20548749604594718, -290.5554468493023137, -318.6482230603169228 ) ) ;
#43821 = CARTESIAN_POINT ( 'NONE',  ( -109.5162230189088604, -282.3967838770487333, -293.4505001835232179 ) ) ;
#43822 = CARTESIAN_POINT ( 'NONE',  ( 14.59257516847157277, -288.6783778740298203, -327.2539087294928777 ) ) ;
#43823 = CARTESIAN_POINT ( 'NONE',  ( -67.56032080925972139, -285.9776975331199651, -203.8861418563127472 ) ) ;
#43824 = CARTESIAN_POINT ( 'NONE',  ( 175.2296996224750103, 128.0000000000000568, 0.000000000000000000 ) ) ;
#43825 = CARTESIAN_POINT ( 'NONE',  ( -32.49377328605026349, -123.7660681094353947, -362.0747317338332891 ) ) ;
#43826 = CARTESIAN_POINT ( 'NONE',  ( 138.3761275019903678, 178.4032963545091661, -238.2084800396306434 ) ) ;
#43827 = CARTESIAN_POINT ( 'NONE',  ( -99.59977877579785854, -278.2791676133982719, -231.8388061061633323 ) ) ;
#43828 = CARTESIAN_POINT ( 'NONE',  ( -7.862580350387181838, -279.3680559078222245, -203.2265432578485331 ) ) ;
#43829 = CARTESIAN_POINT ( 'NONE',  ( 33.69567661556746430, -274.8400821527634434, -240.5681502228325712 ) ) ;
#43830 = CARTESIAN_POINT ( 'NONE',  ( -101.2059816391420384, -255.8329364732449562, -325.0564836861664730 ) ) ;
#43831 = CARTESIAN_POINT ( 'NONE',  ( -102.8966756669376394, -277.6439150704397889, -231.0007761553897296 ) ) ;
#43832 = CARTESIAN_POINT ( 'NONE',  ( -34.81557612609163499, -281.0404013122154652, -344.9758826556931695 ) ) ;
#43833 = CARTESIAN_POINT ( 'NONE',  ( 24.89770203432625095, -295.8966208393606507, -313.9754723689898697 ) ) ;
#43834 = CARTESIAN_POINT ( 'NONE',  ( -64.09998110935865157, -292.1858064316247123, -202.3624066501358811 ) ) ;
#43835 = CARTESIAN_POINT ( 'NONE',  ( -53.53336389100431347, -287.9490785076002339, -342.0484495073671951 ) ) ;
#43836 = CARTESIAN_POINT ( 'NONE',  ( 34.62343721330418589, -275.8602680037275263, -243.2625609396641266 ) ) ;
#43837 = CARTESIAN_POINT ( 'NONE',  ( -94.77212354698522745, -296.0833769705415648, -315.4249224209679028 ) ) ;
#43838 = ORIENTED_EDGE ( 'NONE', *, *, #27340, .F. ) ;
#43839 = DIRECTION ( 'NONE',  ( -0.000000000000000000, -1.000000000000000000, -0.000000000000000000 ) ) ;
#43840 = CARTESIAN_POINT ( 'NONE',  ( 196.7820920054853957, 24.98056201567221635, 13.24702896642047278 ) ) ;
#43841 = CARTESIAN_POINT ( 'NONE',  ( -56.22094678245019850, -281.7310865348313769, -197.1437061014673020 ) ) ;
#43842 = EDGE_CURVE ( 'NONE', #77289, #90976, #52627, .T. ) ;
#43843 = AXIS2_PLACEMENT_3D ( 'NONE', #21815, #50690, #56885 ) ;
#43844 = CARTESIAN_POINT ( 'NONE',  ( 31.35517082314290960, -282.2901848812873595, -244.6232522593568035 ) ) ;
#43845 = CARTESIAN_POINT ( 'NONE',  ( -113.0366189709563685, -280.4038966261870769, -263.1329113806338000 ) ) ;
#43846 = CIRCLE ( 'NONE', #15147, 2.395975569037644970 ) ;
#43847 = CARTESIAN_POINT ( 'NONE',  ( 35.93810580643082631, -280.6236185276035258, -271.3287905638847519 ) ) ;
#43848 = CARTESIAN_POINT ( 'NONE',  ( -96.82970168000497324, -271.6364068563615888, -226.7805554554041976 ) ) ;
#43849 = CARTESIAN_POINT ( 'NONE',  ( 208.6388168579736089, 27.72533456986103317, 12.02378101520651299 ) ) ;
#43850 = DIRECTION ( 'NONE',  ( -0.8195702660916324156, 0.000000000000000000, -0.5729786897769331144 ) ) ;
#43851 = CARTESIAN_POINT ( 'NONE',  ( 35.57347531852190770, -276.0473129241058814, -245.9543226703549976 ) ) ;
#43852 = ORIENTED_EDGE ( 'NONE', *, *, #36263, .T. ) ;
#43853 = CARTESIAN_POINT ( 'NONE',  ( 35.34057441301066405, -277.3146272655753819, -251.8601012629020488 ) ) ;
#43854 = CARTESIAN_POINT ( 'NONE',  ( -110.1111417280659595, -276.8296458870128163, -293.8385715257469997 ) ) ;
#43855 = ORIENTED_EDGE ( 'NONE', *, *, #84181, .F. ) ;
#43856 = DIRECTION ( 'NONE',  ( 0.5335274993777835428, -0.8457827187922967171, 0.000000000000000000 ) ) ;
#43857 = CARTESIAN_POINT ( 'NONE',  ( -106.7030853027152517, -286.1474302321784080, -299.9462420806698901 ) ) ;
#43858 = CARTESIAN_POINT ( 'NONE',  ( -86.02888094471506975, -290.5541441838533956, -215.6837797720032484 ) ) ;
#43859 = ADVANCED_FACE ( 'NONE', ( #85490 ), #56640, .T. ) ;
#43860 = CARTESIAN_POINT ( 'NONE',  ( 25.46664965313900808, -286.3126007077700024, -225.9714876793367182 ) ) ;
#43861 = CARTESIAN_POINT ( 'NONE',  ( -29.35730981752316282, -281.1896220680601459, -343.9937296700563820 ) ) ;
#43863 = CARTESIAN_POINT ( 'NONE',  ( 26.19223815266872890, -285.1079081965983164, -231.5699735935411638 ) ) ;
#43862 = CARTESIAN_POINT ( 'NONE',  ( -89.32325833297035445, -282.3759773022986792, -322.5219354054040082 ) ) ;
#43864 = CARTESIAN_POINT ( 'NONE',  ( -18.61961892768315607, -284.0108196002487375, -341.3829175781882554 ) ) ;
#43865 = CARTESIAN_POINT ( 'NONE',  ( 24.51000108298645941, -272.9770163698478314, -227.9193896109121056 ) ) ;
#43866 = CARTESIAN_POINT ( 'NONE',  ( -89.32543927409190587, -283.7351082154200981, -214.5746402815611020 ) ) ;
#43867 = CARTESIAN_POINT ( 'NONE',  ( -87.25491953841047632, -297.7475330837379488, -326.4099424918628074 ) ) ;
#43868 = CARTESIAN_POINT ( 'NONE',  ( -67.41383070060905425, -280.5890352419417013, -203.5711578420643093 ) ) ;
#43869 = CARTESIAN_POINT ( 'NONE',  ( -77.56347038069934285, -287.5138048358635956, -206.8612154386999862 ) ) ;
#43870 = CARTESIAN_POINT ( 'NONE',  ( 195.7296518112975718, 19.56734160438314873, 12.91086771431476699 ) ) ;
#43871 = LINE ( 'NONE', #36781, #54989 ) ;
#43872 = CARTESIAN_POINT ( 'NONE',  ( 38.00329673141931153, -295.3997119000199518, -264.6650101750379349 ) ) ;
#43873 = CARTESIAN_POINT ( 'NONE',  ( -102.3282010876691857, -276.0511314031393226, -307.9055066036429480 ) ) ;
#43874 = CARTESIAN_POINT ( 'NONE',  ( -43.18024462896039495, -288.3212798056808879, -346.9775014694620836 ) ) ;
#43875 = CARTESIAN_POINT ( 'NONE',  ( 36.42157156636137927, -291.9216372805134370, -268.0329938335682982 ) ) ;
#43876 = CARTESIAN_POINT ( 'NONE',  ( -109.3672217190964489, -277.4292911423320902, -255.6840360473692328 ) ) ;
#43878 = EDGE_CURVE ( 'NONE', #71834, #42078, #72332, .T. ) ;
#43877 = CARTESIAN_POINT ( 'NONE',  ( -110.5854241665983011, -294.5348705711824664, -282.4533622045860284 ) ) ;
#43879 = CARTESIAN_POINT ( 'NONE',  ( -44.36388845285280524, -293.2767947673993376, -197.1530539317977002 ) ) ;
#43880 = CARTESIAN_POINT ( 'NONE',  ( -110.4542110544635705, -280.8376638359844719, -287.0812184334320705 ) ) ;
#43881 = CARTESIAN_POINT ( 'NONE',  ( 14.98901086110268466, -292.8098213345518843, -325.8967321303628637 ) ) ;
#43882 = CARTESIAN_POINT ( 'NONE',  ( 30.69143273250614001, -288.7711097746224596, -241.6293308995907694 ) ) ;
#43883 = CARTESIAN_POINT ( 'NONE',  ( -112.3632089389286932, -288.6390166940348081, -282.4336997310314814 ) ) ;
#43884 = CARTESIAN_POINT ( 'NONE',  ( -56.19921102510999589, -290.7250158839274832, -341.5461504259332628 ) ) ;
#43885 = CARTESIAN_POINT ( 'NONE',  ( 175.2296996224750103, 140.2072866198470251, 0.000000000000000000 ) ) ;
#43886 = CARTESIAN_POINT ( 'NONE',  ( -109.0950958847691084, -291.1661216797250518, -284.7098272671286168 ) ) ;
#43887 = DIRECTION ( 'NONE',  ( 1.000000000000000000, 0.000000000000000000, 0.000000000000000000 ) ) ;
#43888 = CARTESIAN_POINT ( 'NONE',  ( 14.34715685954928155, -289.5500320692665355, -326.9685827087948269 ) ) ;
#43889 = CARTESIAN_POINT ( 'NONE',  ( -91.86584065268043275, -277.2996716465107738, -218.2719317715601903 ) ) ;
#43890 = CARTESIAN_POINT ( 'NONE',  ( -25.40305715213583326, -280.5336310240380726, -194.3136782140570915 ) ) ;
#43891 = CARTESIAN_POINT ( 'NONE',  ( 25.08765291017316912, -281.8164502604197423, -315.4203676390355326 ) ) ;
#43892 = CARTESIAN_POINT ( 'NONE',  ( 37.26648167704814796, -285.4536822679012289, -262.7047575499842651 ) ) ;
#43893 = CARTESIAN_POINT ( 'NONE',  ( 121.3395553409046528, -299.5541904835127980, -191.8695490883551713 ) ) ;
#43894 = CARTESIAN_POINT ( 'NONE',  ( 35.27840652580110969, -279.4911956604726129, -254.8996255427316555 ) ) ;
#43895 = CARTESIAN_POINT ( 'NONE',  ( -8.823591980929922585, -280.6790647675518358, -339.7827283724313929 ) ) ;
#43896 = CARTESIAN_POINT ( 'NONE',  ( 6.586621361128567109, -59.71314100781844303, -351.1713062918258856 ) ) ;
#43897 = CARTESIAN_POINT ( 'NONE',  ( -112.6183987848659882, -276.8743466793583821, -282.8561727090163913 ) ) ;
#43898 = CARTESIAN_POINT ( 'NONE',  ( -109.6811053818439063, -283.7950369421499204, -244.8953967701154966 ) ) ;
#43899 = CARTESIAN_POINT ( 'NONE',  ( -33.80982893058406091, -299.0386861120962863, -197.1252400388727324 ) ) ;
#43900 = CARTESIAN_POINT ( 'NONE',  ( -90.40554557003881087, -292.8853601168768250, -219.0710729265712473 ) ) ;
#43901 = CARTESIAN_POINT ( 'NONE',  ( -34.79678551239572926, -299.3985538800711197, -193.8537097873024209 ) ) ;
#43902 = CARTESIAN_POINT ( 'NONE',  ( 35.66413123561213183, -275.1991483550519320, -268.8657673294840151 ) ) ;
#43903 = CARTESIAN_POINT ( 'NONE',  ( -41.11504517770968192, -297.0997812010708117, -345.2790530161220204 ) ) ;
#43904 = CARTESIAN_POINT ( 'NONE',  ( -20.49433778279724194, -289.0083751281943591, -345.5501079595523493 ) ) ;
#43905 = CARTESIAN_POINT ( 'NONE',  ( 27.06453089242522125, -280.1592517947494230, -309.9716337614506187 ) ) ;
#43906 = CARTESIAN_POINT ( 'NONE',  ( -34.95828677764342984, -291.9145995763387305, -193.3848641482099140 ) ) ;
#43908 = CARTESIAN_POINT ( 'NONE',  ( -110.3582582412613959, -289.5283560155095870, -276.6381833524913532 ) ) ;
#43907 = AXIS2_PLACEMENT_3D ( 'NONE', #34503, #7030, #28801 ) ;
#43909 = CARTESIAN_POINT ( 'NONE',  ( -9.163716676360019520, -292.6837187567485898, -339.9215321763049928 ) ) ;
#43910 = ORIENTED_EDGE ( 'NONE', *, *, #49297, .F. ) ;
#43911 = DIRECTION ( 'NONE',  ( -0.000000000000000000, -1.000000000000000000, -0.000000000000000000 ) ) ;
#43912 = CARTESIAN_POINT ( 'NONE',  ( -105.1725115110989748, -289.6951503130741230, -297.6441111635741663 ) ) ;
#43913 = CARTESIAN_POINT ( 'NONE',  ( 199.0061125298537377, 275.0000000000000568, -12.72542485937401580 ) ) ;
#43914 = AXIS2_PLACEMENT_3D ( 'NONE', #78396, #49040, #12596 ) ;
#43915 = CARTESIAN_POINT ( 'NONE',  ( -65.80130370130943618, -286.6301033374155054, -199.0527479502372330 ) ) ;
#43916 = CARTESIAN_POINT ( 'NONE',  ( -37.30987171927208124, -297.5519495502701375, -340.3611179825599606 ) ) ;
#43917 = CARTESIAN_POINT ( 'NONE',  ( -58.79708573511451419, -294.3816905464427123, -344.1219272551581980 ) ) ;
#43918 = CARTESIAN_POINT ( 'NONE',  ( -55.56836374640140974, -284.5971615363647516, -344.6651354027273442 ) ) ;
#43919 = CARTESIAN_POINT ( 'NONE',  ( -99.60820917864782587, -284.9116670769285520, -232.1612445117027335 ) ) ;
#43920 = CARTESIAN_POINT ( 'NONE',  ( 30.74115971296555827, -277.2371678003347597, -298.1727273250932058 ) ) ;
#43921 = CARTESIAN_POINT ( 'NONE',  ( -31.49819311935199551, -292.9982499648074281, -344.8280862273466596 ) ) ;
#43922 = CARTESIAN_POINT ( 'NONE',  ( 3.341517111109728155, -275.2866304013976446, -331.4512672638328468 ) ) ;
#43923 = VERTEX_POINT ( 'NONE', #5500 ) ;
#43924 = CYLINDRICAL_SURFACE ( 'NONE', #27441, 3.000000000000007994 ) ;
#43925 = CARTESIAN_POINT ( 'NONE',  ( -13.79254825091533476, -294.4213891932420779, -343.6494645141034994 ) ) ;
#43926 = CARTESIAN_POINT ( 'NONE',  ( 33.63945168365759741, -289.1802533405262920, -247.8910439658979783 ) ) ;
#43927 = CARTESIAN_POINT ( 'NONE',  ( -112.3013091418980167, -297.8360021364579211, -254.0963911939644220 ) ) ;
#43928 = CARTESIAN_POINT ( 'NONE',  ( 35.37494195359314375, -288.1048286698856487, -262.8656105004017149 ) ) ;
#43929 = CARTESIAN_POINT ( 'NONE',  ( -114.1421496237037303, -277.6313979254216520, -268.7272552213032100 ) ) ;
#43930 = CARTESIAN_POINT ( 'NONE',  ( -37.68019307119700301, -295.7076600064600598, -347.2715017254911913 ) ) ;
#43931 = CARTESIAN_POINT ( 'NONE',  ( 2.509953869632158163, -286.6639971934728237, -334.8598390977539907 ) ) ;
#43932 = CARTESIAN_POINT ( 'NONE',  ( -103.0953205865691444, -296.3626100400822452, -310.3886795879174088 ) ) ;
#43933 = CARTESIAN_POINT ( 'NONE',  ( -107.0230643449753813, -291.1751839049461523, -248.4879330637774899 ) ) ;
#43934 = CARTESIAN_POINT ( 'NONE',  ( 197.4836817735085219, 42.27872732282707346, 11.66666666666666785 ) ) ;
#43935 = CARTESIAN_POINT ( 'NONE',  ( -110.6395504398199847, -271.5021483123970825, -270.3477634379551660 ) ) ;
#43936 = CARTESIAN_POINT ( 'NONE',  ( 45.91229879761790045, 10.79500447389408180, -328.5722265924176781 ) ) ;
#43937 = CARTESIAN_POINT ( 'NONE',  ( 38.09716837992449001, -288.9263545765463164, -258.7988615211872911 ) ) ;
#43938 = CARTESIAN_POINT ( 'NONE',  ( -99.86837403722181250, -282.6952119285918457, -220.4570493818173702 ) ) ;
#43939 = ORIENTED_EDGE ( 'NONE', *, *, #49884, .T. ) ;
#43940 = CARTESIAN_POINT ( 'NONE',  ( -36.74500289911770778, -279.4080578690017092, -193.4523371623326113 ) ) ;
#43941 = CARTESIAN_POINT ( 'NONE',  ( -86.03591476719596187, -285.7291711703344390, -327.1845452309248117 ) ) ;
#43942 = CARTESIAN_POINT ( 'NONE',  ( -103.5209802914841504, -283.6284706816451262, -232.0602697252504925 ) ) ;
#43943 = CARTESIAN_POINT ( 'NONE',  ( 18.89769419500824199, -286.3143098734357750, -319.2075638371107402 ) ) ;
#43944 = CARTESIAN_POINT ( 'NONE',  ( 24.30780988661840425, -276.8193802305753479, -226.2975501514406744 ) ) ;
#43945 = CARTESIAN_POINT ( 'NONE',  ( -98.50251896629556825, -297.5990085793167168, -230.3027847154496897 ) ) ;
#43946 = CARTESIAN_POINT ( 'NONE',  ( 16.50916399327210371, -292.9510359774853896, -320.3743953365233210 ) ) ;
#43947 = CARTESIAN_POINT ( 'NONE',  ( -69.92674118574088027, -280.2856268490990033, -200.6938370308662343 ) ) ;
#43949 = CARTESIAN_POINT ( 'NONE',  ( -100.8963426182330210, -278.3947543979291481, -234.2404855700987127 ) ) ;
#43948 = CARTESIAN_POINT ( 'NONE',  ( -32.42055882953000179, -276.9885209775325166, -343.2450212210904965 ) ) ;
#43950 = CARTESIAN_POINT ( 'NONE',  ( 13.74826779946631206, -275.8279046361241740, -213.0948172545879800 ) ) ;
#43951 = CARTESIAN_POINT ( 'NONE',  ( -91.12211186784148254, -276.7146977730510002, -325.1087081909852259 ) ) ;
#43952 = CARTESIAN_POINT ( 'NONE',  ( 184.9426652459076479, 263.7189940584568717, -153.2499980067237004 ) ) ;
#43953 = CARTESIAN_POINT ( 'NONE',  ( -90.16780180670041034, -275.7983667034246196, -323.6718310210713412 ) ) ;
#43954 = CARTESIAN_POINT ( 'NONE',  ( -107.8244491619790466, -297.5976398315835922, -300.0071060735955939 ) ) ;
#43955 = EDGE_CURVE ( 'NONE', #58102, #20191, #61852, .T. ) ;
#43956 = CARTESIAN_POINT ( 'NONE',  ( 196.7806748523260012, 250.0000000000000568, -12.67104836398113932 ) ) ;
#43957 = CARTESIAN_POINT ( 'NONE',  ( 139.3989977797154154, 177.7276089766264704, -238.0725708408485843 ) ) ;
#43958 = CARTESIAN_POINT ( 'NONE',  ( -70.13298351644149875, -286.6893129412501935, -204.7806756150225453 ) ) ;
#43959 = CARTESIAN_POINT ( 'NONE',  ( -98.54161512224210639, -286.9195954354957507, -225.2351453106712995 ) ) ;
#43960 = CARTESIAN_POINT ( 'NONE',  ( 27.75268061214526938, -286.4480740683131330, -236.9836725831424928 ) ) ;
#43961 = CARTESIAN_POINT ( 'NONE',  ( -109.8329067194844271, -276.7705925798484827, -284.2650860842762199 ) ) ;
#43962 = CARTESIAN_POINT ( 'NONE',  ( -110.4130066558641232, -286.5833557021732076, -257.1956025475437855 ) ) ;
#43963 = CARTESIAN_POINT ( 'NONE',  ( -39.70424885127346926, -278.5018550133532358, -196.6930236565489736 ) ) ;
#43964 = CARTESIAN_POINT ( 'NONE',  ( -94.82837353542690551, -279.2247955445440084, -316.1690498192689915 ) ) ;
#43965 = CARTESIAN_POINT ( 'NONE',  ( 23.84160967976788470, -275.4916201576054391, -230.4287871889740700 ) ) ;
#43966 = CARTESIAN_POINT ( 'NONE',  ( 38.69447677087688220, -286.4693588440511576, -280.0880675028896007 ) ) ;
#43967 = CARTESIAN_POINT ( 'NONE',  ( 20.00135078341185135, -281.6599002731761630, -219.1951413971889622 ) ) ;
#43968 = CARTESIAN_POINT ( 'NONE',  ( -31.63459242285705031, -283.4743027276146563, -347.1008754879867979 ) ) ;
#43969 = ORIENTED_EDGE ( 'NONE', *, *, #21572, .T. ) ;
#43970 = EDGE_LOOP ( 'NONE', ( #73348, #67827 ) ) ;
#43971 = LINE ( 'NONE', #21284, #539 ) ;
#43972 = CARTESIAN_POINT ( 'NONE',  ( -56.94803817897030740, -291.1626689396801453, -343.5993280237652243 ) ) ;
#43973 = CARTESIAN_POINT ( 'NONE',  ( -71.70010641476484636, -288.1814959839315975, -338.7189865275929606 ) ) ;
#43974 = CARTESIAN_POINT ( 'NONE',  ( -94.04252156878439450, -297.4541001079250577, -321.2869098794395768 ) ) ;
#43975 = CARTESIAN_POINT ( 'NONE',  ( -39.16211993168021621, -297.2259266605749986, -197.2098559609576398 ) ) ;
#43976 = EDGE_CURVE ( 'NONE', #13568, #64042, #46547, .T. ) ;
#43977 = EDGE_CURVE ( 'NONE', #91341, #86001, #78355, .T. ) ;
#43978 = CARTESIAN_POINT ( 'NONE',  ( 22.13569942842645233, -292.2453615147028927, -221.6194342911086608 ) ) ;
#43979 = CARTESIAN_POINT ( 'NONE',  ( 24.12294964675093212, -285.4722109202510296, -229.6139952526254433 ) ) ;
#43980 = CARTESIAN_POINT ( 'NONE',  ( -49.83805983295521713, -290.1305635207045270, -197.3583107231216616 ) ) ;
#43981 = CARTESIAN_POINT ( 'NONE',  ( -3.167891246722748022, -289.7956196537449500, -335.3734094343310517 ) ) ;
#43982 = CARTESIAN_POINT ( 'NONE',  ( 21.27581636871892101, -295.4090924074130839, -223.5744983911110353 ) ) ;
#43983 = CARTESIAN_POINT ( 'NONE',  ( 28.61627507404245563, -290.0276912192342706, -306.1705853382319447 ) ) ;
#43984 = CARTESIAN_POINT ( 'NONE',  ( -3.899829629486747606, -286.6120053630060625, -337.6930739801743471 ) ) ;
#43985 = VECTOR ( 'NONE', #52646, 1000.000000000000000 ) ;
#43986 = CARTESIAN_POINT ( 'NONE',  ( -29.78056737124442677, -290.9567199945363996, -345.0304473626831623 ) ) ;
#43987 = CARTESIAN_POINT ( 'NONE',  ( -109.8468582027819878, -285.6290503384535668, -260.0455714260510831 ) ) ;
#43988 = CARTESIAN_POINT ( 'NONE',  ( 35.96747810008972834, -295.3388831340281513, -253.6964863504453263 ) ) ;
#43989 = PLANE ( 'NONE',  #20156 ) ;
#43990 = CARTESIAN_POINT ( 'NONE',  ( 164.5961120329530161, 215.0000000000000568, 23.14243616685809002 ) ) ;
#43991 = CARTESIAN_POINT ( 'NONE',  ( -54.97374857452631147, -275.8064216708332310, -197.0977733460076138 ) ) ;
#43992 = CARTESIAN_POINT ( 'NONE',  ( -13.48635367079022451, -281.9316368217291142, -339.5778642325623764 ) ) ;
#43993 = CARTESIAN_POINT ( 'NONE',  ( -71.13837325483054030, -281.4980089448363856, -337.3290889095470675 ) ) ;
#43994 = CARTESIAN_POINT ( 'NONE',  ( -110.6488173352366857, -295.4588708060402382, -293.4318003339238885 ) ) ;
#43995 = CARTESIAN_POINT ( 'NONE',  ( -108.9142837430079709, -271.0398311269453870, -251.3143658052405840 ) ) ;
#43996 = CARTESIAN_POINT ( 'NONE',  ( -46.10135080718824696, -275.2438111847399114, -344.3355590814085190 ) ) ;
#43997 = CARTESIAN_POINT ( 'NONE',  ( -98.86954993854234885, -298.4217027132953035, -230.0748759432026702 ) ) ;
#43998 = DIRECTION ( 'NONE',  ( 1.000000000000000000, -0.000000000000000000, -0.000000000000000000 ) ) ;
#43999 = CARTESIAN_POINT ( 'NONE',  ( -50.31683694748694080, -293.4553212652793377, -345.2850424684869495 ) ) ;
#44000 = CARTESIAN_POINT ( 'NONE',  ( 30.03678288590383261, -295.3722993304892270, -299.9502197308556219 ) ) ;
#44001 = CARTESIAN_POINT ( 'NONE',  ( 180.7149167944524493, -12.49482340714361506, 13.00000000000000178 ) ) ;
#44002 = CARTESIAN_POINT ( 'NONE',  ( -90.51758653591971893, -296.6320981476472980, -320.6827151364626047 ) ) ;
#44003 = DIRECTION ( 'NONE',  ( -5.501794166262391869E-14, -0.01273136352371387336, 0.9999189529070978688 ) ) ;
#44005 = CARTESIAN_POINT ( 'NONE',  ( -108.5918691158734362, -296.3425693358669832, -286.2486419939053235 ) ) ;
#44004 = CARTESIAN_POINT ( 'NONE',  ( -103.9658304673356781, -283.0380823914529742, -235.0410544692495023 ) ) ;
#44006 = CARTESIAN_POINT ( 'NONE',  ( -96.27031319143111432, -283.8845804630171301, -319.9437883758359362 ) ) ;
#44007 = CARTESIAN_POINT ( 'NONE',  ( -37.29021556066937393, -284.9716242599978955, -345.9339257643217138 ) ) ;
#44008 = CARTESIAN_POINT ( 'NONE',  ( 34.83587874115121963, -286.8804463637044364, -243.6002996086376413 ) ) ;
#44009 = CARTESIAN_POINT ( 'NONE',  ( 37.47377772135444474, -291.5935751655678132, -273.5929287683359235 ) ) ;
#44010 = CARTESIAN_POINT ( 'NONE',  ( -111.9267015750301368, -277.9815159672648406, -251.8345809438482092 ) ) ;
#44011 = CARTESIAN_POINT ( 'NONE',  ( -106.6379572354042153, -270.4809262143061233, -236.9535640164627068 ) ) ;
#44012 = CARTESIAN_POINT ( 'NONE',  ( -48.18343439339133027, -257.5766546844819231, -488.5262689091863990 ) ) ;
#44013 = CARTESIAN_POINT ( 'NONE',  ( 18.97625804578514064, -285.6824366292649415, -223.2733042783450799 ) ) ;
#44014 = CARTESIAN_POINT ( 'NONE',  ( -114.0592620446531384, -289.4977473901165013, -268.3490466277049222 ) ) ;
#44015 = CARTESIAN_POINT ( 'NONE',  ( 196.1963538710215857, 305.7026273589066250, -40.00000000000000711 ) ) ;
#44016 = CARTESIAN_POINT ( 'NONE',  ( -95.39020467250708180, -297.5165932479951039, -315.9331657504804980 ) ) ;
#44017 = CARTESIAN_POINT ( 'NONE',  ( -99.77807564016275421, -280.5647437018456571, -226.3122212162727749 ) ) ;
#44019 = CARTESIAN_POINT ( 'NONE',  ( 35.16024665971853835, -281.3389308217348344, -279.4650824045208992 ) ) ;
#44018 = CARTESIAN_POINT ( 'NONE',  ( 31.89513393361116655, -291.9609026510638046, -300.2361549402726268 ) ) ;
#44020 = CARTESIAN_POINT ( 'NONE',  ( -66.92247652897121668, -295.5959084278559317, -341.4666527624883656 ) ) ;
#44021 = CARTESIAN_POINT ( 'NONE',  ( 27.47609378644173361, -285.1147926927037588, -231.4275956051534422 ) ) ;
#44022 = CARTESIAN_POINT ( 'NONE',  ( -111.7779455287604549, -280.4291977328733765, -279.9497437665503980 ) ) ;
#44023 = CARTESIAN_POINT ( 'NONE',  ( -109.9679735975299479, -295.7398603426686918, -260.5533841559553707 ) ) ;
#44024 = VERTEX_POINT ( 'NONE', #13538 ) ;
#44025 = DIRECTION ( 'NONE',  ( 0.000000000000000000, 1.000000000000000000, -0.000000000000000000 ) ) ;
#44026 = CARTESIAN_POINT ( 'NONE',  ( 37.34895488333177838, -283.5442926905524246, -271.3100599552428207 ) ) ;
#44027 = DIRECTION ( 'NONE',  ( 0.000000000000000000, -1.000000000000000000, 0.000000000000000000 ) ) ;
#44028 = CARTESIAN_POINT ( 'NONE',  ( -106.6379572354042296, -294.4809262143061233, -236.9535640164627353 ) ) ;
#44029 = CARTESIAN_POINT ( 'NONE',  ( 13.86449909642468903, -273.9457036916368224, -213.0005312680847283 ) ) ;
#44030 = CARTESIAN_POINT ( 'NONE',  ( -90.75773791819591452, -291.1010935544093172, -220.5859595276169784 ) ) ;
#44031 = CARTESIAN_POINT ( 'NONE',  ( 30.98454119687911756, -283.4385049435863948, -297.9696763904863701 ) ) ;
#44032 = CARTESIAN_POINT ( 'NONE',  ( -85.85118687162413664, -274.9675836832465734, -214.6758155856233543 ) ) ;
#44033 = CARTESIAN_POINT ( 'NONE',  ( -24.64658907743955751, -284.4930211980681065, -345.5497161803204449 ) ) ;
#44034 = CARTESIAN_POINT ( 'NONE',  ( 33.70401374697776475, -280.5896469540128919, -288.8403828828775204 ) ) ;
#44035 = CARTESIAN_POINT ( 'NONE',  ( -99.66950811787887687, -281.1173109069549696, -228.5526125903427612 ) ) ;
#44036 = CARTESIAN_POINT ( 'NONE',  ( 30.78831685937531049, -298.8830859118043577, -193.3610866696328685 ) ) ;
#44037 = ORIENTED_EDGE ( 'NONE', *, *, #23779, .T. ) ;
#44038 = CARTESIAN_POINT ( 'NONE',  ( -71.40089124612519811, -273.4480738680367722, -201.3033776132195669 ) ) ;
#44039 = CARTESIAN_POINT ( 'NONE',  ( 33.15705719761975701, -295.1590049182086659, -246.3001998660506899 ) ) ;
#44040 = FACE_BOUND ( 'NONE', #11263, .T. ) ;
#44041 = EDGE_CURVE ( 'NONE', #82488, #22426, #18763, .T. ) ;
#44042 = CARTESIAN_POINT ( 'NONE',  ( 140.6539576904058606, 132.0000000000000568, 12.50000000000000000 ) ) ;
#44043 = CARTESIAN_POINT ( 'NONE',  ( 27.04354491183867637, -292.2236898665133253, -310.3951552170983064 ) ) ;
#44044 = CARTESIAN_POINT ( 'NONE',  ( -51.56730856098430849, -273.3730523486319157, -198.6460418883233672 ) ) ;
#44045 = COLOUR_RGB ( '',0.7921568627450980005, 0.8196078431372548767, 0.9333333333333333481 ) ;
#44046 = CARTESIAN_POINT ( 'NONE',  ( -73.12586384935194417, -293.1067565478068104, -202.9504948871793317 ) ) ;
#44048 = CARTESIAN_POINT ( 'NONE',  ( 10.85697776918869550, -293.9066046520351847, -210.7538535782440192 ) ) ;
#44047 = CARTESIAN_POINT ( 'NONE',  ( 35.77081079830085031, -283.8376638359844719, -253.6410175316879361 ) ) ;
#44049 = CARTESIAN_POINT ( 'NONE',  ( 21.82221221409689704, -290.1820178877637204, -316.2039214950164023 ) ) ;
#44050 = CARTESIAN_POINT ( 'NONE',  ( 21.44729925277438198, -274.1893918510941717, -316.6838195015088218 ) ) ;
#44051 = CARTESIAN_POINT ( 'NONE',  ( -62.24905186942313406, -279.2986389848290969, -340.5653095155972210 ) ) ;
#44052 = CARTESIAN_POINT ( 'NONE',  ( 17.19785535431074663, -292.3461535648852987, -321.0242316466182615 ) ) ;
#44053 = CARTESIAN_POINT ( 'NONE',  ( 10.03191374539644443, -282.5570908980043328, -211.1665178621244365 ) ) ;
#44054 = ORIENTED_EDGE ( 'NONE', *, *, #72628, .T. ) ;
#44055 = CARTESIAN_POINT ( 'NONE',  ( -36.19745628623380185, -282.7041319216452280, -343.3732963701150425 ) ) ;
#44056 = CARTESIAN_POINT ( 'NONE',  ( -90.85237773420880103, -280.3943191650643030, -215.3498351192494624 ) ) ;
#44057 = CARTESIAN_POINT ( 'NONE',  ( 33.19427606454001989, -280.7308528344065621, -300.3743469823941723 ) ) ;
#44058 = CARTESIAN_POINT ( 'NONE',  ( 0.9401287792214468864, -277.4959810107822022, -336.9595388358503101 ) ) ;
#44059 = CARTESIAN_POINT ( 'NONE',  ( 0.000000000000000000, 0.000000000000000000, 0.000000000000000000 ) ) ;
#44060 = CARTESIAN_POINT ( 'NONE',  ( 14.42714466803189488, -277.8602959427839778, -326.4927907685060973 ) ) ;
#44061 = CARTESIAN_POINT ( 'NONE',  ( -82.08285599513421005, -292.1948066931273615, -326.5171145203363494 ) ) ;
#44062 = ORIENTED_EDGE ( 'NONE', *, *, #10535, .F. ) ;
#44063 = CARTESIAN_POINT ( 'NONE',  ( -112.1759815451095648, -274.5879229915463497, -267.5942600973444314 ) ) ;
#44064 = CARTESIAN_POINT ( 'NONE',  ( -35.09278364630892355, -275.0438771422349760, -344.9720366219190169 ) ) ;
#44065 = CARTESIAN_POINT ( 'NONE',  ( -112.1318886583186298, -292.1411412107378851, -283.8658639234906786 ) ) ;
#44066 = CARTESIAN_POINT ( 'NONE',  ( 21.40344152879438866, -293.5099179007456769, -313.8686000995709833 ) ) ;
#44067 = CARTESIAN_POINT ( 'NONE',  ( 21.43794956855026257, -287.7291601388004665, -320.0046440960488212 ) ) ;
#44069 = CARTESIAN_POINT ( 'NONE',  ( -48.46919692003073266, -281.5960250828873086, -343.3174009800020485 ) ) ;
#44068 = CARTESIAN_POINT ( 'NONE',  ( -32.07140973467762990, -293.5616551262005487, -346.6030736061757693 ) ) ;
#44070 = CARTESIAN_POINT ( 'NONE',  ( -37.24298847226193487, -290.9113190842841163, -344.5962561593825626 ) ) ;
#44071 = CARTESIAN_POINT ( 'NONE',  ( -110.1867015026350600, -282.8820420828877218, -281.8386576080146142 ) ) ;
#44072 = CARTESIAN_POINT ( 'NONE',  ( -51.09386472680689195, -284.5466457170364265, -342.6080647163242929 ) ) ;
#44073 = CARTESIAN_POINT ( 'NONE',  ( -95.27283547468262270, -290.8104941890112514, -320.7278110533723634 ) ) ;
#44074 = CARTESIAN_POINT ( 'NONE',  ( 35.76448144918371241, -282.0569870537689212, -271.3083043585982068 ) ) ;
#44075 = CARTESIAN_POINT ( 'NONE',  ( -50.48307129441754881, -290.6828405046820762, -194.8938198896414065 ) ) ;
#44076 = CARTESIAN_POINT ( 'NONE',  ( -30.90758565753862896, -286.9343125435161710, -193.7791826253577483 ) ) ;
#44077 = CARTESIAN_POINT ( 'NONE',  ( 38.04924404560624396, -288.2366681199042660, -285.7146986745073036 ) ) ;
#44078 = CARTESIAN_POINT ( 'NONE',  ( -38.62703663849384839, -286.2023055395117694, -197.3599528656638711 ) ) ;
#44079 = ORIENTED_EDGE ( 'NONE', *, *, #60023, .T. ) ;
#44080 = CARTESIAN_POINT ( 'NONE',  ( 195.3232612940492174, 24.75642484911453423, 13.12563582463413248 ) ) ;
#44081 = CARTESIAN_POINT ( 'NONE',  ( 1.162439852943140117, -296.4041810372761461, -335.6124527175344383 ) ) ;
#44082 = CARTESIAN_POINT ( 'NONE',  ( -41.93281779182947133, -293.7935620943900403, -346.7821476352028185 ) ) ;
#44083 = CARTESIAN_POINT ( 'NONE',  ( -94.64461489327443644, -276.9687349921433679, -315.9858064458254034 ) ) ;
#44084 = CARTESIAN_POINT ( 'NONE',  ( -40.42784804039752089, -297.3630355600913617, -193.4729457260481240 ) ) ;
#44085 = CARTESIAN_POINT ( 'NONE',  ( 35.00134795276837707, -292.2155278483286338, -284.4035945560945606 ) ) ;
#44086 = CARTESIAN_POINT ( 'NONE',  ( 1.120180119018857390, -276.3334292749432279, -207.1261768427396532 ) ) ;
#44087 = CARTESIAN_POINT ( 'NONE',  ( -100.7535733172028074, -295.3112091459133808, -232.0920309628987184 ) ) ;
#44088 = CARTESIAN_POINT ( 'NONE',  ( 34.16574114520963690, -294.9749937863874720, -286.9639354778252027 ) ) ;
#44089 = CARTESIAN_POINT ( 'NONE',  ( 32.08937811181002076, -294.3186577444822092, -246.6755098941000597 ) ) ;
#44090 = CARTESIAN_POINT ( 'NONE',  ( -43.53958171220627804, -248.2610745740583695, -461.0558268132327271 ) ) ;
#44091 = CARTESIAN_POINT ( 'NONE',  ( -104.3355556495353085, -294.1010451522216158, -304.5617979576796870 ) ) ;
#44092 = CARTESIAN_POINT ( 'NONE',  ( -69.15345023634576194, -275.6339466818183155, -202.4278764260954802 ) ) ;
#44093 = CARTESIAN_POINT ( 'NONE',  ( -108.9431327409230335, -291.6956845764705690, -254.9779032123171021 ) ) ;
#44094 = CARTESIAN_POINT ( 'NONE',  ( -58.41028401930568492, -295.6654315039409653, -340.2767976225544544 ) ) ;
#44095 = CARTESIAN_POINT ( 'NONE',  ( -102.1774678322762355, -280.0196401391015115, -308.8656015513670923 ) ) ;
#44096 = CARTESIAN_POINT ( 'NONE',  ( -84.25126708559081123, -278.1073271894395589, -209.8557645281158841 ) ) ;
#44097 = EDGE_CURVE ( 'NONE', #75708, #58726, #19683, .T. ) ;
#44098 = CARTESIAN_POINT ( 'NONE',  ( 23.43237999708655650, -275.5309273536360593, -317.4974788400439820 ) ) ;
#44099 = CARTESIAN_POINT ( 'NONE',  ( -111.3064047064652016, -282.5175766163941375, -279.2056421071889645 ) ) ;
#44100 = CARTESIAN_POINT ( 'NONE',  ( -112.2063405631591593, -277.1324029294298157, -256.0884034393978936 ) ) ;
#44101 = CARTESIAN_POINT ( 'NONE',  ( -67.90322790702578004, -277.6518030891620583, -201.6737823018166580 ) ) ;
#44102 = ADVANCED_FACE ( 'NONE', ( #69412 ), #19224, .T. ) ;
#44103 = CARTESIAN_POINT ( 'NONE',  ( -110.7754166671343086, -271.1989731141462698, -264.8514040384455370 ) ) ;
#44104 = CARTESIAN_POINT ( 'NONE',  ( -1.849681332598452244, -276.5224153657350712, -204.2762730632705370 ) ) ;
#44105 = CYLINDRICAL_SURFACE ( 'NONE', #68611, 0.5000000000000043299 ) ;
#44106 = TOROIDAL_SURFACE ( 'NONE', #21489, 1.000000000000000000, 0.5000000000000000000 ) ;
#44107 = CARTESIAN_POINT ( 'NONE',  ( -72.64043411783150361, -289.6073080689881749, -203.7702201917964828 ) ) ;
#44108 = CIRCLE ( 'NONE', #21492, 0.5000000000000004441 ) ;
#44109 = CARTESIAN_POINT ( 'NONE',  ( -78.13640619104597818, -289.5841849134964718, -335.7286898721372381 ) ) ;
#44110 = CARTESIAN_POINT ( 'NONE',  ( -36.97488297297677917, -276.0569231675438004, -195.1826011640731053 ) ) ;
#44111 = CARTESIAN_POINT ( 'NONE',  ( -36.43070675429654415, -296.0634240084475550, -195.5280873641150663 ) ) ;
#44112 = CARTESIAN_POINT ( 'NONE',  ( -80.83835934114465260, -284.6757198884120612, -206.9549748846036437 ) ) ;
#44113 = LINE ( 'NONE', #1053, #50207 ) ;
#44114 = AXIS2_PLACEMENT_3D ( 'NONE', #92685, #27854, #7001 ) ;
#44115 = CARTESIAN_POINT ( 'NONE',  ( -104.0717042862764288, -282.0978181708819648, -304.7093259955146323 ) ) ;
#44116 = CARTESIAN_POINT ( 'NONE',  ( 170.8178014930282700, 8.542400036368780647, 25.74970488511327815 ) ) ;
#44117 = CARTESIAN_POINT ( 'NONE',  ( -5.857461145425837401, -291.2704756189223758, -204.0458778779909892 ) ) ;
#44118 = CARTESIAN_POINT ( 'NONE',  ( -109.8666489912981916, -282.8980214791935737, -254.4589625155815895 ) ) ;
#44119 = DIRECTION ( 'NONE',  ( 0.9999189529070979798, -0.01273136352371030157, 0.000000000000000000 ) ) ;
#44120 = CARTESIAN_POINT ( 'NONE',  ( 31.70674536624019879, -291.1678279935823639, -240.9482378215590472 ) ) ;
#44121 = CARTESIAN_POINT ( 'NONE',  ( -70.79745113023881231, -279.1012749278464184, -336.1422181713911073 ) ) ;
#44122 = CARTESIAN_POINT ( 'NONE',  ( -93.63840408274512583, -286.4688374217048477, -218.3344450476159864 ) ) ;
#44124 = CARTESIAN_POINT ( 'NONE',  ( -38.62490764333821858, -286.0356524706753589, -197.3599154069878239 ) ) ;
#44123 = CARTESIAN_POINT ( 'NONE',  ( 34.68249033531274961, -273.9246005445561991, -293.2047207221085614 ) ) ;
#44125 = CARTESIAN_POINT ( 'NONE',  ( -108.7393801580826818, -279.7434630676462461, -288.2384494771071672 ) ) ;
#44126 = CARTESIAN_POINT ( 'NONE',  ( -16.32472344052246882, -277.5764120391957590, -340.4919777814241684 ) ) ;
#44127 = CARTESIAN_POINT ( 'NONE',  ( -99.35748562819151175, -287.1243932113331425, -228.0906294698411614 ) ) ;
#44128 = VERTEX_POINT ( 'NONE', #49507 ) ;
#44129 = CARTESIAN_POINT ( 'NONE',  ( -110.6395504398199847, -271.5021483123970825, -270.3477634379551660 ) ) ;
#44130 = CARTESIAN_POINT ( 'NONE',  ( -112.8882716364605159, -296.5725423155080307, -255.4032052554253198 ) ) ;
#44131 = CARTESIAN_POINT ( 'NONE',  ( 19.08509719053820675, -290.2137259213678817, -319.3043090022773640 ) ) ;
#44132 = CARTESIAN_POINT ( 'NONE',  ( 156.4947056272797852, 21.00000000000000000, -15.00000000000000000 ) ) ;
#44133 = CARTESIAN_POINT ( 'NONE',  ( 13.84574458161073096, -278.9090924074131408, -334.4957818155094174 ) ) ;
#44134 = CARTESIAN_POINT ( 'NONE',  ( -92.84052196834250026, -278.1997472452241027, -217.3572569169104440 ) ) ;
#44135 = CARTESIAN_POINT ( 'NONE',  ( 16.93424471673715814, -291.2091459564875322, -216.8025723418089115 ) ) ;
#44136 = CARTESIAN_POINT ( 'NONE',  ( 35.81481182980429168, -289.1883037335769586, -279.2398853642694121 ) ) ;
#44137 = CARTESIAN_POINT ( 'NONE',  ( -46.60520626743090133, -281.6932587640106362, -196.8779665232102616 ) ) ;
#44138 = CARTESIAN_POINT ( 'NONE',  ( 16.28545371658437801, -289.7344440529325311, -324.8657211449441320 ) ) ;
#44139 = CARTESIAN_POINT ( 'NONE',  ( -108.4361152196800333, -286.8630330684059118, -246.3114162501495628 ) ) ;
#44140 = CARTESIAN_POINT ( 'NONE',  ( -70.29909077224183989, -277.6411918085017874, -339.9658592409560356 ) ) ;
#44141 = VERTEX_POINT ( 'NONE', #47621 ) ;
#44142 = CARTESIAN_POINT ( 'NONE',  ( -110.9278836594412496, -270.7306310512091727, -256.4792130527324616 ) ) ;
#44143 = CARTESIAN_POINT ( 'NONE',  ( 37.43061990652664406, -291.4888294980463570, -259.1274482269715236 ) ) ;
#44144 = CARTESIAN_POINT ( 'NONE',  ( -35.33390146101689311, -279.9099900183558702, -193.3741626031550709 ) ) ;
#44145 = CARTESIAN_POINT ( 'NONE',  ( -59.87271460015958979, -275.6176736148978534, -199.5738591962133910 ) ) ;
#44146 = DIRECTION ( 'NONE',  ( -1.000000000000000000, 0.000000000000000000, 0.000000000000000000 ) ) ;
#44147 = CARTESIAN_POINT ( 'NONE',  ( -37.30987171927208124, -291.5519495502701943, -345.3611179825600175 ) ) ;
#44148 = CARTESIAN_POINT ( 'NONE',  ( -36.92251312779276873, -272.2972305803796189, -194.3627234916388602 ) ) ;
#44149 = DIRECTION ( 'NONE',  ( -0.01818181818182024526, -0.000000000000000000, -0.9998346970812742596 ) ) ;
#44150 = CARTESIAN_POINT ( 'NONE',  ( -30.25017641578499195, -279.6517930434106916, -197.5941559951730255 ) ) ;
#44151 = CARTESIAN_POINT ( 'NONE',  ( -2.889871793493798524, -277.8121324800636671, -338.7941418375052081 ) ) ;
#44152 = CARTESIAN_POINT ( 'NONE',  ( -92.29691102077217124, -298.6716372440093323, -221.4193187341389546 ) ) ;
#44153 = CARTESIAN_POINT ( 'NONE',  ( -97.86632649394189798, -282.9780834495130648, -317.5796505446180049 ) ) ;
#44154 = CARTESIAN_POINT ( 'NONE',  ( 33.28728010440637064, -289.6035135905833044, -292.6569862521859022 ) ) ;
#44155 = CARTESIAN_POINT ( 'NONE',  ( -108.2515440643995674, -298.4346764019963416, -242.0321233671757852 ) ) ;
#44156 = EDGE_CURVE ( 'NONE', #33034, #74793, #64793, .T. ) ;
#44157 = CARTESIAN_POINT ( 'NONE',  ( -89.35003785156875722, -298.5445892839471185, -214.0474356187960154 ) ) ;
#44158 = EDGE_CURVE ( 'NONE', #10842, #23364, #77453, .T. ) ;
#44159 = CARTESIAN_POINT ( 'NONE',  ( 33.27843931474874495, -295.8754012364652795, -295.2717191445337903 ) ) ;
#44160 = CARTESIAN_POINT ( 'NONE',  ( -88.19285662459073194, -281.7653921851065206, -325.3336579998240268 ) ) ;
#44161 = CARTESIAN_POINT ( 'NONE',  ( -88.44132444995396725, -271.3522266511541829, -215.8782857808451467 ) ) ;
#44162 = CARTESIAN_POINT ( 'NONE',  ( 35.08223714319956343, -288.8491702274219506, -246.5025610590157044 ) ) ;
#44163 = CARTESIAN_POINT ( 'NONE',  ( -45.41006640045394960, -288.0771063677282768, -343.2248781042105179 ) ) ;
#44164 = CARTESIAN_POINT ( 'NONE',  ( 195.5582280236794475, 277.9486174577299380, -125.6969904412313070 ) ) ;
#44165 = VERTEX_POINT ( 'NONE', #71298 ) ;
#44166 = CARTESIAN_POINT ( 'NONE',  ( -38.92629107760777885, -287.6464015149084048, -346.7554591757346998 ) ) ;
#44167 = CARTESIAN_POINT ( 'NONE',  ( -69.98571976429278152, -289.1611452922231820, -335.6930913783895107 ) ) ;
#44168 = VERTEX_POINT ( 'NONE', #5022 ) ;
#44169 = CARTESIAN_POINT ( 'NONE',  ( -46.48234764152076792, -287.0183941167695139, -194.2169056462059871 ) ) ;
#44170 = CARTESIAN_POINT ( 'NONE',  ( -7.495127165695278038, -276.9829737251915844, -337.0039688313361808 ) ) ;
#44171 = CARTESIAN_POINT ( 'NONE',  ( 3.986582512691288382, -291.5148054197242686, -205.6957994855593483 ) ) ;
#44172 = CARTESIAN_POINT ( 'NONE',  ( -0.4170870768949739293, -283.2259664171843383, -337.8288788632528963 ) ) ;
#44173 = CARTESIAN_POINT ( 'NONE',  ( -2.722154013542533502, -282.0215261930935071, -202.3450922761558672 ) ) ;
#44174 = CARTESIAN_POINT ( 'NONE',  ( -74.26211103376897427, -283.8620768005749255, -337.9678166649973718 ) ) ;
#44175 = CARTESIAN_POINT ( 'NONE',  ( 32.75369649040284514, -281.6148138787478388, -249.8983992065044220 ) ) ;
#44176 = CARTESIAN_POINT ( 'NONE',  ( 154.0998481207909379, 207.0352699179129559, -217.4206707551776105 ) ) ;
#44177 = AXIS2_PLACEMENT_3D ( 'NONE', #85905, #49471, #71739 ) ;
#44178 = CARTESIAN_POINT ( 'NONE',  ( -70.02980485779180242, -279.4838224125497845, -337.6918383107881709 ) ) ;
#44179 = CARTESIAN_POINT ( 'NONE',  ( 24.23470416219412371, -22.50377800736068323, -344.3197070345564725 ) ) ;
#44180 = CARTESIAN_POINT ( 'NONE',  ( 201.0615436985592908, 293.2992059325864034, -68.27523266910206701 ) ) ;
#44181 = TOROIDAL_SURFACE ( 'NONE', #45716, 1.000000000000000000, 0.5000000000000000000 ) ;
#44182 = CARTESIAN_POINT ( 'NONE',  ( -104.5239402591454478, -272.1392627428297146, -241.2647166030098163 ) ) ;
#44183 = CARTESIAN_POINT ( 'NONE',  ( 38.00904969897577956, -293.2544328439536230, -285.9107611931934798 ) ) ;
#44184 = CARTESIAN_POINT ( 'NONE',  ( 174.2662291550402074, 240.3192241394675079, -177.2675829000265537 ) ) ;
#44185 = AXIS2_PLACEMENT_3D ( 'NONE', #57439, #56024, #92450 ) ;
#44187 = CARTESIAN_POINT ( 'NONE',  ( -110.9219885117268234, -288.8695857362028505, -276.6783256055854281 ) ) ;
#44186 = CARTESIAN_POINT ( 'NONE',  ( -99.15862868464212454, -271.8401489300471781, -225.1959667016525373 ) ) ;
#44188 = CARTESIAN_POINT ( 'NONE',  ( -78.61717904793809453, -297.4744966252449103, -332.1257089985984408 ) ) ;
#44189 = CARTESIAN_POINT ( 'NONE',  ( 23.16536800631423532, -289.4446340011258485, -312.0982709022560471 ) ) ;
#44190 = ORIENTED_EDGE ( 'NONE', *, *, #5345, .T. ) ;
#44191 = CARTESIAN_POINT ( 'NONE',  ( -88.43984633436494391, -296.6887950310547808, -327.7193832130890883 ) ) ;
#44192 = CIRCLE ( 'NONE', #69889, 1.000000000000000888 ) ;
#44193 = CARTESIAN_POINT ( 'NONE',  ( 18.70493752357450035, -287.3795849803549913, -223.4719925560505658 ) ) ;
#44194 = CARTESIAN_POINT ( 'NONE',  ( -106.5583079042602037, -271.8975530742450246, -237.3375852092785863 ) ) ;
#44195 = CARTESIAN_POINT ( 'NONE',  ( 23.05111624384964841, -294.9918123902675688, -317.8887209517366159 ) ) ;
#44196 = CARTESIAN_POINT ( 'NONE',  ( 39.54561512865520001, -294.0796059905883340, -273.1660521483253206 ) ) ;
#44197 = CARTESIAN_POINT ( 'NONE',  ( -62.80271767970420171, -291.8779247651003743, -201.9452090889473368 ) ) ;
#44198 = EDGE_LOOP ( 'NONE', ( #30349, #79293 ) ) ;
#44199 = CARTESIAN_POINT ( 'NONE',  ( -70.78781701246508362, -275.5345701890504984, -202.6066239058280019 ) ) ;
#44200 = CARTESIAN_POINT ( 'NONE',  ( 36.49874880616503248, -274.6043469331105484, -290.7961831706880957 ) ) ;
#44201 = ORIENTED_EDGE ( 'NONE', *, *, #791, .F. ) ;
#44202 = CARTESIAN_POINT ( 'NONE',  ( -94.91157564584894146, -278.7519079637411323, -219.3196021724193088 ) ) ;
#44203 = CARTESIAN_POINT ( 'NONE',  ( 33.27602869215502324, -274.2333270949336566, -291.8426268657913738 ) ) ;
#44204 = CARTESIAN_POINT ( 'NONE',  ( -59.58245494610068249, -274.8370548186397286, -200.4540145010778929 ) ) ;
#44205 = CARTESIAN_POINT ( 'NONE',  ( -56.93606160809189021, -274.7345605476013475, -199.7428733336180358 ) ) ;
#44206 = CARTESIAN_POINT ( 'NONE',  ( -82.98948492906988861, -275.1976673495402679, -209.5477897017458133 ) ) ;
#44207 = CARTESIAN_POINT ( 'NONE',  ( 35.01380846795892410, -273.3004200898033105, -249.1289194178671949 ) ) ;
#44208 = CARTESIAN_POINT ( 'NONE',  ( -42.38849250033216975, -295.7688954099421608, -343.2886337433527615 ) ) ;
#44209 = CARTESIAN_POINT ( 'NONE',  ( 12.74272004544800296, -292.9120683986142808, -324.3468572826103582 ) ) ;
#44210 = FACE_OUTER_BOUND ( 'NONE', #32450, .T. ) ;
#44211 = CARTESIAN_POINT ( 'NONE',  ( 3.474174293229708166, -277.0116810888953296, -335.6433970705903675 ) ) ;
#44212 = CARTESIAN_POINT ( 'NONE',  ( -46.18088475194703335, -274.1035764587128938, -197.8982390742496023 ) ) ;
#44213 = CARTESIAN_POINT ( 'NONE',  ( -108.5632250512156247, -283.5951063048372589, -242.2744572681871773 ) ) ;
#44214 = CARTESIAN_POINT ( 'NONE',  ( -96.80805936358210317, -297.9236062943652996, -316.3369871953059942 ) ) ;
#44215 = CARTESIAN_POINT ( 'NONE',  ( 165.2494399300530290, 8.542400036368780647, 10.00000000000000000 ) ) ;
#44216 = CARTESIAN_POINT ( 'NONE',  ( -98.23581421593654284, -284.3110344478233174, -229.8085767988599741 ) ) ;
#44217 = CARTESIAN_POINT ( 'NONE',  ( -110.0428307851742034, -276.6106056074396520, -284.3033307366886220 ) ) ;
#44218 = CARTESIAN_POINT ( 'NONE',  ( -91.41303848245777885, -276.4150650546976067, -320.3518441923130808 ) ) ;
#44219 = CARTESIAN_POINT ( 'NONE',  ( -110.4719326398463863, -286.7667217879182999, -253.6621375893454058 ) ) ;
#44220 = CARTESIAN_POINT ( 'NONE',  ( 15.72331339533422678, -276.0290172102775159, -219.5802184918402986 ) ) ;
#44221 = LINE ( 'NONE', #38041, #27716 ) ;
#44222 = CARTESIAN_POINT ( 'NONE',  ( 23.84974165440123173, -273.3419448418790694, -224.9513407345810947 ) ) ;
#44223 = CARTESIAN_POINT ( 'NONE',  ( -94.52800328201561797, -281.2264783127059218, -221.5586059181094924 ) ) ;
#44224 = CARTESIAN_POINT ( 'NONE',  ( 204.6539576904058606, 300.0210572133868823, -59.00000000000003553 ) ) ;
#44225 = CARTESIAN_POINT ( 'NONE',  ( -64.06128927176088439, -287.6265035753560255, -199.6692269937903461 ) ) ;
#44226 = CARTESIAN_POINT ( 'NONE',  ( 154.9065949031762841, 18.65395765032815234, -9.525636664970921430 ) ) ;
#44227 = CARTESIAN_POINT ( 'NONE',  ( 15.23539413068917270, -290.7939003430067260, -216.8047613663628681 ) ) ;
#44228 = EDGE_CURVE ( 'NONE', #47701, #75524, #55639, .T. ) ;
#44229 = FACE_OUTER_BOUND ( 'NONE', #71699, .T. ) ;
#44230 = CARTESIAN_POINT ( 'NONE',  ( -82.17459559740092345, -296.2202369010653911, -212.1835314915800268 ) ) ;
#44231 = CARTESIAN_POINT ( 'NONE',  ( -75.59615210149343056, -289.6759379042433125, -206.6814448480564863 ) ) ;
#44232 = CARTESIAN_POINT ( 'NONE',  ( -107.3349855510151656, -256.5393008024622077, -313.9713749062190686 ) ) ;
#44233 = FACE_OUTER_BOUND ( 'NONE', #68617, .T. ) ;
#44234 = CARTESIAN_POINT ( 'NONE',  ( -101.7267520673037922, -288.4892405297173354, -311.4129121200614918 ) ) ;
#44235 = CARTESIAN_POINT ( 'NONE',  ( 16.42250400512222797, -283.8728382227190536, -320.9902921522305519 ) ) ;
#44236 = CARTESIAN_POINT ( 'NONE',  ( -110.7365007942342885, -283.0439403702375216, -250.4867607419369335 ) ) ;
#44237 = CARTESIAN_POINT ( 'NONE',  ( 16.26746647612966612, -283.6980103413923757, -320.8472754617042710 ) ) ;
#44238 = CARTESIAN_POINT ( 'NONE',  ( -96.04520858568972130, -284.7438653608107870, -314.0246018351343764 ) ) ;
#44239 = CARTESIAN_POINT ( 'NONE',  ( -109.9502291657798452, -292.2739538444660639, -290.5206893010515046 ) ) ;
#44240 = AXIS2_PLACEMENT_3D ( 'NONE', #23842, #89613, #22909 ) ;
#44241 = CARTESIAN_POINT ( 'NONE',  ( -31.26596745729547067, -274.4601643074283857, -193.6091292834974524 ) ) ;
#44242 = VECTOR ( 'NONE', #62643, 1000.000000000000000 ) ;
#44243 = CARTESIAN_POINT ( 'NONE',  ( 7.068035009423874193, -286.5329084905408763, -331.5573651096770504 ) ) ;
#44244 = CARTESIAN_POINT ( 'NONE',  ( 26.14456769441573414, -274.9768540199766562, -226.7660392318886977 ) ) ;
#44245 = CARTESIAN_POINT ( 'NONE',  ( 37.35404291076277161, -295.5369866900414877, -270.7437446896001347 ) ) ;
#44246 = CARTESIAN_POINT ( 'NONE',  ( -48.18343439339132317, -274.8200403470298738, -436.8002545823309219 ) ) ;
#44247 = CARTESIAN_POINT ( 'NONE',  ( -106.6662871844225293, -293.4805209788415823, -237.0123917617630980 ) ) ;
#44248 = CARTESIAN_POINT ( 'NONE',  ( -26.68772616763157046, -281.5987579708564112, -343.1295855098389893 ) ) ;
#44249 = VECTOR ( 'NONE', #73494, 1000.000000000000000 ) ;
#44250 = CARTESIAN_POINT ( 'NONE',  ( -108.9286662694375138, -276.2548504243796970, -293.4490655206435008 ) ) ;
#44251 = CARTESIAN_POINT ( 'NONE',  ( -94.55370034198027440, -271.7219805740683682, -219.8685959108111092 ) ) ;
#44252 = CARTESIAN_POINT ( 'NONE',  ( 7.636591263180227074, -275.7684751826718070, -328.0523955772432032 ) ) ;
#44253 = CIRCLE ( 'NONE', #42709, 10.55076157886938937 ) ;
#44254 = CARTESIAN_POINT ( 'NONE',  ( -68.10813376321992507, -293.1607865170478249, -203.3835721314831915 ) ) ;
#44255 = PRODUCT ( 'Pneumatic Power Actuating Cylinder', 'Pneumatic Power Actuating Cylinder', '', ( #76689 ) ) ;
#44256 = CARTESIAN_POINT ( 'NONE',  ( 11.07741701989542449, -293.6830193049062814, -215.3480533558231684 ) ) ;
#44257 = CARTESIAN_POINT ( 'NONE',  ( -110.1944039448576405, -286.4830971900316854, -257.2337614647697706 ) ) ;
#44258 = CARTESIAN_POINT ( 'NONE',  ( 10.73386698722642407, -294.1267657837903471, -210.9015922608761002 ) ) ;
#44259 = CARTESIAN_POINT ( 'NONE',  ( 39.01122901738659010, -294.9381259910376798, -275.9860984305571492 ) ) ;
#44260 = CARTESIAN_POINT ( 'NONE',  ( -92.19207784247504378, -295.6978372760135017, -318.5320227810769893 ) ) ;
#44261 = CARTESIAN_POINT ( 'NONE',  ( -56.55399730580961659, -291.2998115424617254, -342.9126154468874574 ) ) ;
#44262 = CARTESIAN_POINT ( 'NONE',  ( -98.04311187050015519, -284.0858361666709015, -317.7355690824039129 ) ) ;
#44263 = CARTESIAN_POINT ( 'NONE',  ( -112.3183849281744244, -270.8348142488693497, -259.1044052736238541 ) ) ;
#44264 = CARTESIAN_POINT ( 'NONE',  ( -99.34297766170321609, -284.9930855666974594, -224.6133253961504010 ) ) ;
#44265 = CARTESIAN_POINT ( 'NONE',  ( -81.77879077782938566, -279.6406875791032007, -330.3377115366125736 ) ) ;
#44266 = CARTESIAN_POINT ( 'NONE',  ( -109.0495640668344492, -283.5532556106758761, -254.6464188711234442 ) ) ;
#44267 = CARTESIAN_POINT ( 'NONE',  ( 15.26448937178230558, -286.3095632037154701, -323.8897361082658790 ) ) ;
#44268 = CARTESIAN_POINT ( 'NONE',  ( -107.3619393009930150, -277.0655587574885885, -241.4220166775552343 ) ) ;
#44269 = EDGE_CURVE ( 'NONE', #67382, #37492, #84074, .T. ) ;
#44270 = LINE ( 'NONE', #8299, #81687 ) ;
#44271 = CARTESIAN_POINT ( 'NONE',  ( -109.2524821411010549, -284.2309727311548500, -257.3745831739649361 ) ) ;
#44272 = CARTESIAN_POINT ( 'NONE',  ( 5.947164010663343880, -281.8301973971152847, -207.1623604055843941 ) ) ;
#44273 = CARTESIAN_POINT ( 'NONE',  ( -74.32451217551619038, -288.5902225194246284, -337.6449293966938967 ) ) ;
#44274 = CARTESIAN_POINT ( 'NONE',  ( -64.78770275756014030, -279.0046608303928792, -341.5023758337149502 ) ) ;
#44275 = EDGE_CURVE ( 'NONE', #4269, #69256, #34373, .T. ) ;
#44276 = CARTESIAN_POINT ( 'NONE',  ( -98.39967108264154660, -279.2491628226472358, -316.4827487892523550 ) ) ;
#44278 = ADVANCED_FACE ( 'NONE', ( #63278 ), #39117, .F. ) ;
#44277 = CARTESIAN_POINT ( 'NONE',  ( -9.245385095142074405, -280.2633230881125996, -202.9845858212300413 ) ) ;
#44279 = CARTESIAN_POINT ( 'NONE',  ( 10.52084277501579912, -276.6963827057916205, -213.0132279692040242 ) ) ;
#44280 = CARTESIAN_POINT ( 'NONE',  ( 38.35725277512000275, -293.7293203700261870, -284.5273437214487444 ) ) ;
#44281 = CARTESIAN_POINT ( 'NONE',  ( -31.77326406589785890, -287.0017718883546536, -344.8496958323131025 ) ) ;
#44282 = CARTESIAN_POINT ( 'NONE',  ( -81.48370377214789073, -293.0626865193349886, -208.2489297427242434 ) ) ;
#44283 = AXIS2_PLACEMENT_3D ( 'NONE', #10015, #30408, #31804 ) ;
#44284 = CARTESIAN_POINT ( 'NONE',  ( -66.18737576575108505, -294.3591806187856719, -337.7566153932162933 ) ) ;
#44285 = CARTESIAN_POINT ( 'NONE',  ( 30.60367693512107934, -293.5781292341820290, -297.2485209610801462 ) ) ;
#44286 = CARTESIAN_POINT ( 'NONE',  ( -98.11178808324184786, -292.2587806512038924, -223.5585752111180113 ) ) ;
#44287 = CARTESIAN_POINT ( 'NONE',  ( 30.43213151035883257, -282.5699360638055282, -297.7582056555559689 ) ) ;
#44288 = CARTESIAN_POINT ( 'NONE',  ( -113.3096713220419787, -271.7538298802033410, -258.9677402597746436 ) ) ;
#44289 = CARTESIAN_POINT ( 'NONE',  ( -48.84554408078385990, -289.8462754519599116, -346.4477091772499193 ) ) ;
#44290 = CARTESIAN_POINT ( 'NONE',  ( -67.41323597047463068, -281.5819763459932688, -339.9025316476034959 ) ) ;
#44291 = CARTESIAN_POINT ( 'NONE',  ( 31.67034875309768793, -288.3251596649110979, -304.5853281146143559 ) ) ;
#44292 = CARTESIAN_POINT ( 'NONE',  ( -91.53976564075794897, -285.5867395296721725, -221.3515810274289493 ) ) ;
#44293 = CARTESIAN_POINT ( 'NONE',  ( 202.9738562182569694, 295.9636489450776367, -54.00000000004089173 ) ) ;
#44294 = CARTESIAN_POINT ( 'NONE',  ( -72.20741897415064159, -195.2005351582145920, -358.5414825501330824 ) ) ;
#44295 = CARTESIAN_POINT ( 'NONE',  ( -47.44010110492147447, -155.2456545128756886, -361.2982599994518864 ) ) ;
#44296 = CARTESIAN_POINT ( 'NONE',  ( -91.40927597213088518, -278.4545472724033743, -221.0731988796577809 ) ) ;
#44297 = CARTESIAN_POINT ( 'NONE',  ( -91.20427172815162464, -276.7606101788438764, -320.1647378175440508 ) ) ;
#44298 = CARTESIAN_POINT ( 'NONE',  ( -10.35105033397390883, -274.0615003983485849, -198.2124598010597936 ) ) ;
#44299 = CARTESIAN_POINT ( 'NONE',  ( 86.02760830248789148, 81.15136696978881048, -299.6155979961977209 ) ) ;
#44300 = CARTESIAN_POINT ( 'NONE',  ( -111.1570698369404653, -277.3766041890256702, -250.5648273664892827 ) ) ;
#44301 = CARTESIAN_POINT ( 'NONE',  ( -2.884028679770540560, -280.6145789443700096, -336.5911121559167896 ) ) ;
#44302 = CARTESIAN_POINT ( 'NONE',  ( -37.66191096783632730, -296.8162085151935230, -346.3600199473525549 ) ) ;
#44303 = CARTESIAN_POINT ( 'NONE',  ( -1.231711286763641722, -293.0373959675957849, -206.8324032252917846 ) ) ;
#44304 = CARTESIAN_POINT ( 'NONE',  ( -60.81062250351171627, -274.6962675792217397, -197.2164631965916612 ) ) ;
#44305 = CARTESIAN_POINT ( 'NONE',  ( -37.28433474693761696, -287.7362434404299734, -343.8542481986509642 ) ) ;
#44306 = CARTESIAN_POINT ( 'NONE',  ( -35.83594424014573576, -298.5628754214549190, -193.4225339918467625 ) ) ;
#44307 = CARTESIAN_POINT ( 'NONE',  ( -109.3625686777309198, -296.5616392050403647, -282.2772624038217373 ) ) ;
#44308 = ORIENTED_EDGE ( 'NONE', *, *, #81073, .F. ) ;
#44309 = CARTESIAN_POINT ( 'NONE',  ( 196.7510731661265595, -141.7221692137691775, -21.50000000000000000 ) ) ;
#44310 = ADVANCED_FACE ( 'NONE', ( #42864 ), #32519, .T. ) ;
#44311 = CARTESIAN_POINT ( 'NONE',  ( -110.7698943111320915, -280.2444763586340741, -288.2369826619550395 ) ) ;
#44312 = AXIS2_PLACEMENT_3D ( 'NONE', #91971, #64080, #44468 ) ;
#44313 = CIRCLE ( 'NONE', #24719, 28.04691768583012035 ) ;
#44314 = CARTESIAN_POINT ( 'NONE',  ( -9.141089901701752396, -281.5094732023418942, -202.6931665065401944 ) ) ;
#44315 = CARTESIAN_POINT ( 'NONE',  ( -81.93327532074388841, -279.4108154737498921, -331.8880668207454505 ) ) ;
#44316 = CARTESIAN_POINT ( 'NONE',  ( -48.96589212619218756, -272.3813992028697726, -197.5386834195107895 ) ) ;
#44317 = DIRECTION ( 'NONE',  ( -0.9693563597868428694, -0.2456588035076310295, 1.704600374100243061E-15 ) ) ;
#44318 = CARTESIAN_POINT ( 'NONE',  ( 140.6539576904058606, 130.0000000000000568, 12.50000000000000000 ) ) ;
#44319 = CARTESIAN_POINT ( 'NONE',  ( -54.49484821393048861, -279.9923816359219586, -199.3528106552576276 ) ) ;
#44320 = VECTOR ( 'NONE', #21210, 1000.000000000000000 ) ;
#44321 = CARTESIAN_POINT ( 'NONE',  ( 38.33129238530805338, -276.1869474650199550, -256.9534359876311669 ) ) ;
#44322 = CARTESIAN_POINT ( 'NONE',  ( 31.20252124061569887, -277.9511857996409390, -300.8027073419864905 ) ) ;
#44323 = CARTESIAN_POINT ( 'NONE',  ( -38.55395293646709121, -275.6418077723151328, -346.7622746371741300 ) ) ;
#44324 = VERTEX_POINT ( 'NONE', #60709 ) ;
#44325 = CARTESIAN_POINT ( 'NONE',  ( 197.7225753183262782, 40.74748806490614328, 10.04280106464628020 ) ) ;
#44326 = CARTESIAN_POINT ( 'NONE',  ( -4.849709395424552483, -284.6063199712243090, -338.3655742620771321 ) ) ;
#44327 = AXIS2_PLACEMENT_3D ( 'NONE', #26044, #5696, #54929 ) ;
#44328 = CARTESIAN_POINT ( 'NONE',  ( -47.00569737939760273, -291.1234238793411464, -197.8407147582254879 ) ) ;
#44329 = CARTESIAN_POINT ( 'NONE',  ( 32.62273875463439055, -286.4908329654080035, -238.3222454954391765 ) ) ;
#44330 = CARTESIAN_POINT ( 'NONE',  ( -105.0492133949513800, -282.3952231223228750, -300.2553759303422112 ) ) ;
#44332 = CARTESIAN_POINT ( 'NONE',  ( 23.17627917975993412, -285.0368792986515700, -226.9280302573315851 ) ) ;
#44331 = CARTESIAN_POINT ( 'NONE',  ( -0.9764910023544955964, -281.1339448159719723, -334.3372579321289209 ) ) ;
#44333 = CARTESIAN_POINT ( 'NONE',  ( -62.45917585592964372, -280.9231657350135833, -201.3419456730977402 ) ) ;
#44334 = CARTESIAN_POINT ( 'NONE',  ( -88.77235587117522186, -271.3304146040374007, -215.7018676450574048 ) ) ;
#44335 = CARTESIAN_POINT ( 'NONE',  ( -89.90124104501845181, -282.1789037785655410, -325.6053554415149165 ) ) ;
#44336 = CARTESIAN_POINT ( 'NONE',  ( -32.12550206775134853, -296.9865349872839602, -345.1924212355330042 ) ) ;
#44337 = CIRCLE ( 'NONE', #85175, 2.000000000000007105 ) ;
#44338 = CARTESIAN_POINT ( 'NONE',  ( -103.3378633286069714, -279.0638564591805562, -302.2260956324977315 ) ) ;
#44339 = CARTESIAN_POINT ( 'NONE',  ( -111.3277351600586798, -286.3786482096307964, -283.9164505795901619 ) ) ;
#44340 = CARTESIAN_POINT ( 'NONE',  ( 219.8344101925596021, 35.72494958537217968, -9.000000000000001776 ) ) ;
#44341 = CARTESIAN_POINT ( 'NONE',  ( -53.11307774118312608, -293.7717778121119068, -196.4119133981878917 ) ) ;
#44342 = AXIS2_PLACEMENT_3D ( 'NONE', #68152, #61978, #75711 ) ;
#44343 = CARTESIAN_POINT ( 'NONE',  ( -2.973054411784074702, -274.5977860903446413, -337.0229274656924758 ) ) ;
#44344 = CARTESIAN_POINT ( 'NONE',  ( 22.27337497298141145, -287.4013077462379897, -318.8606999541798928 ) ) ;
#44345 = CARTESIAN_POINT ( 'NONE',  ( -5.680136884807626352, -290.8754869230110103, -203.6839558843439875 ) ) ;
#44346 = CARTESIAN_POINT ( 'NONE',  ( -37.82973210483599047, -275.7431786125061421, -343.8651869101385614 ) ) ;
#44347 = CARTESIAN_POINT ( 'NONE',  ( -80.89834370404440733, -293.7901378483425106, -330.4750454716466948 ) ) ;
#44348 = CARTESIAN_POINT ( 'NONE',  ( -86.26974549416443949, -292.6718098741879430, -215.4538438420588591 ) ) ;
#44349 = DIRECTION ( 'NONE',  ( 0.5370370370370424196, -2.395818010342801312E-14, -0.8435586647355799439 ) ) ;
#44350 = DIRECTION ( 'NONE',  ( 1.000000000000000000, 0.000000000000000000, 0.000000000000000000 ) ) ;
#44351 = CARTESIAN_POINT ( 'NONE',  ( -61.39157226653063759, -293.8386983675802639, -342.8339785763364489 ) ) ;
#44352 = CARTESIAN_POINT ( 'NONE',  ( 18.36683560309531416, -288.4696662351336158, -221.9565782860350964 ) ) ;
#44353 = CARTESIAN_POINT ( 'NONE',  ( -85.84870287679824230, -289.6312338776223783, -211.8031175765976855 ) ) ;
#44354 = CARTESIAN_POINT ( 'NONE',  ( 6.207821419030736365, -289.8735238183497245, -329.7442276092970701 ) ) ;
#44355 = CARTESIAN_POINT ( 'NONE',  ( 129.4467878515196162, -299.5541904835127980, -195.3611179825600175 ) ) ;
#44356 = CARTESIAN_POINT ( 'NONE',  ( -72.42733682808474782, -290.3320390541636584, -334.5608050893261520 ) ) ;
#44357 = DIRECTION ( 'NONE',  ( 0.5000000000000032196, -0.8660254037844368202, 0.000000000000000000 ) ) ;
#44358 = CARTESIAN_POINT ( 'NONE',  ( -59.89565118516785702, -290.5431459785781954, -343.5685493637126910 ) ) ;
#44359 = CARTESIAN_POINT ( 'NONE',  ( -110.4832104780518733, -276.8046467916510665, -252.1774413975929576 ) ) ;
#44360 = CARTESIAN_POINT ( 'NONE',  ( -7.549092803123564011, -280.7654470216926370, -199.3669287783266668 ) ) ;
#44361 = CARTESIAN_POINT ( 'NONE',  ( 6.175798002383604768, -280.2920882314238042, -206.8633097690626244 ) ) ;
#44362 = CARTESIAN_POINT ( 'NONE',  ( 33.27415416238365253, -285.8794511306149388, -295.6277317301095877 ) ) ;
#44363 = DIRECTION ( 'NONE',  ( -0.000000000000000000, -1.000000000000000000, -0.000000000000000000 ) ) ;
#44364 = CARTESIAN_POINT ( 'NONE',  ( -99.00666014600341214, -277.2573572768194481, -228.9383175334328939 ) ) ;
#44365 = CARTESIAN_POINT ( 'NONE',  ( -104.0181008197655217, -282.0962989754925161, -304.8148365035943357 ) ) ;
#44366 = CARTESIAN_POINT ( 'NONE',  ( -76.15439624828563581, -208.4761096198365351, -353.6627254251765180 ) ) ;
#44367 = CARTESIAN_POINT ( 'NONE',  ( -104.1769097210477213, -277.5132987597655756, -233.5404375194501654 ) ) ;
#44368 = CARTESIAN_POINT ( 'NONE',  ( -83.08045875909370181, -284.3630566759910607, -208.7363266263961350 ) ) ;
#44369 = CARTESIAN_POINT ( 'NONE',  ( -67.13259920691677962, -274.4541651701845240, -203.5259595818224057 ) ) ;
#44370 = CARTESIAN_POINT ( 'NONE',  ( -60.70833197001743287, -275.1802099290781598, -197.5556040499927519 ) ) ;
#44371 = CARTESIAN_POINT ( 'NONE',  ( 31.28017531377432547, -275.5531324580429100, -295.4705142078872768 ) ) ;
#44372 = CARTESIAN_POINT ( 'NONE',  ( -3.409625314792581907, -296.6043879041391165, -337.2605893837646249 ) ) ;
#44373 = CARTESIAN_POINT ( 'NONE',  ( -82.85093667304971632, -289.8223478022947575, -332.4731892214102800 ) ) ;
#44374 = CIRCLE ( 'NONE', #35337, 24.00000000000000355 ) ;
#44375 = CARTESIAN_POINT ( 'NONE',  ( 29.46037816190632697, -279.1660899202661312, -234.9394982464266945 ) ) ;
#44376 = CARTESIAN_POINT ( 'NONE',  ( -5.884994359699165400, -292.2876765261773926, -200.0654259477474852 ) ) ;
#44377 = ADVANCED_FACE ( 'NONE', ( #89086 ), #67353, .T. ) ;
#44378 = CARTESIAN_POINT ( 'NONE',  ( -76.00309409725149123, -288.6412777343273888, -332.5600332811768567 ) ) ;
#44379 = CARTESIAN_POINT ( 'NONE',  ( 37.44861756189148139, -291.4800287172817548, -264.7567423375353997 ) ) ;
#44380 = ORIENTED_EDGE ( 'NONE', *, *, #73898, .T. ) ;
#44381 = CARTESIAN_POINT ( 'NONE',  ( 0.000000000000000000, 0.000000000000000000, 10.00000000000000000 ) ) ;
#44382 = CARTESIAN_POINT ( 'NONE',  ( -109.0003189781140378, -289.8711513757135663, -284.6740238976378237 ) ) ;
#44383 = DIRECTION ( 'NONE',  ( -0.000000000000000000, -1.000000000000000000, -0.000000000000000000 ) ) ;
#44384 = CARTESIAN_POINT ( 'NONE',  ( 26.93417499958815498, -287.9403251794864218, -228.3916994810386996 ) ) ;
#44385 = CARTESIAN_POINT ( 'NONE',  ( 17.40634833298267736, -296.6948066931273047, -313.9805196606274080 ) ) ;
#44386 = CARTESIAN_POINT ( 'NONE',  ( 24.68905125968658254, -293.2132097090457137, -315.6049992319474882 ) ) ;
#44387 = ADVANCED_FACE ( 'NONE', ( #30421 ), #37491, .T. ) ;
#44388 = CARTESIAN_POINT ( 'NONE',  ( -5.644450957155282111, -283.9590942759782024, -339.9928827841347925 ) ) ;
#44389 = CARTESIAN_POINT ( 'NONE',  ( -67.54575944813693411, -285.4778171993384603, -203.9027490203200443 ) ) ;
#44390 = CIRCLE ( 'NONE', #26216, 204.9779373800640485 ) ;
#44391 = CARTESIAN_POINT ( 'NONE',  ( 20.42038450697154062, -277.5041895992366108, -315.8212963961043442 ) ) ;
#44392 = CARTESIAN_POINT ( 'NONE',  ( 20.08265250920577927, -292.2337960397535994, -318.0506402110909221 ) ) ;
#44393 = CARTESIAN_POINT ( 'NONE',  ( -65.95386005564168386, -272.4641321515136383, -202.7706244956038404 ) ) ;
#44394 = ORIENTED_EDGE ( 'NONE', *, *, #6688, .F. ) ;
#44395 = CARTESIAN_POINT ( 'NONE',  ( 152.4536156746142410, 275.0000000000000568, 14.50000000000000000 ) ) ;
#44396 = CARTESIAN_POINT ( 'NONE',  ( 11.18169288377148085, -294.0680743689401879, -330.1895312541307135 ) ) ;
#44397 = CARTESIAN_POINT ( 'NONE',  ( -38.67474428239044926, -287.9554958543614589, -195.9203231659482469 ) ) ;
#44398 = CARTESIAN_POINT ( 'NONE',  ( -100.5039200552215135, -298.2086314536894065, -226.8406034725549034 ) ) ;
#44399 = CIRCLE ( 'NONE', #8181, 20.00000000000000355 ) ;
#44400 = CARTESIAN_POINT ( 'NONE',  ( 25.03338392898101716, -287.6790611060463334, -232.2397124875878660 ) ) ;
#44401 = CARTESIAN_POINT ( 'NONE',  ( -93.17113290953955129, -276.8886407447756710, -323.1241681779562782 ) ) ;
#44402 = CARTESIAN_POINT ( 'NONE',  ( -22.10961441625129353, -295.5133499431731252, -345.7354926144147385 ) ) ;
#44403 = CARTESIAN_POINT ( 'NONE',  ( 18.69446659952220102, -286.3962902350400554, -321.3731161338902211 ) ) ;
#44404 = CARTESIAN_POINT ( 'NONE',  ( -11.06043674947947153, -295.0521836527204869, -342.7712458051398130 ) ) ;
#44405 = CARTESIAN_POINT ( 'NONE',  ( -22.74054715544054872, -292.5774930038245429, -198.8146727979816717 ) ) ;
#44406 = FACE_OUTER_BOUND ( 'NONE', #29919, .T. ) ;
#44407 = CARTESIAN_POINT ( 'NONE',  ( -26.41588298435790350, -486.4924983417995463, -472.6442049081569508 ) ) ;
#44408 = CARTESIAN_POINT ( 'NONE',  ( 207.8064396648212551, 36.74001737686529623, 13.57731244650625690 ) ) ;
#44409 = CARTESIAN_POINT ( 'NONE',  ( 24.96766530141969298, -288.4837852136734000, -226.2903202452731080 ) ) ;
#44410 = CARTESIAN_POINT ( 'NONE',  ( -111.2869819898779866, -287.6237833571632905, -305.9350535429201159 ) ) ;
#44411 = EDGE_LOOP ( 'NONE', ( #35252, #53760, #93464, #27538 ) ) ;
#44412 = CARTESIAN_POINT ( 'NONE',  ( -73.71010316927231543, -278.9309456273461478, -202.5918370350309772 ) ) ;
#44413 = CARTESIAN_POINT ( 'NONE',  ( 21.09200081758644885, -282.9079775485607229, -223.6114546128249856 ) ) ;
#44414 = CARTESIAN_POINT ( 'NONE',  ( -37.53648651393305613, -140.8450507183935372, -363.5632225393354133 ) ) ;
#44415 = CARTESIAN_POINT ( 'NONE',  ( -112.9019556255240531, -283.2745553166539594, -258.6437639470820500 ) ) ;
#44416 = CARTESIAN_POINT ( 'NONE',  ( 4.402289580088711851, -286.5645569975753801, -332.0572899117436236 ) ) ;
#44417 = CARTESIAN_POINT ( 'NONE',  ( 4.166324136486196927, -276.4651173473556582, -206.9160032604663968 ) ) ;
#44418 = CIRCLE ( 'NONE', #86729, 35.00000000000003553 ) ;
#44419 = CARTESIAN_POINT ( 'NONE',  ( -96.93656144539038166, -297.6341838151465709, -228.0948081563197150 ) ) ;
#44420 = EDGE_LOOP ( 'NONE', ( #31838, #92742, #32108, #13903 ) ) ;
#44421 = CARTESIAN_POINT ( 'NONE',  ( -47.88019754310063547, -293.8736607139437638, -343.1463937689038062 ) ) ;
#44422 = CARTESIAN_POINT ( 'NONE',  ( -100.1704968793952730, -279.7910095877339245, -226.0231536011464186 ) ) ;
#44423 = CARTESIAN_POINT ( 'NONE',  ( 19.18159363966009678, -276.2064553192546441, -316.5773227746499288 ) ) ;
#44424 = CARTESIAN_POINT ( 'NONE',  ( -58.05141491136269138, -274.8704876454293640, -196.4641886117378533 ) ) ;
#44425 = CARTESIAN_POINT ( 'NONE',  ( -95.92201054560364071, -276.8027795264148381, -319.8772475206681065 ) ) ;
#44426 = DIRECTION ( 'NONE',  ( 0.6522365350567651543, -0.2069344830099842103, -0.7292226148979034095 ) ) ;
#44427 = CARTESIAN_POINT ( 'NONE',  ( -99.00777544970651434, -275.9721055732606487, -313.1379650736610643 ) ) ;
#44428 = CARTESIAN_POINT ( 'NONE',  ( -96.89858719006657850, -298.6238831381976411, -222.4906312597882163 ) ) ;
#44429 = CARTESIAN_POINT ( 'NONE',  ( 21.27581636871892101, -277.4090924074130839, -223.5744983911110353 ) ) ;
#44430 = CARTESIAN_POINT ( 'NONE',  ( -104.5266604826868644, -260.4492150524036447, -315.3738353148558531 ) ) ;
#44431 = CARTESIAN_POINT ( 'NONE',  ( -72.53443448135334393, -286.6543576803468341, -206.0374509878675156 ) ) ;
#44432 = CARTESIAN_POINT ( 'NONE',  ( -111.2284843650547970, -286.0867631514931873, -288.1564007223932435 ) ) ;
#44433 = CARTESIAN_POINT ( 'NONE',  ( -11.97884976289537384, -285.7397812019814864, -201.8000613284982876 ) ) ;
#44434 = CARTESIAN_POINT ( 'NONE',  ( -95.09165902370692436, -276.3099652982359657, -316.3310943708975742 ) ) ;
#44435 = CARTESIAN_POINT ( 'NONE',  ( -110.1449122680498647, -286.6008033708632752, -255.8505085892934119 ) ) ;
#44436 = CARTESIAN_POINT ( 'NONE',  ( -107.8852716038370119, -277.3115757372997905, -249.0465155607871282 ) ) ;
#44437 = CARTESIAN_POINT ( 'NONE',  ( 31.55697813618587588, -276.9658574173840293, -295.5526353879783983 ) ) ;
#44438 = CARTESIAN_POINT ( 'NONE',  ( 199.8304385318961351, 66.96291204605094549, -8.111402028797257913 ) ) ;
#44439 = CARTESIAN_POINT ( 'NONE',  ( -105.4758991599336042, -273.3983116452837976, -243.8450373613339082 ) ) ;
#44440 = CARTESIAN_POINT ( 'NONE',  ( 23.61295256125125519, -281.7293639233248541, -223.5561990381359578 ) ) ;
#44441 = CARTESIAN_POINT ( 'NONE',  ( 39.55849578082804641, -282.0748664622238948, -272.7873851220412007 ) ) ;
#44442 = VERTEX_POINT ( 'NONE', #74917 ) ;
#44443 = ORIENTED_EDGE ( 'NONE', *, *, #56330, .T. ) ;
#44444 = CARTESIAN_POINT ( 'NONE',  ( 196.1511317126956158, 42.06348744092182557, 13.68688499713156403 ) ) ;
#44445 = CARTESIAN_POINT ( 'NONE',  ( 31.74836090790034859, -289.8162046137148309, -301.4556342819422525 ) ) ;
#44446 = CARTESIAN_POINT ( 'NONE',  ( -97.94727184224944949, -289.8643234001185647, -223.6466403493475354 ) ) ;
#44447 = CARTESIAN_POINT ( 'NONE',  ( -101.6140365460790207, -295.2733017846820758, -305.3134926926056210 ) ) ;
#44448 = CARTESIAN_POINT ( 'NONE',  ( 1.655572977045638883, -291.9074594633247557, -204.0241312106408600 ) ) ;
#44449 = CARTESIAN_POINT ( 'NONE',  ( 31.12220547957002381, -286.3950449812379588, -297.7640427143419402 ) ) ;
#44450 = CARTESIAN_POINT ( 'NONE',  ( -44.07600371577404275, -287.1701884124922799, -197.2736384802797147 ) ) ;
#44451 = CARTESIAN_POINT ( 'NONE',  ( 10.64812456238590066, -296.9090924074130271, -330.4860931364851808 ) ) ;
#44452 = AXIS2_PLACEMENT_3D ( 'NONE', #22006, #88235, #30489 ) ;
#44453 = CARTESIAN_POINT ( 'NONE',  ( 32.19777683865432039, -289.9200825905789429, -298.5933697598667322 ) ) ;
#44454 = CARTESIAN_POINT ( 'NONE',  ( -95.00151520645839298, -287.8870459135698070, -318.6032244064245447 ) ) ;
#44455 = CARTESIAN_POINT ( 'NONE',  ( -70.31014610554780120, -284.4389455149029118, -335.7700183032857808 ) ) ;
#44456 = CARTESIAN_POINT ( 'NONE',  ( -91.50904514648496502, -293.2837682530359871, -218.1724824709413326 ) ) ;
#44457 = DIRECTION ( 'NONE',  ( -0.000000000000000000, 1.000000000000000000, -0.000000000000000000 ) ) ;
#44458 =( REPRESENTATION_RELATIONSHIP ('NONE','NONE', #78428, #61554 ) REPRESENTATION_RELATIONSHIP_WITH_TRANSFORMATION ( #78109 )SHAPE_REPRESENTATION_RELATIONSHIP( ) );
#44459 = DIRECTION ( 'NONE',  ( -0.000000000000000000, -0.000000000000000000, -1.000000000000000000 ) ) ;
#44460 = CIRCLE ( 'NONE', #12724, 4.000000000000003553 ) ;
#44461 = CARTESIAN_POINT ( 'NONE',  ( -35.53988309452446970, -299.9946885707460638, -194.8005259585299882 ) ) ;
#44462 = CARTESIAN_POINT ( 'NONE',  ( -34.29639471325485545, -279.2885446299473529, -197.2504767746720518 ) ) ;
#44463 = CARTESIAN_POINT ( 'NONE',  ( -108.0680676132336515, -282.2269498391435718, -295.4715142238394492 ) ) ;
#44464 = CARTESIAN_POINT ( 'NONE',  ( 39.49491924258473574, -292.7128737016991522, -267.4529351068531469 ) ) ;
#44465 = CARTESIAN_POINT ( 'NONE',  ( -81.66010341218630231, -271.6797174297837500, -211.0190601774547190 ) ) ;
#44466 = CARTESIAN_POINT ( 'NONE',  ( 1.604380613884477835, -274.6074031863089431, -333.8607555102322522 ) ) ;
#44467 = CARTESIAN_POINT ( 'NONE',  ( -47.35641305353401265, -299.2375501049691593, -197.5019437679379166 ) ) ;
#44468 = DIRECTION ( 'NONE',  ( 0.000000000000000000, 0.000000000000000000, 1.000000000000000000 ) ) ;
#44469 = CARTESIAN_POINT ( 'NONE',  ( -90.02586537163300306, -294.0236367781329818, -325.1907983128676847 ) ) ;
#44470 = CIRCLE ( 'NONE', #698, 5.568361562975243650 ) ;
#44471 = CARTESIAN_POINT ( 'NONE',  ( 35.42337767063744280, -295.1254929474005735, -281.6757419492871009 ) ) ;
#44472 = CARTESIAN_POINT ( 'NONE',  ( 188.7399167944524550, 8.542400036368780647, 13.00000000000000178 ) ) ;
#44473 = CARTESIAN_POINT ( 'NONE',  ( -34.28423557078182426, -295.8155653478509635, -343.4586804439903744 ) ) ;
#44474 = DIRECTION ( 'NONE',  ( 3.961265963009670520E-15, 7.202301750926674102E-15, -1.000000000000000000 ) ) ;
#44476 = CARTESIAN_POINT ( 'NONE',  ( -101.4673155125522044, -296.0760051309009100, -305.2452899171625518 ) ) ;
#44475 = CARTESIAN_POINT ( 'NONE',  ( -35.16982601332965430, -284.0993750176975823, -195.0243565101894774 ) ) ;
#44477 = AXIS2_PLACEMENT_3D ( 'NONE', #53060, #75318, #3338 ) ;
#44478 = CARTESIAN_POINT ( 'NONE',  ( -81.56155594951749777, -283.6353463407463096, -333.4625159746628924 ) ) ;
#44479 = CARTESIAN_POINT ( 'NONE',  ( 36.46433779166198974, -283.6793481051777235, -286.6068446237343892 ) ) ;
#44480 = CARTESIAN_POINT ( 'NONE',  ( 12.39893236550466149, -288.0477611921755852, -329.1115543262658889 ) ) ;
#44481 = CARTESIAN_POINT ( 'NONE',  ( 37.36665883640003472, -291.4857647391988849, -265.2150234997680514 ) ) ;
#44482 = CARTESIAN_POINT ( 'NONE',  ( -114.2756510520024023, -277.9211900629985053, -268.7281209873597163 ) ) ;
#44483 = CARTESIAN_POINT ( 'NONE',  ( -106.6662871844225293, -275.6237833571632905, -303.7098442033569654 ) ) ;
#44484 = CARTESIAN_POINT ( 'NONE',  ( -48.18343439339133027, -253.0058770677770497, -490.0359438847364686 ) ) ;
#44485 = VECTOR ( 'NONE', #73522, 1000.000000000000000 ) ;
#44486 = CARTESIAN_POINT ( 'NONE',  ( 35.84656591180441865, -286.4280063342276890, -276.5299010496783012 ) ) ;
#44487 = CARTESIAN_POINT ( 'NONE',  ( -107.4543787818009690, -289.0728505083510527, -301.5675758362905299 ) ) ;
#44488 = PLANE ( 'NONE',  #92941 ) ;
#44489 = CARTESIAN_POINT ( 'NONE',  ( -88.55011191044064844, -280.7756261154848403, -213.6486426861320638 ) ) ;
#44491 = CARTESIAN_POINT ( 'NONE',  ( 30.35254270268198695, -281.5854002178119799, -297.7395214106401227 ) ) ;
#44490 = CARTESIAN_POINT ( 'NONE',  ( -2.745557503210954486, -292.6171428844522211, -337.3052269194305381 ) ) ;
#44492 = CARTESIAN_POINT ( 'NONE',  ( -33.43271445983832280, -295.1709301181975889, -347.2749514855799475 ) ) ;
#44493 = CARTESIAN_POINT ( 'NONE',  ( 30.14680484349281286, -285.1864433826016239, -236.3814786101340246 ) ) ;
#44494 = CARTESIAN_POINT ( 'NONE',  ( -107.8476544276615670, -280.2189563632457521, -296.0845840191279308 ) ) ;
#44495 = ADVANCED_FACE ( 'NONE', ( #73969 ), #17146, .F. ) ;
#44496 = ORIENTED_EDGE ( 'NONE', *, *, #26979, .T. ) ;
#44497 = CARTESIAN_POINT ( 'NONE',  ( 202.4403316624510580, 63.53362652955771495, -6.999999999998341771 ) ) ;
#44498 = CARTESIAN_POINT ( 'NONE',  ( -108.6533021207399941, -295.8503018677580485, -286.2558926937859951 ) ) ;
#44499 = CARTESIAN_POINT ( 'NONE',  ( 194.5881128153457098, 0.000000000000000000, 21.50000000000000000 ) ) ;
#44500 = CARTESIAN_POINT ( 'NONE',  ( -69.85430415644619018, -277.1237833571632905, -202.7746430608542312 ) ) ;
#44501 = CARTESIAN_POINT ( 'NONE',  ( -68.76864842908555886, -272.8466325309435092, -200.2289550064433001 ) ) ;
#44502 = CARTESIAN_POINT ( 'NONE',  ( -105.1138348963155096, -290.0207650408347035, -297.6249682552959825 ) ) ;
#44503 = CARTESIAN_POINT ( 'NONE',  ( -108.6483298486302971, -280.3161605161693046, -251.7084807321710116 ) ) ;
#44504 = CARTESIAN_POINT ( 'NONE',  ( -3.758639256968665521, -276.1029865031083546, -204.6307367993258310 ) ) ;
#44505 = CARTESIAN_POINT ( 'NONE',  ( -8.324456075631273322, -284.2787723166438809, -340.8758594970555578 ) ) ;
#44506 = CARTESIAN_POINT ( 'NONE',  ( 34.96087503310251066, -280.1813885121293310, -257.7330488293075632 ) ) ;
#44507 = CARTESIAN_POINT ( 'NONE',  ( -5.402396971767837286, -278.6321329417295942, -338.2345440956249263 ) ) ;
#44508 = EDGE_LOOP ( 'NONE', ( #64959, #82454 ) ) ;
#44509 = CARTESIAN_POINT ( 'NONE',  ( -44.04064290410936167, -273.8031295698629606, -193.5997647266876811 ) ) ;
#44510 = CARTESIAN_POINT ( 'NONE',  ( -84.76485457830875703, -293.3126168828366644, -212.9820397666364897 ) ) ;
#44511 = DIRECTION ( 'NONE',  ( -0.000000000000000000, 1.000000000000000000, 0.000000000000000000 ) ) ;
#44512 = ADVANCED_FACE ( 'NONE', ( #24714 ), #46469, .T. ) ;
#44513 = CARTESIAN_POINT ( 'NONE',  ( 113.5000000000000568, -218.8335761803644743, -447.4016117689005796 ) ) ;
#44514 = CARTESIAN_POINT ( 'NONE',  ( -8.874483681549044434, -292.8234407389844591, -340.6300956179244963 ) ) ;
#44515 = CARTESIAN_POINT ( 'NONE',  ( -34.03162291124731809, -273.6025578906466080, -197.3745998397894823 ) ) ;
#44516 = DIRECTION ( 'NONE',  ( 0.000000000000000000, 1.000000000000000000, 0.000000000000000000 ) ) ;
#44517 = ADVANCED_FACE ( 'NONE', ( #3876 ), #84324, .F. ) ;
#44518 = CARTESIAN_POINT ( 'NONE',  ( -40.62216451258591832, -293.5317462503446677, -194.1119325345804043 ) ) ;
#44520 = CARTESIAN_POINT ( 'NONE',  ( -14.00211361193672488, -293.5533089795849833, -197.3446760585814559 ) ) ;
#44519 = CARTESIAN_POINT ( 'NONE',  ( -95.99890600148557951, -281.6948066931273615, -223.6242672951989618 ) ) ;
#44521 = CARTESIAN_POINT ( 'NONE',  ( 31.64215255283919248, -289.1710774764609937, -241.2226099136157984 ) ) ;
#44522 = CARTESIAN_POINT ( 'NONE',  ( 37.47637329432973985, -273.5325373212593831, -268.8497236634133287 ) ) ;
#44523 = CARTESIAN_POINT ( 'NONE',  ( 8.485773122936732804, -278.3396286921513365, -329.0881921755071744 ) ) ;
#44524 = CARTESIAN_POINT ( 'NONE',  ( -15.18712578377499867, -292.8430217246077518, -341.4821248836370273 ) ) ;
#44525 = CARTESIAN_POINT ( 'NONE',  ( -97.60846626097666956, -281.0348212588008323, -224.4245933156176989 ) ) ;
#44526 = VERTEX_POINT ( 'NONE', #63066 ) ;
#44527 = CARTESIAN_POINT ( 'NONE',  ( -99.05117690618099857, -283.6784212986337366, -309.4945871985907502 ) ) ;
#44528 = CARTESIAN_POINT ( 'NONE',  ( -99.18677729593699155, -280.2367619352089605, -224.9883271627897159 ) ) ;
#44529 = CARTESIAN_POINT ( 'NONE',  ( -21.82150746302388455, -281.6524179623428381, -345.3753322163662460 ) ) ;
#44530 = CIRCLE ( 'NONE', #24879, 25.00000000000000355 ) ;
#44531 = CARTESIAN_POINT ( 'NONE',  ( -4.085903519213418988, -277.5655622886697529, -339.5627995235928438 ) ) ;
#44532 = CARTESIAN_POINT ( 'NONE',  ( 33.54740286788948112, -277.4353878861709859, -298.7426974221996261 ) ) ;
#44533 = CARTESIAN_POINT ( 'NONE',  ( 7.450504543161046378, -284.9090924074130839, -326.4764044574609443 ) ) ;
#44534 = ORIENTED_EDGE ( 'NONE', *, *, #11260, .F. ) ;
#44535 = ORIENTED_EDGE ( 'NONE', *, *, #57901, .T. ) ;
#44536 = CARTESIAN_POINT ( 'NONE',  ( -95.21197722736944513, -275.2080839337588145, -222.8957426162362196 ) ) ;
#44537 = CARTESIAN_POINT ( 'NONE',  ( -97.02097982478332483, -292.2251515782290880, -227.7004791358921523 ) ) ;
#44538 = CARTESIAN_POINT ( 'NONE',  ( -111.5997290360169956, -276.6765306270784777, -262.2784132876439003 ) ) ;
#44539 = CARTESIAN_POINT ( 'NONE',  ( -48.69515949728628357, -290.9548249376470608, -345.5480509916260985 ) ) ;
#44540 = CARTESIAN_POINT ( 'NONE',  ( -62.82850568139382119, -291.0599634610347266, -201.8460436494954138 ) ) ;
#44541 = CARTESIAN_POINT ( 'NONE',  ( -14.97613394031227685, -288.2777900849700359, -344.0327749128680921 ) ) ;
#44542 = LINE ( 'NONE', #73445, #18871 ) ;
#44543 = CARTESIAN_POINT ( 'NONE',  ( -98.20353022599101678, -282.3762547052830882, -312.1908215390862438 ) ) ;
#44544 = CARTESIAN_POINT ( 'NONE',  ( -108.9495300949364918, -292.6668875430676735, -250.7860274442684840 ) ) ;
#44545 = CARTESIAN_POINT ( 'NONE',  ( -60.17525078554039908, -284.2305803015421475, -200.2944588943720134 ) ) ;
#44546 = CARTESIAN_POINT ( 'NONE',  ( 25.54968415209746269, -282.3462423541583348, -232.2373147414432424 ) ) ;
#44547 = CARTESIAN_POINT ( 'NONE',  ( -74.30347451398851888, -290.4724224527875549, -337.6564888963608837 ) ) ;
#44548 = CARTESIAN_POINT ( 'NONE',  ( -41.06058262325050379, -280.4964356004866772, -197.3942874719873259 ) ) ;
#44549 = CARTESIAN_POINT ( 'NONE',  ( -27.88282330290596533, -290.9644974789804905, -194.2910214177152284 ) ) ;
#44550 = CARTESIAN_POINT ( 'NONE',  ( 39.54105710971416698, -288.3697402850789331, -271.5385890454601849 ) ) ;
#44551 = CARTESIAN_POINT ( 'NONE',  ( 3.153082315061669139, -289.0163810657550130, -335.8430311126187462 ) ) ;
#44552 = CARTESIAN_POINT ( 'NONE',  ( -5.800571593454897368, -286.6454022889337239, -204.5130177428107174 ) ) ;
#44553 = ORIENTED_EDGE ( 'NONE', *, *, #39969, .T. ) ;
#44554 = DIRECTION ( 'NONE',  ( 0.000000000000000000, 0.000000000000000000, -1.000000000000000000 ) ) ;
#44555 = CARTESIAN_POINT ( 'NONE',  ( -5.007819722550730823, -296.4914400188387162, -338.8941561392257995 ) ) ;
#44556 = CARTESIAN_POINT ( 'NONE',  ( -88.28959555612692611, -294.4327322491347445, -327.5076521907544134 ) ) ;
#44557 = CARTESIAN_POINT ( 'NONE',  ( -18.96945557316667674, -275.8685172346219474, -341.2544821108269275 ) ) ;
#44558 = CARTESIAN_POINT ( 'NONE',  ( -102.2259323693968014, -296.4424229146545144, -229.0894667808400982 ) ) ;
#44559 = CARTESIAN_POINT ( 'NONE',  ( 23.49451730750386247, -292.6063665550602195, -312.0395319126256481 ) ) ;
#44560 = CARTESIAN_POINT ( 'NONE',  ( -109.4594346524990698, -295.0085612084535569, -253.7176092238774174 ) ) ;
#44561 = CARTESIAN_POINT ( 'NONE',  ( 34.87109307281083659, -294.5840231894339922, -257.1595545445645143 ) ) ;
#44562 = CARTESIAN_POINT ( 'NONE',  ( 29.77856839255682786, -295.0267540612816219, -299.8415458359543209 ) ) ;
#44563 = DIRECTION ( 'NONE',  ( 0.6056179655966478226, -0.7957555401921982963, 0.000000000000000000 ) ) ;
#44564 = CARTESIAN_POINT ( 'NONE',  ( -37.70627606878536398, -293.0565156026447085, -345.5396714588636655 ) ) ;
#44565 = CARTESIAN_POINT ( 'NONE',  ( 82.12347693879148380, -301.5478687382300222, -195.3203844934047311 ) ) ;
#44566 = CARTESIAN_POINT ( 'NONE',  ( -66.41143275288175118, -290.3835155073352325, -337.6340440660973741 ) ) ;
#44567 = CARTESIAN_POINT ( 'NONE',  ( -73.30912404235306212, -295.8766123599677940, -333.9097757478731978 ) ) ;
#44568 = CARTESIAN_POINT ( 'NONE',  ( -108.1817001848615405, -280.1986913336840530, -296.2060549065487294 ) ) ;
#44569 = CARTESIAN_POINT ( 'NONE',  ( -68.45652880106044336, -278.3366787867803396, -200.4528655925653595 ) ) ;
#44570 = ORIENTED_EDGE ( 'NONE', *, *, #1420, .F. ) ;
#44571 = CARTESIAN_POINT ( 'NONE',  ( -109.0685185281854643, -272.2540321755280388, -242.4913780628532152 ) ) ;
#44572 = CARTESIAN_POINT ( 'NONE',  ( 23.30051269408180659, -279.0406177156627336, -227.1889484361012705 ) ) ;
#44573 = CARTESIAN_POINT ( 'NONE',  ( -77.05797299808246237, -277.9296433904203241, -205.2688336345278799 ) ) ;
#44574 = CARTESIAN_POINT ( 'NONE',  ( -104.5252511496972545, -276.9975555567187939, -236.5347552008784362 ) ) ;
#44575 = EDGE_CURVE ( 'NONE', #9328, #2619, #29947, .T. ) ;
#44576 = CARTESIAN_POINT ( 'NONE',  ( -102.5441727504278617, -271.5887871775647113, -236.1331745616857063 ) ) ;
#44577 = CARTESIAN_POINT ( 'NONE',  ( -112.1889503641107950, -274.6232853802811746, -264.8338837743303316 ) ) ;
#44578 = CARTESIAN_POINT ( 'NONE',  ( 193.5162140859150668, 250.0000000000000568, 17.51463615629760895 ) ) ;
#44579 = CARTESIAN_POINT ( 'NONE',  ( -112.1831259452708736, -288.4544794835377388, -279.5775346463707933 ) ) ;
#44580 = CARTESIAN_POINT ( 'NONE',  ( -74.42731838132610278, -289.5313224861060348, -337.8569607667662353 ) ) ;
#44581 = CARTESIAN_POINT ( 'NONE',  ( -2.182146302530975746, -276.5166566984440806, -203.9244247787239601 ) ) ;
#44582 = CARTESIAN_POINT ( 'NONE',  ( -35.05284281979317029, -296.0807104606674329, -195.5285584408348711 ) ) ;
#44583 = CARTESIAN_POINT ( 'NONE',  ( -109.8215417628479287, -284.0718311411624200, -244.8497209834165460 ) ) ;
#44584 = FACE_OUTER_BOUND ( 'NONE', #20592, .T. ) ;
#44585 = CARTESIAN_POINT ( 'NONE',  ( -4.537303454627476640, -280.6198067724292287, -337.8204163905774067 ) ) ;
#44586 = CARTESIAN_POINT ( 'NONE',  ( 199.1087447750284980, 64.61450673763175701, -10.46317447812566570 ) ) ;
#44587 = CARTESIAN_POINT ( 'NONE',  ( -33.47223843021657785, -290.8968293585060110, -197.0535528786665225 ) ) ;
#44588 = CARTESIAN_POINT ( 'NONE',  ( -41.36660575354350300, -284.1405522321418857, -196.2223962516110589 ) ) ;
#44589 = CARTESIAN_POINT ( 'NONE',  ( 195.5825507613122056, 25.45032227799513791, 14.51846093667993465 ) ) ;
#44590 = CARTESIAN_POINT ( 'NONE',  ( 128.9960186029002500, -299.5541904835127980, -201.1130027942871266 ) ) ;
#44591 = CARTESIAN_POINT ( 'NONE',  ( -27.82807646614444863, -290.1726618137871014, -195.9148144460450283 ) ) ;
#44592 = CARTESIAN_POINT ( 'NONE',  ( -95.89544874472140634, -279.5271080104831753, -315.2821480264194633 ) ) ;
#44593 = CARTESIAN_POINT ( 'NONE',  ( 4.342564639707441998, -283.7089005723038326, -334.6922459569185548 ) ) ;
#44595 = CARTESIAN_POINT ( 'NONE',  ( -108.9289666493128976, -284.7406883148457837, -256.0690477330068688 ) ) ;
#44594 = CARTESIAN_POINT ( 'NONE',  ( -54.97342816398631982, -271.9070030809024843, -196.8870656809470461 ) ) ;
#44596 = CIRCLE ( 'NONE', #80833, 4.999999999999997335 ) ;
#44597 = CARTESIAN_POINT ( 'NONE',  ( -11.02651898563433441, -278.1275328455262752, -339.0843757538093541 ) ) ;
#44598 = CARTESIAN_POINT ( 'NONE',  ( -64.38333566952888987, -278.2170181170437218, -338.3954395343232591 ) ) ;
#44599 = CARTESIAN_POINT ( 'NONE',  ( -94.72325778133917140, -285.8844174726269785, -318.6754674865924812 ) ) ;
#44600 = EDGE_CURVE ( 'NONE', #43712, #35960, #91897, .T. ) ;
#44601 = ORIENTED_EDGE ( 'NONE', *, *, #36488, .T. ) ;
#44602 = DIRECTION ( 'NONE',  ( 0.000000000000000000, 0.000000000000000000, 1.000000000000000000 ) ) ;
#44603 = CARTESIAN_POINT ( 'NONE',  ( -112.6000473950164888, -296.5898526349620283, -254.0152002827317688 ) ) ;
#44604 = CARTESIAN_POINT ( 'NONE',  ( -1.416422438511701021, -288.5104897743728998, -204.8720907206462414 ) ) ;
#44605 = CARTESIAN_POINT ( 'NONE',  ( 195.6515579107327483, 26.26913368994353348, 14.74629060332673980 ) ) ;
#44606 = CARTESIAN_POINT ( 'NONE',  ( -72.08107566293803359, -292.9809262143061233, -342.4248175857292154 ) ) ;
#44607 = CARTESIAN_POINT ( 'NONE',  ( -107.1320942456446090, -277.8819512006079435, -238.4403332413932901 ) ) ;
#44608 = CARTESIAN_POINT ( 'NONE',  ( -81.45054519529385573, -289.8629449931410136, -208.2253778607089032 ) ) ;
#44609 = CARTESIAN_POINT ( 'NONE',  ( -79.72370072472189406, -286.9881181221589941, -210.0118627776461722 ) ) ;
#44610 = CONICAL_SURFACE ( 'NONE', #77901, 5.025000000000002132, 0.7853981633971707232 ) ;
#44611 = CARTESIAN_POINT ( 'NONE',  ( -68.97646978270985585, -281.3904523356027880, -203.4491208114842777 ) ) ;
#44612 = CARTESIAN_POINT ( 'NONE',  ( 35.28327770688060383, -288.6743423350946500, -246.4387367549829548 ) ) ;
#44613 = CARTESIAN_POINT ( 'NONE',  ( 37.56466911442159784, -283.6004216151127935, -274.1076487702263194 ) ) ;
#44614 = CARTESIAN_POINT ( 'NONE',  ( -39.96082666270670103, -277.2508535597563650, -347.3296270181057821 ) ) ;
#44615 = CARTESIAN_POINT ( 'NONE',  ( -95.72232120735915828, -295.2146963515584162, -223.8471427734565680 ) ) ;
#44616 = CARTESIAN_POINT ( 'NONE',  ( -109.6054548109871263, -278.7232482755541128, -243.6186671819040441 ) ) ;
#44617 = CARTESIAN_POINT ( 'NONE',  ( -13.69402298196853529, -276.2228071967882670, -199.9931363106979347 ) ) ;
#44618 = CARTESIAN_POINT ( 'NONE',  ( 169.7306087885279169, 249.5000000000000568, -24.89999999999998792 ) ) ;
#44619 = ADVANCED_FACE ( 'NONE', ( #40752, #76312, #5752, #61642 ), #62105, .F. ) ;
#44620 = CLOSED_SHELL ( 'NONE', ( #16198, #13204, #69298, #11489, #49402, #51333, #56872, #91623, #29850, #42271, #64220, #75500, #30698, #33856, #75088, #30940, #83301, #68366, #75852, #733, #73637, #81893, #24291, #84393, #8068, #75445, #19071 ) ) ;
#44621 = CARTESIAN_POINT ( 'NONE',  ( -106.6662871844225293, -287.4805209788416391, -237.0123917617630980 ) ) ;
#44622 = CARTESIAN_POINT ( 'NONE',  ( -49.53425585000079678, -272.1387402999603751, -195.3059184839057139 ) ) ;
#44623 = CARTESIAN_POINT ( 'NONE',  ( 213.7238915819278589, 32.98517505407394168, 12.09245862095555601 ) ) ;
#44624 = CARTESIAN_POINT ( 'NONE',  ( -87.56838295377406212, -278.8359714518171586, -217.2321004917276923 ) ) ;
#44625 = CARTESIAN_POINT ( 'NONE',  ( 14.62513591415104663, -277.5453004359696934, -326.7134886409957630 ) ) ;
#44626 = CARTESIAN_POINT ( 'NONE',  ( -21.78541642493446773, -281.9161992435768411, -345.5330691986537772 ) ) ;
#44627 = CARTESIAN_POINT ( 'NONE',  ( 20.31681896614901817, -289.9593618248425173, -316.7666046462033478 ) ) ;
#44628 = CARTESIAN_POINT ( 'NONE',  ( -93.16883987994312122, -298.7885027996163672, -218.2644281607912546 ) ) ;
#44629 = CARTESIAN_POINT ( 'NONE',  ( -106.1633422266400828, -298.1914197729561238, -236.7219994400396672 ) ) ;
#44630 = CARTESIAN_POINT ( 'NONE',  ( 37.25392819670436495, -295.6290118142692336, -276.3210390607483760 ) ) ;
#44631 = CARTESIAN_POINT ( 'NONE',  ( 18.44613789808553861, -278.8559449414447613, -220.4838129597063698 ) ) ;
#44632 = CARTESIAN_POINT ( 'NONE',  ( -65.15884029580085723, -271.7069913710247988, -201.0793533605327355 ) ) ;
#44633 = CARTESIAN_POINT ( 'NONE',  ( -111.4364158034859429, -285.9267762441473337, -288.2043090941172068 ) ) ;
#44634 = CARTESIAN_POINT ( 'NONE',  ( -50.82173890067777933, -288.1486111645336337, -342.4721225434952885 ) ) ;
#44635 = CARTESIAN_POINT ( 'NONE',  ( 203.4894716936504722, 292.6718879101889570, -83.16901316872426264 ) ) ;
#44636 = ORIENTED_EDGE ( 'NONE', *, *, #7316, .F. ) ;
#44637 = CARTESIAN_POINT ( 'NONE',  ( 35.81596198814759191, -286.4063980440811861, -292.4646931912116656 ) ) ;
#44638 = CARTESIAN_POINT ( 'NONE',  ( -8.213959618484716785, -288.3267408992413721, -337.3753253256066955 ) ) ;
#44639 = ORIENTED_EDGE ( 'NONE', *, *, #19673, .F. ) ;
#44640 = CARTESIAN_POINT ( 'NONE',  ( -97.34717193201876739, -286.2737686607163141, -222.6030206056668987 ) ) ;
#44641 = CARTESIAN_POINT ( 'NONE',  ( -37.80563493136995135, -277.3913669075303119, -343.3932448444861052 ) ) ;
#44642 = EDGE_CURVE ( 'NONE', #74853, #45543, #69669, .T. ) ;
#44643 = CARTESIAN_POINT ( 'NONE',  ( 23.73741687090086216, -291.8517634764929767, -223.9624184666445217 ) ) ;
#44644 = CARTESIAN_POINT ( 'NONE',  ( 29.67713935713489448, -282.6946486322358396, -308.1762652143417540 ) ) ;
#44645 = CARTESIAN_POINT ( 'NONE',  ( 31.77270039375430954, -283.4915360243597320, -302.8261636814642088 ) ) ;
#44646 = CARTESIAN_POINT ( 'NONE',  ( -81.54594247968130105, -283.9685738634240124, -333.4476209434370162 ) ) ;
#44647 = CARTESIAN_POINT ( 'NONE',  ( -27.55974336206074327, -280.5129850451773450, -197.9469330038109831 ) ) ;
#44648 = CARTESIAN_POINT ( 'NONE',  ( 26.53690525259170840, -296.4086741954485547, -200.3901485728259502 ) ) ;
#44649 = CARTESIAN_POINT ( 'NONE',  ( 180.4107272569747522, 254.1056192471400834, -166.8072156021353862 ) ) ;
#44650 = ORIENTED_EDGE ( 'NONE', *, *, #266, .T. ) ;
#44651 = CARTESIAN_POINT ( 'NONE',  ( -36.41863139110428449, -279.0407500586431979, -345.2015424416197789 ) ) ;
#44652 = CARTESIAN_POINT ( 'NONE',  ( 44.12337886667094722, 12.84550829123691607, -331.4150732913272464 ) ) ;
#44653 = CARTESIAN_POINT ( 'NONE',  ( 172.1664621943805855, 241.6173149327171927, -177.3709744135503570 ) ) ;
#44654 = CARTESIAN_POINT ( 'NONE',  ( -109.8362118316587441, -296.0296523786192324, -260.5748814699558125 ) ) ;
#44655 = CARTESIAN_POINT ( 'NONE',  ( 37.39872793009974572, -293.2890167128820167, -288.6753417241641841 ) ) ;
#44656 = CARTESIAN_POINT ( 'NONE',  ( -76.03803979523620171, -208.5652239327323230, -353.7424279183983344 ) ) ;
#44658 = CARTESIAN_POINT ( 'NONE',  ( -87.28560909400981416, -288.1617947099340995, -324.7632003716275335 ) ) ;
#44657 = CARTESIAN_POINT ( 'NONE',  ( -97.75683960899084468, -295.7565143839406687, -223.5573490943200170 ) ) ;
#44659 = CARTESIAN_POINT ( 'NONE',  ( -36.96589763307245136, -296.9077808332467612, -344.6080054043234782 ) ) ;
#44660 = CARTESIAN_POINT ( 'NONE',  ( 35.94505693686367209, -288.9478502166791714, -276.5060089043064977 ) ) ;
#44661 = ORIENTED_EDGE ( 'NONE', *, *, #1524, .F. ) ;
#44662 = CARTESIAN_POINT ( 'NONE',  ( -56.00145377709480954, -296.2280420907616190, -344.8234158657631383 ) ) ;
#44663 = CARTESIAN_POINT ( 'NONE',  ( -10.73339725628381913, -286.9010971248844726, -202.3035759172179269 ) ) ;
#44664 = CARTESIAN_POINT ( 'NONE',  ( 19.04079931267920500, -297.5382118137887346, -193.7694208783678960 ) ) ;
#44665 = CARTESIAN_POINT ( 'NONE',  ( -25.05735014571818908, -293.0078349272711762, -194.5109131998279679 ) ) ;
#44666 = CARTESIAN_POINT ( 'NONE',  ( 21.32479549574819799, -294.7160000565395421, -320.1383135106926829 ) ) ;
#44667 = CARTESIAN_POINT ( 'NONE',  ( -90.76063324359087403, -291.4343998394230653, -220.5890667451404852 ) ) ;
#44668 = ORIENTED_EDGE ( 'NONE', *, *, #47032, .F. ) ;
#44669 = DIRECTION ( 'NONE',  ( 1.000000000000000000, -0.000000000000000000, -0.000000000000000000 ) ) ;
#44670 = CARTESIAN_POINT ( 'NONE',  ( -24.43018444405199929, -276.1357367808887489, -195.8592807407198677 ) ) ;
#44671 = CARTESIAN_POINT ( 'NONE',  ( 33.80971135660507798, -274.7106289550790166, -298.8851311009365759 ) ) ;
#44672 = VERTEX_POINT ( 'NONE', #41708 ) ;
#44673 = CARTESIAN_POINT ( 'NONE',  ( -74.07299186125582935, -277.0344159499891248, -337.9803917655460737 ) ) ;
#44674 = CARTESIAN_POINT ( 'NONE',  ( -37.12834905313825828, -296.5347552425564572, -196.6649599176964784 ) ) ;
#44675 = CARTESIAN_POINT ( 'NONE',  ( -67.32288110887056121, -275.5891577717744667, -338.2727831776886092 ) ) ;
#44676 = CARTESIAN_POINT ( 'NONE',  ( -108.2425790858671348, -273.8791828732166209, -251.5305680901520589 ) ) ;
#44677 = CARTESIAN_POINT ( 'NONE',  ( -40.79800506375547542, -274.9490062376215178, -197.1575673354057869 ) ) ;
#44678 = CARTESIAN_POINT ( 'NONE',  ( -78.31426933644966937, -275.2691208377483463, -206.3671918259205711 ) ) ;
#44679 = CARTESIAN_POINT ( 'NONE',  ( -57.65349535606151932, -271.8114165114203615, -197.7407897154428440 ) ) ;
#44680 = CARTESIAN_POINT ( 'NONE',  ( -108.6895465585165397, -296.9938770632317642, -286.2789532096331868 ) ) ;
#44681 = CARTESIAN_POINT ( 'NONE',  ( -5.301236082398643745, -293.1967711233344289, -336.6229329529934375 ) ) ;
#44682 = CARTESIAN_POINT ( 'NONE',  ( 208.4306832106271088, -74.55766379199613425, 0.000000000000000000 ) ) ;
#44683 = CARTESIAN_POINT ( 'NONE',  ( 23.47326059264479881, -276.6745026864238639, -317.5106893298946034 ) ) ;
#44684 = CARTESIAN_POINT ( 'NONE',  ( -8.972789955045374910, -274.6003677338711100, -203.0449969625420010 ) ) ;
#44685 = CIRCLE ( 'NONE', #23538, 11.60392986742922439 ) ;
#44686 = CARTESIAN_POINT ( 'NONE',  ( -68.28584703499974751, -284.3389852862416660, -200.3771416406644619 ) ) ;
#44687 = CARTESIAN_POINT ( 'NONE',  ( -110.4961289190214160, -298.7736498809231307, -253.0851815561672709 ) ) ;
#44688 = DIRECTION ( 'NONE',  ( 0.000000000000000000, 0.000000000000000000, 1.000000000000000000 ) ) ;
#44689 = CARTESIAN_POINT ( 'NONE',  ( -6.940097155144616892, -285.6587834874952136, -203.8015540110765755 ) ) ;
#44690 = CARTESIAN_POINT ( 'NONE',  ( -85.78519100076424309, -275.9731597293535401, -326.3861723131170720 ) ) ;
#44691 = CARTESIAN_POINT ( 'NONE',  ( -110.7575939558557252, -277.0516825539775709, -276.1069616884851143 ) ) ;
#44692 = CARTESIAN_POINT ( 'NONE',  ( 21.21648027691207261, -284.1969157558150414, -317.2421113133214590 ) ) ;
#44693 = CARTESIAN_POINT ( 'NONE',  ( -1.542295531487216209, -275.7430442908468535, -206.2722937548323046 ) ) ;
#44694 = CARTESIAN_POINT ( 'NONE',  ( 155.2899061951533213, 19.82375796246816435, 13.63853015639329413 ) ) ;
#44695 = CARTESIAN_POINT ( 'NONE',  ( 22.00497724944198552, -274.5995621614944753, -318.1772756555577075 ) ) ;
#44696 = CARTESIAN_POINT ( 'NONE',  ( -56.12377700401275860, -281.8110800841286618, -197.5251300938368502 ) ) ;
#44697 = CARTESIAN_POINT ( 'NONE',  ( 151.6966102050380414, 129.9764884006976899, 12.50000000000000178 ) ) ;
#44698 = CARTESIAN_POINT ( 'NONE',  ( -54.65878368267649989, -287.7514365363581419, -196.8122715449479472 ) ) ;
#44699 = CARTESIAN_POINT ( 'NONE',  ( 154.6019620322547041, 19.02489598991821751, -11.88315578651767979 ) ) ;
#44700 = CARTESIAN_POINT ( 'NONE',  ( -68.09640297299399947, -289.6482022707571673, -201.9429564497393130 ) ) ;
#44701 = DIRECTION ( 'NONE',  ( -0.9531768234071980039, 0.3024135303179465994, 0.000000000000000000 ) ) ;
#44702 = CARTESIAN_POINT ( 'NONE',  ( -85.62160426803460211, -272.0527504544953104, -214.8830665554402515 ) ) ;
#44703 = CARTESIAN_POINT ( 'NONE',  ( -60.62426123480083362, -289.8866211824146149, -199.8175581276832418 ) ) ;
#44704 = CARTESIAN_POINT ( 'NONE',  ( -101.2450674239233592, -254.4445186991787295, -323.9438275447045612 ) ) ;
#44705 = CARTESIAN_POINT ( 'NONE',  ( 180.2297292323760303, 215.0000000000001705, -24.97289011430694217 ) ) ;
#44706 = CARTESIAN_POINT ( 'NONE',  ( 31.05727500542148789, -286.4720547611850634, -304.3075498103050904 ) ) ;
#44707 = CARTESIAN_POINT ( 'NONE',  ( -32.06842260366386910, -284.5846534396746392, -343.9724823211214471 ) ) ;
#44708 = CARTESIAN_POINT ( 'NONE',  ( -70.60218817851117024, -283.8594481473888322, -202.0404479599195042 ) ) ;
#44709 = CARTESIAN_POINT ( 'NONE',  ( -69.01760083171541282, -291.6236601841486618, -204.5777373949150046 ) ) ;
#44710 = CARTESIAN_POINT ( 'NONE',  ( 35.28801081261830319, -283.1324308091676585, -282.2059483491906917 ) ) ;
#44711 = CARTESIAN_POINT ( 'NONE',  ( 33.11771182293239235, -282.6147824746102515, -290.0606863735500269 ) ) ;
#44712 = CARTESIAN_POINT ( 'NONE',  ( -31.91940922578854511, -290.9640783308745426, -345.5724175824318536 ) ) ;
#44713 = CARTESIAN_POINT ( 'NONE',  ( -23.36195680614620684, -298.3893324513517200, -193.3607339042446540 ) ) ;
#44714 = ORIENTED_EDGE ( 'NONE', *, *, #26543, .T. ) ;
#44715 = CARTESIAN_POINT ( 'NONE',  ( -18.11478860929830148, -286.8860449579979672, -343.4339588246510289 ) ) ;
#44716 = CARTESIAN_POINT ( 'NONE',  ( 39.63086186175308256, -275.5264464585653741, -268.3057103049698640 ) ) ;
#44717 = CARTESIAN_POINT ( 'NONE',  ( -60.79924813879813428, -293.7263106862739050, -199.4436958951495740 ) ) ;
#44718 = CARTESIAN_POINT ( 'NONE',  ( 201.2104617360081704, 60.19600395700749829, 9.000000000000001776 ) ) ;
#44719 = CARTESIAN_POINT ( 'NONE',  ( -20.19161114001083490, -297.3376638359846424, -345.3538533559490702 ) ) ;
#44720 = CARTESIAN_POINT ( 'NONE',  ( -23.99223936933285017, -281.5628720852006381, -342.6316885778049368 ) ) ;
#44721 = CARTESIAN_POINT ( 'NONE',  ( -61.83329689734288337, -275.3694319706043530, -341.4807822853480275 ) ) ;
#44722 = CARTESIAN_POINT ( 'NONE',  ( 156.4947056272797852, 20.00000000000000000, -15.00000000000000000 ) ) ;
#44723 = CARTESIAN_POINT ( 'NONE',  ( -113.5665141736607637, -294.9259093960350242, -272.4275516044332903 ) ) ;
#44724 = CARTESIAN_POINT ( 'NONE',  ( 35.74498614642443783, -274.8810675183170247, -268.8681487109377031 ) ) ;
#44725 = CARTESIAN_POINT ( 'NONE',  ( -57.86643658045814931, -293.3024744560507884, -199.5303163994831550 ) ) ;
#44726 = CARTESIAN_POINT ( 'NONE',  ( 8.988454232498714447, -293.6470273010241954, -213.5774049988777392 ) ) ;
#44727 = CARTESIAN_POINT ( 'NONE',  ( -109.6597734657279517, -286.5179925544603634, -254.5516204331351275 ) ) ;
#44728 = CARTESIAN_POINT ( 'NONE',  ( 38.85213999318408185, -294.9049098300262131, -264.6074218465794274 ) ) ;
#44729 = CARTESIAN_POINT ( 'NONE',  ( 17.22166499399533635, -295.6089827009751616, -324.0661191648778185 ) ) ;
#44730 = CARTESIAN_POINT ( 'NONE',  ( -66.05509232820192267, -295.2720244408669714, -337.4769962296836070 ) ) ;
#44731 = CARTESIAN_POINT ( 'NONE',  ( -88.06372293221394898, -291.7615039317842047, -325.6789649307979175 ) ) ;
#44732 = CARTESIAN_POINT ( 'NONE',  ( -55.70012464209018077, -283.4488524062487045, -345.1405821010450836 ) ) ;
#44733 = CARTESIAN_POINT ( 'NONE',  ( -36.88264727789704267, -296.1377079819332039, -194.8012588250561521 ) ) ;
#44734 = CARTESIAN_POINT ( 'NONE',  ( -104.4180584499296458, -283.8935991299841817, -308.2813115394941974 ) ) ;
#44735 = CARTESIAN_POINT ( 'NONE',  ( -94.85763323616953357, -279.8721596840393318, -317.9601673568814704 ) ) ;
#44736 = CARTESIAN_POINT ( 'NONE',  ( -110.6236579043854391, -283.4118556721556956, -265.4232834957563796 ) ) ;
#44737 = CARTESIAN_POINT ( 'NONE',  ( 25.47688555729405380, -284.9993870828847093, -229.3876394770667275 ) ) ;
#44738 = CARTESIAN_POINT ( 'NONE',  ( -106.2851385975139635, -277.1013322941293495, -238.8166198569192886 ) ) ;
#44739 = CARTESIAN_POINT ( 'NONE',  ( 200.9306832106271088, -134.2391364535880882, 0.000000000000000000 ) ) ;
#44740 = CARTESIAN_POINT ( 'NONE',  ( -107.4527420557531485, -283.7875800675814730, -290.9589078047928865 ) ) ;
#44741 = CARTESIAN_POINT ( 'NONE',  ( 29.42339311803416990, -283.2482220161219857, -308.0249686546339944 ) ) ;
#44742 = CARTESIAN_POINT ( 'NONE',  ( -1.919984878073659917, -287.6533100300147794, -338.4648792764691621 ) ) ;
#44743 = CARTESIAN_POINT ( 'NONE',  ( -79.76372037430267881, -279.2150229643513626, -333.7240142589708398 ) ) ;
#44744 = CARTESIAN_POINT ( 'NONE',  ( -59.50603922779158950, -278.6485014039391217, -343.5870720149753765 ) ) ;
#44745 = CARTESIAN_POINT ( 'NONE',  ( -70.93977880302659855, -279.4292542214962509, -205.5383189467578688 ) ) ;
#44746 = CARTESIAN_POINT ( 'NONE',  ( -21.61145548622377177, -276.2347099145011384, -197.3925891287979653 ) ) ;
#44747 = CARTESIAN_POINT ( 'NONE',  ( 36.36968895583773786, -293.8336313973234724, -292.8045129553890433 ) ) ;
#44748 = CARTESIAN_POINT ( 'NONE',  ( 37.51496625655154560, -285.5252883449841192, -268.2864241490587460 ) ) ;
#44749 = VECTOR ( 'NONE', #43487, 1000.000000000000000 ) ;
#44750 = CARTESIAN_POINT ( 'NONE',  ( -64.12688193265761072, -293.3087435754818557, -198.9683332250135379 ) ) ;
#44751 = CARTESIAN_POINT ( 'NONE',  ( 29.76753150895131128, -292.8677587994326927, -299.8666615598075964 ) ) ;
#44752 = CARTESIAN_POINT ( 'NONE',  ( 32.76928783810420498, -293.4892996287213123, -290.8152853006679379 ) ) ;
#44753 = CARTESIAN_POINT ( 'NONE',  ( -94.49017891993483431, -292.3283144061011853, -219.2187296741897740 ) ) ;
#44754 = CARTESIAN_POINT ( 'NONE',  ( 23.76318053072366610, -281.6469269062584431, -230.1439659249684269 ) ) ;
#44755 = EDGE_CURVE ( 'NONE', #13111, #41136, #10252, .T. ) ;
#44756 = CARTESIAN_POINT ( 'NONE',  ( -93.96358585662680696, -272.3182801167610592, -218.5075328834848847 ) ) ;
#44757 = CARTESIAN_POINT ( 'NONE',  ( 28.60685175407669689, -287.6859457337085928, -230.7097191566026595 ) ) ;
#44758 = CARTESIAN_POINT ( 'NONE',  ( 21.54798034489373038, -280.3416052439997657, -318.0503424261314649 ) ) ;
#44759 = CARTESIAN_POINT ( 'NONE',  ( 23.27343695480106689, -288.5200472869787518, -317.8328387135502453 ) ) ;
#44760 = CARTESIAN_POINT ( 'NONE',  ( -71.19179091716839025, -285.9255657695690616, -205.6598132011637574 ) ) ;
#44761 = FACE_OUTER_BOUND ( 'NONE', #88514, .T. ) ;
#44762 = CARTESIAN_POINT ( 'NONE',  ( -14.33830847277128662, -91.16400973458658541, -357.8324979133209354 ) ) ;
#44763 = CARTESIAN_POINT ( 'NONE',  ( -82.89404955411457365, -218.6374574953077570, -348.8632550632670473 ) ) ;
#44764 = CARTESIAN_POINT ( 'NONE',  ( -105.4217893198336782, -277.3918462768014592, -297.1511008538128635 ) ) ;
#44765 = CARTESIAN_POINT ( 'NONE',  ( -110.5895536243074986, -277.4331145171180424, -273.3574542330976556 ) ) ;
#44766 = CARTESIAN_POINT ( 'NONE',  ( -30.48509448647785547, -297.6434982183235434, -193.4232108530147229 ) ) ;
#44767 = CARTESIAN_POINT ( 'NONE',  ( -96.95894580772622362, -247.6687050397709129, -332.0224721523202902 ) ) ;
#44768 = CARTESIAN_POINT ( 'NONE',  ( -67.52953661069818736, -276.1248168577565139, -340.6604266715875724 ) ) ;
#44769 = CARTESIAN_POINT ( 'NONE',  ( -78.90372080204622307, -297.3643163006117334, -333.9737932112203680 ) ) ;
#44770 = CARTESIAN_POINT ( 'NONE',  ( -93.49115227342161916, -291.7073450886715591, -223.5951683252780526 ) ) ;
#44771 = CARTESIAN_POINT ( 'NONE',  ( -48.95569808031642367, -298.7107656020162381, -194.3518271525058765 ) ) ;
#44772 = CARTESIAN_POINT ( 'NONE',  ( -66.54026285516115991, -288.1274541424928088, -337.8594634240878918 ) ) ;
#44773 = CARTESIAN_POINT ( 'NONE',  ( -14.83877591472487012, -298.8191636796547073, -193.4208306832735502 ) ) ;
#44774 = CARTESIAN_POINT ( 'NONE',  ( -108.5914054341570392, -296.5092223847959758, -286.2507214494972914 ) ) ;
#44775 = ORIENTED_EDGE ( 'NONE', *, *, #58549, .T. ) ;
#44776 = DIRECTION ( 'NONE',  ( -1.000000000000000000, 0.000000000000000000, 0.000000000000000000 ) ) ;
#44777 = CARTESIAN_POINT ( 'NONE',  ( -111.3129590246118426, -280.6695308242854594, -254.8854119829896945 ) ) ;
#44778 = CARTESIAN_POINT ( 'NONE',  ( -99.42960280185914712, -279.0946903869648281, -309.4343484115653382 ) ) ;
#44779 = CARTESIAN_POINT ( 'NONE',  ( -88.51295616188255622, -279.5183081714269520, -326.5347467389992744 ) ) ;
#44780 = CARTESIAN_POINT ( 'NONE',  ( -87.79400934037354887, -271.8119228288654767, -216.5765389216107621 ) ) ;
#44781 = DIRECTION ( 'NONE',  ( -0.000000000000000000, -0.000000000000000000, -1.000000000000000000 ) ) ;
#44782 = FACE_OUTER_BOUND ( 'NONE', #32173, .T. ) ;
#44783 = CARTESIAN_POINT ( 'NONE',  ( -4.349468131463234855, -280.6662493064595765, -205.2280084688505326 ) ) ;
#44784 = CARTESIAN_POINT ( 'NONE',  ( 21.72016852956733501, -275.6924834627180871, -221.2097752563675215 ) ) ;
#44785 = CARTESIAN_POINT ( 'NONE',  ( 18.40806390262041248, -278.2515910834043211, -320.5497030182786489 ) ) ;
#44786 = CARTESIAN_POINT ( 'NONE',  ( -98.34406267571065996, -276.5091596740006707, -316.3969231582526618 ) ) ;
#44787 = ORIENTED_EDGE ( 'NONE', *, *, #80099, .F. ) ;
#44788 = DIRECTION ( 'NONE',  ( -0.000000000000000000, -0.000000000000000000, 1.000000000000000000 ) ) ;
#44789 = CARTESIAN_POINT ( 'NONE',  ( -3.606082695485143930, -284.5891196346562992, -337.7573191692628143 ) ) ;
#44790 = CARTESIAN_POINT ( 'NONE',  ( -105.8582764708482244, -290.0925123653496485, -244.5643403522202846 ) ) ;
#44791 = CARTESIAN_POINT ( 'NONE',  ( -40.80356843434887537, -285.3584038721391494, -193.4888905030086050 ) ) ;
#44792 = CARTESIAN_POINT ( 'NONE',  ( -85.53839468222153641, -281.9694747034328657, -326.5309732887333780 ) ) ;
#44793 = CARTESIAN_POINT ( 'NONE',  ( -96.40543317635200538, -282.5161207291093319, -314.2570216278494399 ) ) ;
#44794 = CARTESIAN_POINT ( 'NONE',  ( -1.787096532268313887, -281.7395368591172655, -206.1505217501277514 ) ) ;
#44795 = CARTESIAN_POINT ( 'NONE',  ( 64.47034096727303165, 48.08436259181641503, -318.7852478153986908 ) ) ;
#44796 = CARTESIAN_POINT ( 'NONE',  ( -81.11879237899330519, -282.0354755576044568, -332.7952388372868882 ) ) ;
#44797 = CARTESIAN_POINT ( 'NONE',  ( 27.72748973062332212, -295.0547921759773544, -233.0649897977404805 ) ) ;
#44798 = CARTESIAN_POINT ( 'NONE',  ( -62.60970155663485315, -287.7242411621383553, -199.5687700240574145 ) ) ;
#44799 = EDGE_CURVE ( 'NONE', #86758, #70448, #69538, .T. ) ;
#44800 = EDGE_CURVE ( 'NONE', #4038, #52800, #19019, .T. ) ;
#44801 = CARTESIAN_POINT ( 'NONE',  ( 152.4771702478159909, 19.90416625621075752, 8.234418254360116762 ) ) ;
#44802 = CARTESIAN_POINT ( 'NONE',  ( -6.497557358764993296, -294.3741731780079931, -201.3691821394449164 ) ) ;
#44803 = CARTESIAN_POINT ( 'NONE',  ( 27.08083609230942912, -274.0659118144562285, -308.7634287702098845 ) ) ;
#44804 = CARTESIAN_POINT ( 'NONE',  ( 25.71332827411659849, -287.3318785423260238, -314.3639847695816343 ) ) ;
#44805 = CARTESIAN_POINT ( 'NONE',  ( -32.08013147951756139, -290.5194624245420982, -196.7361571637703719 ) ) ;
#44806 = CARTESIAN_POINT ( 'NONE',  ( -48.18343439339133027, -261.8354831489689332, -437.9975051613113806 ) ) ;
#44807 = CARTESIAN_POINT ( 'NONE',  ( -108.0885160136129599, -277.4988490640187706, -250.4114605798086188 ) ) ;
#44808 = CARTESIAN_POINT ( 'NONE',  ( -102.2838809488369662, -295.1751045264184086, -234.3975443534600345 ) ) ;
#44809 = CARTESIAN_POINT ( 'NONE',  ( -102.0695999085541388, -291.3945649229704600, -305.2761892758041427 ) ) ;
#44810 = CARTESIAN_POINT ( 'NONE',  ( 197.1123855246548828, 18.41506350946109194, 10.91506350946109016 ) ) ;
#44811 = CARTESIAN_POINT ( 'NONE',  ( 35.62967047056401526, -291.7493174923444030, -248.0477402503465498 ) ) ;
#44812 = CARTESIAN_POINT ( 'NONE',  ( 36.45533259483765676, -289.1609277709895309, -271.0232163866380120 ) ) ;
#44813 = CARTESIAN_POINT ( 'NONE',  ( -92.86785171340416412, -288.0745598828029301, -322.3100952687722156 ) ) ;
#44814 = CARTESIAN_POINT ( 'NONE',  ( -39.96089308189817046, -290.5108494771675396, -343.9536993061166186 ) ) ;
#44815 = CARTESIAN_POINT ( 'NONE',  ( 34.17068769065854639, -288.5590217795732997, -285.8659523390452364 ) ) ;
#44816 = CARTESIAN_POINT ( 'NONE',  ( -25.14856655163930910, -296.8774596948274507, -344.7762146540899266 ) ) ;
#44817 = CARTESIAN_POINT ( 'NONE',  ( 189.4188515237862589, 293.9636489450775798, -40.00000000000000711 ) ) ;
#44818 = CARTESIAN_POINT ( 'NONE',  ( -37.48536153880243660, -290.2589463793318032, -346.9769168707042013 ) ) ;
#44819 = CARTESIAN_POINT ( 'NONE',  ( -81.25936728188860059, -277.4785086805243282, -209.1267704977872484 ) ) ;
#44820 = CARTESIAN_POINT ( 'NONE',  ( -112.9762002832144816, -279.0654999807183572, -255.9669613026391914 ) ) ;
#44821 = CARTESIAN_POINT ( 'NONE',  ( -42.42441875411951457, -279.6564150252649483, -193.5502446448204239 ) ) ;
#44822 = CARTESIAN_POINT ( 'NONE',  ( -110.6135000402559996, -282.7582995383197613, -254.2936281617217844 ) ) ;
#44823 = CARTESIAN_POINT ( 'NONE',  ( 128.9467878515196162, -299.5541904835127980, -195.3611179825600175 ) ) ;
#44824 = CARTESIAN_POINT ( 'NONE',  ( -13.89668288513848537, -278.4990481378181926, -199.8710056227882319 ) ) ;
#44825 = CARTESIAN_POINT ( 'NONE',  ( -109.9454637646575321, -282.3097460895926929, -289.2188602398896933 ) ) ;
#44826 = CARTESIAN_POINT ( 'NONE',  ( 121.3887860922853150, -299.5541904835127980, -193.1197964255135844 ) ) ;
#44827 = CARTESIAN_POINT ( 'NONE',  ( -109.8844550021252360, -277.3344239351918645, -246.5238099684989095 ) ) ;
#44828 = CARTESIAN_POINT ( 'NONE',  ( -109.7125227737370494, -274.1555102275907529, -256.7525563329999159 ) ) ;
#44829 = CARTESIAN_POINT ( 'NONE',  ( -85.91723954275585129, -282.6276006684570348, -329.7067958323213475 ) ) ;
#44830 = CARTESIAN_POINT ( 'NONE',  ( -87.45133094437605337, -274.1345033083858880, -216.9848356747382070 ) ) ;
#44831 = CARTESIAN_POINT ( 'NONE',  ( -67.32131059478003010, -275.0918828034294279, -200.0771991241786054 ) ) ;
#44832 = CARTESIAN_POINT ( 'NONE',  ( 32.88152789986077806, -274.9520975295013727, -250.1607706154053119 ) ) ;
#44833 = CARTESIAN_POINT ( 'NONE',  ( -64.26376091054356721, -297.4034475821760566, -340.4175866497764105 ) ) ;
#44834 = CARTESIAN_POINT ( 'NONE',  ( -1.798836417077152916, -288.7610629285026675, -338.6670829032461825 ) ) ;
#44835 = CARTESIAN_POINT ( 'NONE',  ( -31.16659066621182106, -278.2092962448659250, -195.0021606616707288 ) ) ;
#44836 = CARTESIAN_POINT ( 'NONE',  ( -114.1126571216632613, -290.3030509816737208, -276.9514797539881670 ) ) ;
#44837 = CARTESIAN_POINT ( 'NONE',  ( -110.0244992001172477, -289.4928306369570805, -279.3399356704422303 ) ) ;
#44838 = CARTESIAN_POINT ( 'NONE',  ( 36.36459098178308835, -291.3739008404184574, -256.4908871948564411 ) ) ;
#44839 = VERTEX_POINT ( 'NONE', #26102 ) ;
#44840 = CARTESIAN_POINT ( 'NONE',  ( 197.0996632504151762, 71.85522536017060702, 12.14506853158196265 ) ) ;
#44841 = CARTESIAN_POINT ( 'NONE',  ( -108.1665842616880440, -290.2969794809960717, -252.3707939916815519 ) ) ;
#44842 = CARTESIAN_POINT ( 'NONE',  ( -57.23711263161519724, -331.8906705383788562, 52.50000000000000711 ) ) ;
#44843 = CARTESIAN_POINT ( 'NONE',  ( -23.83911004664717836, -287.1617319711425580, -194.7392162161667954 ) ) ;
#44844 = CARTESIAN_POINT ( 'NONE',  ( -102.0172624299486870, -292.6233781216987495, -301.5434626090942061 ) ) ;
#44845 = CARTESIAN_POINT ( 'NONE',  ( -70.71644438930614740, -294.5402841608669746, -339.5055105387589833 ) ) ;
#44846 = CARTESIAN_POINT ( 'NONE',  ( -13.55923351420843304, -284.0648632846011310, -343.0776398579266697 ) ) ;
#44847 = CARTESIAN_POINT ( 'NONE',  ( -102.2374226790117575, -284.8399235084859242, -236.9314126432019521 ) ) ;
#44848 = CARTESIAN_POINT ( 'NONE',  ( 36.13560834171039460, -276.8473382598899661, -268.8351374350356764 ) ) ;
#44849 = CARTESIAN_POINT ( 'NONE',  ( 24.72254015447936126, -291.0090541605105727, -228.8897196343893370 ) ) ;
#44850 = CARTESIAN_POINT ( 'NONE',  ( -6.347422214351442271, -273.2635757185508396, -203.8292816731760979 ) ) ;
#44851 = EDGE_LOOP ( 'NONE', ( #91719, #32832, #13700, #34907, #25675 ) ) ;
#44852 = DIRECTION ( 'NONE',  ( 0.000000000000000000, 0.000000000000000000, -1.000000000000000000 ) ) ;
#44853 = CARTESIAN_POINT ( 'NONE',  ( 21.34877672232704526, -293.8905051744324055, -320.1724843428212353 ) ) ;
#44854 = CARTESIAN_POINT ( 'NONE',  ( -71.86739548078840301, -287.5121820922828419, -204.4119666553180821 ) ) ;
#44855 = CARTESIAN_POINT ( 'NONE',  ( -114.0013770531242443, -297.6769958988410849, -266.7635474953483481 ) ) ;
#44856 = CARTESIAN_POINT ( 'NONE',  ( -30.53003536021292774, -286.7918340046165326, -197.5263639791413368 ) ) ;
#44857 = CARTESIAN_POINT ( 'NONE',  ( -112.5654737403736334, -277.4181082703252628, -285.7298566160930591 ) ) ;
#44858 = CARTESIAN_POINT ( 'NONE',  ( 13.20522743624334794, -293.3888403381756689, -212.4100964203909427 ) ) ;
#44859 = CARTESIAN_POINT ( 'NONE',  ( 37.75417510060062654, -285.5640550156600739, -260.3154719736058382 ) ) ;
#44860 = CARTESIAN_POINT ( 'NONE',  ( 37.73973963241286356, -293.6722737940024786, -253.3161059073749186 ) ) ;
#44861 = CARTESIAN_POINT ( 'NONE',  ( -33.51157017901221025, -292.4349377721255223, -197.4279968699894141 ) ) ;
#44862 = LINE ( 'NONE', #66210, #82029 ) ;
#44863 =( NAMED_UNIT ( * ) PLANE_ANGLE_UNIT ( ) SI_UNIT ( $, .RADIAN. ) );
#44864 = CARTESIAN_POINT ( 'NONE',  ( 161.2402580060632147, 217.6105062135258095, -202.4543169503909610 ) ) ;
#44865 = CARTESIAN_POINT ( 'NONE',  ( 25.77291357601318822, -288.5013954184609020, -227.4512683872464152 ) ) ;
#44866 = CARTESIAN_POINT ( 'NONE',  ( -19.11405058567864046, -280.3380690714490129, -350.3683826091709648 ) ) ;
#44867 = VERTEX_POINT ( 'NONE', #27050 ) ;
#44868 = CARTESIAN_POINT ( 'NONE',  ( -95.36951592401595690, -282.8441847773926270, -315.1811527220429525 ) ) ;
#44869 = CARTESIAN_POINT ( 'NONE',  ( -113.6955703002261089, -278.3464054398949656, -260.1664551931082769 ) ) ;
#44870 = CARTESIAN_POINT ( 'NONE',  ( 35.85318259912133243, -283.3511463421290273, -254.7265447461116139 ) ) ;
#44871 = CARTESIAN_POINT ( 'NONE',  ( 7.677621891900887618, -59.82691858394279905, -353.2347412010317385 ) ) ;
#44872 = CARTESIAN_POINT ( 'NONE',  ( -102.4257697418197353, -282.5996320843825060, -310.3944812501870274 ) ) ;
#44873 = CARTESIAN_POINT ( 'NONE',  ( -27.59742183241397129, -284.1966481620742684, -196.3550652468307192 ) ) ;
#44874 = CARTESIAN_POINT ( 'NONE',  ( 13.12379576613483323, -276.6085234987818353, -213.7796218371169630 ) ) ;
#44875 = CARTESIAN_POINT ( 'NONE',  ( -49.97071242924983636, -298.3789930052282671, -198.3993469524838531 ) ) ;
#44876 = CARTESIAN_POINT ( 'NONE',  ( -4.128678093487827994, -293.2895897531827814, -335.9354004423030347 ) ) ;
#44877 = CARTESIAN_POINT ( 'NONE',  ( -98.50033958787030031, -279.8260141020185756, -223.7249293083094983 ) ) ;
#44878 = CARTESIAN_POINT ( 'NONE',  ( 11.74770313617410444, -276.3479567014632607, -324.4596143623290914 ) ) ;
#44879 = CARTESIAN_POINT ( 'NONE',  ( -113.2404333110514045, -273.7744271896679606, -259.0041579536853078 ) ) ;
#44880 = CARTESIAN_POINT ( 'NONE',  ( -25.82999229414716069, -275.8291290068479498, -346.1831008886371706 ) ) ;
#44881 = CARTESIAN_POINT ( 'NONE',  ( -95.79658185063551912, -239.9132554249223972, -341.7037225619939136 ) ) ;
#44882 = CARTESIAN_POINT ( 'NONE',  ( -18.63779021769444100, -274.8112331595512501, -343.0443770915891264 ) ) ;
#44883 = CARTESIAN_POINT ( 'NONE',  ( -76.76256789907030509, -296.9938775006589822, -335.8795331689473187 ) ) ;
#44884 = DIRECTION ( 'NONE',  ( 0.000000000000000000, 0.000000000000000000, 1.000000000000000000 ) ) ;
#44885 = LINE ( 'NONE', #66234, #85002 ) ;
#44886 = CARTESIAN_POINT ( 'NONE',  ( -67.90074174454966283, -284.5426918370051226, -336.9972271879709638 ) ) ;
#44887 = CARTESIAN_POINT ( 'NONE',  ( -83.25287784326982887, -285.4310989093687567, -330.9758397337648717 ) ) ;
#44888 = CARTESIAN_POINT ( 'NONE',  ( -74.76517734613999266, -284.8882149780384907, -207.5648121906982908 ) ) ;
#44889 = CONICAL_SURFACE ( 'NONE', #4024, 2.241321557046427326, 0.09862129276975473147 ) ;
#44890 = CARTESIAN_POINT ( 'NONE',  ( -110.2858528267710625, -276.8057861783671001, -281.5678571466028757 ) ) ;
#44891 = CARTESIAN_POINT ( 'NONE',  ( -85.64790207335592243, -285.5894491232702421, -326.7293389164128712 ) ) ;
#44892 = CARTESIAN_POINT ( 'NONE',  ( -87.99325395927627369, -277.8083621993210386, -216.7637254420216379 ) ) ;
#44893 = CARTESIAN_POINT ( 'NONE',  ( -32.38598643313268610, -278.0680181076066333, -343.5527132183279946 ) ) ;
#44894 = FACE_OUTER_BOUND ( 'NONE', #7418, .T. ) ;
#44895 = CARTESIAN_POINT ( 'NONE',  ( -78.89521878112562092, -273.9677917405644507, -210.2056212678602094 ) ) ;
#44896 = CARTESIAN_POINT ( 'NONE',  ( 26.14142257911781186, -281.7817514731621600, -226.9779743120037665 ) ) ;
#44897 = CARTESIAN_POINT ( 'NONE',  ( -41.55948849069151407, -283.5961418111362491, -347.2361675200016293 ) ) ;
#44898 = ORIENTED_EDGE ( 'NONE', *, *, #24425, .T. ) ;
#44899 = ORIENTED_EDGE ( 'NONE', *, *, #34695, .F. ) ;
#44900 = CARTESIAN_POINT ( 'NONE',  ( 195.0934829612641295, 39.77032864624461439, 15.17998222329788760 ) ) ;
#44901 = CARTESIAN_POINT ( 'NONE',  ( 36.62432930176822765, -289.6219083200477939, -286.8317652917231726 ) ) ;
#44902 = CARTESIAN_POINT ( 'NONE',  ( -70.53168554395965373, -296.8000967899567968, -205.1472791797875743 ) ) ;
#44903 = CARTESIAN_POINT ( 'NONE',  ( -74.62220758075554272, -290.9180136745612231, -203.1043224092960884 ) ) ;
#44904 = CARTESIAN_POINT ( 'NONE',  ( 35.81013993305315068, -286.1485499826483192, -279.2782950993930058 ) ) ;
#44906 = CARTESIAN_POINT ( 'NONE',  ( -32.06294684805041584, -290.3594754125659847, -196.5234704348577282 ) ) ;
#44905 = CARTESIAN_POINT ( 'NONE',  ( -31.84531552763532858, -287.5563022883413851, -343.7958308776430840 ) ) ;
#44907 = CARTESIAN_POINT ( 'NONE',  ( -6.865557171864504760, -287.6663669500873084, -203.5765519488274720 ) ) ;
#44908 = CARTESIAN_POINT ( 'NONE',  ( -103.2310110255232303, -276.0760238941593343, -306.1884728315868642 ) ) ;
#44909 = CARTESIAN_POINT ( 'NONE',  ( 38.90169518151787287, -285.9671659966109587, -271.5592601806049515 ) ) ;
#44910 = CARTESIAN_POINT ( 'NONE',  ( 22.25623811635489346, -288.9287967970451518, -224.8089114094292142 ) ) ;
#44911 = CARTESIAN_POINT ( 'NONE',  ( -97.57567154493682438, -287.9389745409797001, -315.3479219858205624 ) ) ;
#44912 = CARTESIAN_POINT ( 'NONE',  ( -18.66409561926110072, -283.7470383120365796, -341.2272200174068644 ) ) ;
#44913 = CARTESIAN_POINT ( 'NONE',  ( -112.1840283378751195, -292.6485916650241279, -262.8461942793977073 ) ) ;
#44914 = CARTESIAN_POINT ( 'NONE',  ( 82.12347693879148380, -301.5478687382300222, -195.3203844934047311 ) ) ;
#44915 = EDGE_CURVE ( 'NONE', #65773, #87468, #49609, .T. ) ;
#44916 = FACE_OUTER_BOUND ( 'NONE', #18843, .T. ) ;
#44917 = CARTESIAN_POINT ( 'NONE',  ( -112.8714614705549621, -298.5173432895429642, -266.8274731023640811 ) ) ;
#44918 = CARTESIAN_POINT ( 'NONE',  ( -7.925157689368147906, -279.6448499745104641, -203.3603352654254479 ) ) ;
#44919 = CARTESIAN_POINT ( 'NONE',  ( 29.93413013003397793, -279.9906237221798051, -303.6295130106403803 ) ) ;
#44920 = CARTESIAN_POINT ( 'NONE',  ( -33.45325553772223515, -294.2015741049136750, -347.1142830203291396 ) ) ;
#44921 = CARTESIAN_POINT ( 'NONE',  ( -68.69167761721190857, -271.8742543503462912, -203.3013298842599283 ) ) ;
#44922 = CARTESIAN_POINT ( 'NONE',  ( -40.59265452147325703, -275.1731659805272443, -344.7428100305156704 ) ) ;
#44923 = CARTESIAN_POINT ( 'NONE',  ( -82.65076559589833494, -297.0010907282301105, -328.2907647318019713 ) ) ;
#44924 = CARTESIAN_POINT ( 'NONE',  ( 201.2104617360081704, 25.32700003806615996, 9.000000000000001776 ) ) ;
#44925 = CARTESIAN_POINT ( 'NONE',  ( -65.98933895103067471, -272.2593041037410444, -199.5097860267667329 ) ) ;
#44926 = CARTESIAN_POINT ( 'NONE',  ( -87.94750118390280136, -293.9878366632519828, -327.1152638649896858 ) ) ;
#44927 = CARTESIAN_POINT ( 'NONE',  ( -4.054016701165524594, -296.0295927006360444, -336.0052927053072835 ) ) ;
#44928 = DIRECTION ( 'NONE',  ( 0.000000000000000000, 0.000000000000000000, 1.000000000000000000 ) ) ;
#44929 = CARTESIAN_POINT ( 'NONE',  ( -26.17269284347905867, -295.7091510257329787, -342.6650252273538513 ) ) ;
#44930 = LINE ( 'NONE', #10345, #73221 ) ;
#44932 = CARTESIAN_POINT ( 'NONE',  ( -102.7681588153689631, -296.1118715700067128, -302.8540226837514524 ) ) ;
#44931 = CARTESIAN_POINT ( 'NONE',  ( -110.7515609803033811, -282.7896664967382776, -253.3493826984608575 ) ) ;
#44933 = CARTESIAN_POINT ( 'NONE',  ( -109.3029549977986647, -284.2036891710071700, -297.9063684378443213 ) ) ;
#44934 = CARTESIAN_POINT ( 'NONE',  ( -31.21536424951356281, -282.0489848413953951, -194.9981769272174574 ) ) ;
#44935 = CARTESIAN_POINT ( 'NONE',  ( -97.56120596943499379, -284.8610448793852470, -222.4095235575200320 ) ) ;
#44936 = CARTESIAN_POINT ( 'NONE',  ( -109.1474470674475157, -288.8244599768494254, -249.2452393417684107 ) ) ;
#44937 = CARTESIAN_POINT ( 'NONE',  ( 21.31550574532286291, -272.4094976428775681, -223.6242672951989618 ) ) ;
#44938 = CARTESIAN_POINT ( 'NONE',  ( -37.26364556790584004, -284.7379370136624743, -196.8554845851783455 ) ) ;
#44939 = CARTESIAN_POINT ( 'NONE',  ( -111.6914943778332230, -289.7093215302534759, -251.5039898923010924 ) ) ;
#44940 = CARTESIAN_POINT ( 'NONE',  ( 154.9842916688210153, 128.0000000000000568, 12.88888888888890349 ) ) ;
#44941 = CARTESIAN_POINT ( 'NONE',  ( -110.5960206018325920, -298.0300692622855081, -279.7273716327206330 ) ) ;
#44942 = CARTESIAN_POINT ( 'NONE',  ( -112.2126018767962989, -279.7842497935694723, -285.6885487601256841 ) ) ;
#44944 = CARTESIAN_POINT ( 'NONE',  ( 35.70862955333024757, -281.1954758924251792, -268.5872965196671203 ) ) ;
#44943 = CARTESIAN_POINT ( 'NONE',  ( -47.43672265507717611, -293.1999635024898225, -345.0370667288032678 ) ) ;
#44945 = CARTESIAN_POINT ( 'NONE',  ( 17.56303478610158564, -294.4606738631777603, -324.4227896493760568 ) ) ;
#44946 = CARTESIAN_POINT ( 'NONE',  ( -101.2865750478492970, -283.1691899289404546, -230.1073334596489701 ) ) ;
#44947 = CARTESIAN_POINT ( 'NONE',  ( -74.05182509965642623, -281.5645111741306437, -204.9595325700548472 ) ) ;
#44948 = CARTESIAN_POINT ( 'NONE',  ( -63.66472440017997769, -294.4625096249060334, -338.7559594641590479 ) ) ;
#44949 = CARTESIAN_POINT ( 'NONE',  ( -98.07044248564953648, -271.1552731524466253, -225.9798332660311928 ) ) ;
#44950 = VERTEX_POINT ( 'NONE', #47873 ) ;
#44951 = DIRECTION ( 'NONE',  ( -1.000000000000000000, 0.000000000000000000, 0.000000000000000000 ) ) ;
#44952 = CARTESIAN_POINT ( 'NONE',  ( 37.33221743365529477, -283.5082770428304570, -268.5183672133357504 ) ) ;
#44953 = CARTESIAN_POINT ( 'NONE',  ( -41.04860782057726709, -294.6076761692886521, -343.3411356771468377 ) ) ;
#44954 = DIRECTION ( 'NONE',  ( 1.000000000000000000, 0.000000000000000000, -0.000000000000000000 ) ) ;
#44955 = CARTESIAN_POINT ( 'NONE',  ( 10.59707575819633618, -273.9094976428776249, -330.5268031993606428 ) ) ;
#44956 = CARTESIAN_POINT ( 'NONE',  ( -83.47496131242027673, -272.6351060016030488, -208.8463336005037263 ) ) ;
#44957 = CARTESIAN_POINT ( 'NONE',  ( -110.3677456655047138, -290.4105546439384398, -268.4596414602061145 ) ) ;
#44958 = CARTESIAN_POINT ( 'NONE',  ( -59.96471228920603380, -281.2738750558607421, -200.1723814198369382 ) ) ;
#44959 = CARTESIAN_POINT ( 'NONE',  ( -92.63087372674183939, -274.8430728556506324, -221.4781178799393899 ) ) ;
#44960 = CARTESIAN_POINT ( 'NONE',  ( -64.94321019922705318, -285.0068630810242212, -341.4004993741073122 ) ) ;
#44961 = CARTESIAN_POINT ( 'NONE',  ( -24.79349950775172928, -279.0107329556851141, -198.0446387747937251 ) ) ;
#44962 = CARTESIAN_POINT ( 'NONE',  ( 21.60989744357675946, -278.1890651969129067, -316.7467717988959635 ) ) ;
#44963 = ORIENTED_EDGE ( 'NONE', *, *, #8073, .F. ) ;
#44964 = CARTESIAN_POINT ( 'NONE',  ( -70.12984044125136052, -273.4653903228503395, -200.6764969470301310 ) ) ;
#44965 = CARTESIAN_POINT ( 'NONE',  ( 11.86470794584511168, -294.6617638169417432, -214.4350054671125747 ) ) ;
#44966 = PLANE ( 'NONE',  #40000 ) ;
#44967 = CARTESIAN_POINT ( 'NONE',  ( 175.2296996224750103, 20.99999999999998934, 24.00000000000000355 ) ) ;
#44968 = CARTESIAN_POINT ( 'NONE',  ( 21.31505990980102538, -292.3461877180073429, -318.3365593364886195 ) ) ;
#44969 = CARTESIAN_POINT ( 'NONE',  ( -110.4030052300476115, -272.0958164305236551, -267.6287084019114104 ) ) ;
#44970 = DIRECTION ( 'NONE',  ( -0.000000000000000000, 1.000000000000000000, -0.000000000000000000 ) ) ;
#44971 = CARTESIAN_POINT ( 'NONE',  ( 1.331857138137925389, -294.0786443404025476, -204.5203201921196126 ) ) ;
#44972 = CARTESIAN_POINT ( 'NONE',  ( -112.3417001280813849, -275.0519495502701943, -270.3929463913696054 ) ) ;
#44973 = CARTESIAN_POINT ( 'NONE',  ( 35.48883471264535672, -289.3302962816950412, -253.1086760576881147 ) ) ;
#44974 = CARTESIAN_POINT ( 'NONE',  ( 37.41998447263363659, -273.4966165216893046, -266.0583256298650099 ) ) ;
#44975 = CARTESIAN_POINT ( 'NONE',  ( 35.78357977591105765, -277.2921194104836786, -256.4324554781686629 ) ) ;
#44976 = CARTESIAN_POINT ( 'NONE',  ( -12.55129066572806806, -292.8072579743591746, -340.6062287963176800 ) ) ;
#44977 = CARTESIAN_POINT ( 'NONE',  ( -14.62111816618705795, -282.2038194188187958, -198.0283185196263389 ) ) ;
#44978 = ORIENTED_EDGE ( 'NONE', *, *, #29709, .T. ) ;
#44979 = CARTESIAN_POINT ( 'NONE',  ( -51.02602017184861438, -282.8984557946668588, -342.1401583220393263 ) ) ;
#44980 = CARTESIAN_POINT ( 'NONE',  ( -100.2042186998935165, -279.0487491537156757, -314.2905644712399749 ) ) ;
#44981 = EDGE_CURVE ( 'NONE', #13368, #3752, #17563, .T. ) ;
#44982 = CARTESIAN_POINT ( 'NONE',  ( -19.02827411831646032, -281.6165672692053477, -344.7974214811313800 ) ) ;
#44983 = CARTESIAN_POINT ( 'NONE',  ( -101.8926164392937892, -278.9455216463430247, -312.0032410400955882 ) ) ;
#44984 = CARTESIAN_POINT ( 'NONE',  ( -3.019465798492313002, -278.1271277400308009, -338.5276424403434135 ) ) ;
#44985 = CARTESIAN_POINT ( 'NONE',  ( -37.37352853689063181, -282.5519495502701375, -200.3611179825600459 ) ) ;
#44986 = VERTEX_POINT ( 'NONE', #26585 ) ;
#44987 = CARTESIAN_POINT ( 'NONE',  ( -109.7736464647251182, -298.8030332313194322, -250.8535645650285062 ) ) ;
#44988 = CARTESIAN_POINT ( 'NONE',  ( -101.4004482277824195, -292.1184189522355155, -234.6099001427998871 ) ) ;
#44989 = CARTESIAN_POINT ( 'NONE',  ( -109.4148316350069052, -276.3213413071885611, -289.7856004683449100 ) ) ;
#44990 = CARTESIAN_POINT ( 'NONE',  ( -101.4343284784878847, -291.7689749532872838, -311.2759018222711802 ) ) ;
#44991 = CARTESIAN_POINT ( 'NONE',  ( -91.74347583773356973, -290.5987917589371250, -221.5126990191346010 ) ) ;
#44992 = CARTESIAN_POINT ( 'NONE',  ( 37.96456850763826196, -286.8617049278752233, -254.5336483576866158 ) ) ;
#44993 = DIRECTION ( 'NONE',  ( -1.000000000000000000, 0.000000000000000000, 0.000000000000000000 ) ) ;
#44994 = CARTESIAN_POINT ( 'NONE',  ( -109.2089677214262764, -282.7324230716570810, -287.1954419439665003 ) ) ;
#44995 = CARTESIAN_POINT ( 'NONE',  ( -109.9231648269188497, -292.6146997664095011, -254.7791904466284336 ) ) ;
#44996 = CARTESIAN_POINT ( 'NONE',  ( -70.27506980044306317, -284.0899403070055769, -204.4220786081634458 ) ) ;
#44997 = CARTESIAN_POINT ( 'NONE',  ( 36.18031487576281080, -282.8436658394828100, -268.5548571121732380 ) ) ;
#44998 = CARTESIAN_POINT ( 'NONE',  ( -70.52647021523173976, -290.4201997297916478, -339.5968794339055989 ) ) ;
#44999 = CARTESIAN_POINT ( 'NONE',  ( -59.75847031462780024, -280.2462658141396332, -200.7701734572789576 ) ) ;
#45000 = CARTESIAN_POINT ( 'NONE',  ( -11.27386834692455686, -291.1792002377596873, -198.2742817387639036 ) ) ;
#45001 = CARTESIAN_POINT ( 'NONE',  ( 20.15909876017686742, -287.6623731904183501, -219.3138034766267594 ) ) ;
#45002 = CARTESIAN_POINT ( 'NONE',  ( 39.64099133976078804, -288.0593048627596886, -271.5440799452276224 ) ) ;
#45003 = CARTESIAN_POINT ( 'NONE',  ( -49.42361886076759703, -286.0606446342503091, -198.3163748136984168 ) ) ;
#45004 = ORIENTED_EDGE ( 'NONE', *, *, #92815, .T. ) ;
#45005 = CYLINDRICAL_SURFACE ( 'NONE', #29266, 1.999999999999988454 ) ;
#45006 = CARTESIAN_POINT ( 'NONE',  ( 18.48916599484682521, -294.7043465154985711, -219.1437393988558142 ) ) ;
#45007 = CARTESIAN_POINT ( 'NONE',  ( -71.86657925686228054, -294.1837927747952790, -338.6350588064914291 ) ) ;
#45008 = CARTESIAN_POINT ( 'NONE',  ( -36.47537942012152001, -276.0998136476359264, -343.6037965660678424 ) ) ;
#45009 = EDGE_CURVE ( 'NONE', #71244, #17165, #55475, .T. ) ;
#45010 = CARTESIAN_POINT ( 'NONE',  ( -46.11000515357697083, -297.2922911212299937, -193.9645891778158386 ) ) ;
#45011 = CARTESIAN_POINT ( 'NONE',  ( 28.11113576304865447, -291.5758829128906200, -236.4991330379089902 ) ) ;
#45012 = CARTESIAN_POINT ( 'NONE',  ( -93.49883555591291895, -295.4691579200028286, -222.1301165406080997 ) ) ;
#45013 = CARTESIAN_POINT ( 'NONE',  ( -93.75482582498300133, -292.4199583252784009, -223.3873681428105442 ) ) ;
#45014 = CARTESIAN_POINT ( 'NONE',  ( 25.10399850599438665, -294.1035264581045112, -231.8621619403613749 ) ) ;
#45015 = CARTESIAN_POINT ( 'NONE',  ( 208.3080460680526755, 36.52560914003142045, 14.78771946819801109 ) ) ;
#45016 = CARTESIAN_POINT ( 'NONE',  ( -64.95430543207319829, -293.4118216271949109, -340.2861789718533601 ) ) ;
#45017 = CARTESIAN_POINT ( 'NONE',  ( -102.8666662774895428, -298.0654440227073110, -306.9560002683538187 ) ) ;
#45018 = CARTESIAN_POINT ( 'NONE',  ( -90.75618442156434185, -290.7740214440402724, -320.5380686947973459 ) ) ;
#45019 = CARTESIAN_POINT ( 'NONE',  ( -31.59645874093947171, -295.3110501249717572, -343.2060235448338403 ) ) ;
#45020 = CARTESIAN_POINT ( 'NONE',  ( 11.65469459019522702, -278.3558221822689802, -327.6128437602155827 ) ) ;
#45021 = CARTESIAN_POINT ( 'NONE',  ( -99.02030575490984177, -277.8423035465062867, -225.0726038609904265 ) ) ;
#45022 = CARTESIAN_POINT ( 'NONE',  ( -71.35024695003625084, -272.9634191520783588, -201.3920558591475185 ) ) ;
#45023 = CARTESIAN_POINT ( 'NONE',  ( 21.67221892397924066, -279.0056015145915467, -224.9678051746266476 ) ) ;
#45024 = CARTESIAN_POINT ( 'NONE',  ( -59.05448767232898888, -278.1756220060979672, -197.3200660267687852 ) ) ;
#45025 = EDGE_CURVE ( 'NONE', #87746, #58890, #12373, .T. ) ;
#45026 = CARTESIAN_POINT ( 'NONE',  ( -110.8672608630167673, -295.2586687192013528, -268.7051849345505730 ) ) ;
#45027 = CARTESIAN_POINT ( 'NONE',  ( -89.07483363196955395, -275.3254076992274122, -215.9889488845848575 ) ) ;
#45028 = CARTESIAN_POINT ( 'NONE',  ( -27.28435202728121212, -274.8346239058199103, -197.9033645069180238 ) ) ;
#45029 = CARTESIAN_POINT ( 'NONE',  ( 196.3996634987102539, 25.59933695287653777, 11.39947427447970441 ) ) ;
#45030 = CARTESIAN_POINT ( 'NONE',  ( -106.8402410552994297, -288.9508347281673650, -241.2345045657722267 ) ) ;
#45031 = CARTESIAN_POINT ( 'NONE',  ( -112.9249582457598393, -290.7368894666012125, -255.5896734205759344 ) ) ;
#45032 = CARTESIAN_POINT ( 'NONE',  ( -49.44964024417996740, -275.8984366418305854, -196.1235108769647582 ) ) ;
#45033 = CARTESIAN_POINT ( 'NONE',  ( -87.30590175267187192, -295.3534229674876315, -214.6510921349343164 ) ) ;
#45034 = CARTESIAN_POINT ( 'NONE',  ( -21.76872404554887552, -282.0545963758418111, -345.6049963776457048 ) ) ;
#45035 = CARTESIAN_POINT ( 'NONE',  ( 0.3351527144970434802, -280.5505321844422610, -335.2690112824063249 ) ) ;
#45036 = CARTESIAN_POINT ( 'NONE',  ( 196.1963538710216994, 282.2246705312485915, -40.00000000000000711 ) ) ;
#45037 = CARTESIAN_POINT ( 'NONE',  ( -37.53567607646679249, -290.8446289544783667, -196.9517884067832085 ) ) ;
#45038 = CARTESIAN_POINT ( 'NONE',  ( -110.8317405842020662, -282.8278344389742074, -259.8692433082197226 ) ) ;
#45039 = DIRECTION ( 'NONE',  ( -1.000000000000000000, -0.000000000000000000, -0.000000000000000000 ) ) ;
#45040 = ADVANCED_FACE ( 'NONE', ( #85279 ), #84792, .F. ) ;
#45041 = LINE ( 'NONE', #58368, #76025 ) ;
#45042 = CARTESIAN_POINT ( 'NONE',  ( 36.89081888944549803, -291.4145776736198741, -259.6590728838539235 ) ) ;
#45043 = CARTESIAN_POINT ( 'NONE',  ( -40.52004547041168081, -278.6928795587459149, -344.1052492624293677 ) ) ;
#45044 = CARTESIAN_POINT ( 'NONE',  ( -95.02556474304107326, -285.0719612038552668, -320.7652892621512706 ) ) ;
#45046 = CARTESIAN_POINT ( 'NONE',  ( -12.02198274293792046, -286.3910893566877007, -201.8927901839605852 ) ) ;
#45045 = CARTESIAN_POINT ( 'NONE',  ( -92.11121905872373361, -271.3571875064064329, -218.2882905403421319 ) ) ;
#45047 = CARTESIAN_POINT ( 'NONE',  ( 34.07667785116749570, -276.7451721625916434, -252.6187899053837214 ) ) ;
#45048 = CARTESIAN_POINT ( 'NONE',  ( -72.91158753461822073, -278.3390957636441954, -334.3081891941630488 ) ) ;
#45049 = CARTESIAN_POINT ( 'NONE',  ( -86.97831698256817390, -285.7427942221026456, -326.6550523934734542 ) ) ;
#45050 = AXIS2_PLACEMENT_3D ( 'NONE', #58291, #21352, #64947 ) ;
#45051 = B_SPLINE_CURVE_WITH_KNOTS ( 'NONE', 3,
 ( #16485, #40104, #32574, #60062, #67161, #53396, #11250, #25001 ),
 .UNSPECIFIED., .F., .F.,
 ( 4, 2, 2, 4 ),
 ( 0.000000000000000000, 0.004397459120518200718, 0.006596188680777302811, 0.008794918241036404905 ),
 .UNSPECIFIED. ) ;
#45052 = ORIENTED_EDGE ( 'NONE', *, *, #203, .F. ) ;
#45053 = DIRECTION ( 'NONE',  ( 0.000000000000000000, 0.000000000000000000, -1.000000000000000000 ) ) ;
#45054 = CARTESIAN_POINT ( 'NONE',  ( -65.60547335084395115, -295.2450061577498559, -342.0004692933496244 ) ) ;
#45055 = CARTESIAN_POINT ( 'NONE',  ( 23.31371403259033670, -288.9362955945862268, -226.7680637701012643 ) ) ;
#45056 = CARTESIAN_POINT ( 'NONE',  ( 197.1933712184921603, 24.89666632552609826, 12.64285714285712992 ) ) ;
#45057 = CARTESIAN_POINT ( 'NONE',  ( -55.63300648810263738, -286.7666405000204577, -350.3538533559490702 ) ) ;
#45058 = CARTESIAN_POINT ( 'NONE',  ( -77.31959820859130161, -278.4500164629433812, -204.8530250470102203 ) ) ;
#45059 = CARTESIAN_POINT ( 'NONE',  ( -102.5208738600124576, -289.4738042523592867, -230.7864546700232893 ) ) ;
#45060 = CARTESIAN_POINT ( 'NONE',  ( -86.20016995144860061, -286.8802959206793730, -215.1244492291654922 ) ) ;
#45061 = CARTESIAN_POINT ( 'NONE',  ( -105.3823149106760013, -280.6982198208115733, -241.2329743553731873 ) ) ;
#45062 = CARTESIAN_POINT ( 'NONE',  ( 34.52453284190504235, -289.3095206890816371, -296.4738004929021145 ) ) ;
#45063 = CARTESIAN_POINT ( 'NONE',  ( 35.70260027967242422, -283.3338264577108134, -253.3455124549539619 ) ) ;
#45064 = CARTESIAN_POINT ( 'NONE',  ( 36.49406691238041844, -275.9934369045114977, -292.2543696306888705 ) ) ;
#45065 = CARTESIAN_POINT ( 'NONE',  ( -82.92914717370662459, -295.4455451274745315, -211.1886760348594407 ) ) ;
#45066 = CARTESIAN_POINT ( 'NONE',  ( -103.4105036632464589, -278.9023045922635333, -230.7111070666566661 ) ) ;
#45067 = CARTESIAN_POINT ( 'NONE',  ( -97.27393865318751409, -299.0793475167554334, -226.1871146775593786 ) ) ;
#45068 = CARTESIAN_POINT ( 'NONE',  ( 157.7437329832453088, 18.12362412296306502, 11.08836552221218419 ) ) ;
#45069 = CARTESIAN_POINT ( 'NONE',  ( -110.4683760289727132, -281.2662352645559167, -253.7030783399848985 ) ) ;
#45070 = CARTESIAN_POINT ( 'NONE',  ( -16.03966176233213758, -272.5636453452710271, -197.3668200790013429 ) ) ;
#45071 = DIRECTION ( 'NONE',  ( -0.000000000000000000, -0.000000000000000000, -1.000000000000000000 ) ) ;
#45072 = CARTESIAN_POINT ( 'NONE',  ( -39.69694010020822361, -279.5294636104500228, -197.3250209367067498 ) ) ;
#45073 = CARTESIAN_POINT ( 'NONE',  ( 24.99480058169025654, -276.1641458837946175, -225.8171231697601797 ) ) ;
#45074 = CARTESIAN_POINT ( 'NONE',  ( 32.96227231253141099, -280.2165964070200630, -239.5362632160081944 ) ) ;
#45075 = CARTESIAN_POINT ( 'NONE',  ( -29.03747700862987813, -290.7056084709684001, -343.9071164531536624 ) ) ;
#45076 = CARTESIAN_POINT ( 'NONE',  ( 7.462758075997037110, -300.1235921870971310, -194.0430978029753817 ) ) ;
#45077 = CARTESIAN_POINT ( 'NONE',  ( -78.00474998966045348, -298.7235478835002027, -205.4417441867235823 ) ) ;
#45078 = CARTESIAN_POINT ( 'NONE',  ( 30.38723081137278470, -295.1315086119431044, -238.4140699798435321 ) ) ;
#45079 = CARTESIAN_POINT ( 'NONE',  ( 13.13500835329171323, -280.3445444974924499, -325.6072067582007321 ) ) ;
#45080 = CARTESIAN_POINT ( 'NONE',  ( 37.12735433239998883, -283.4485485312707169, -268.5241133501003219 ) ) ;
#45081 = CARTESIAN_POINT ( 'NONE',  ( -102.1332017961093044, -271.0701969018276145, -233.1909701514428264 ) ) ;
#45082 = CARTESIAN_POINT ( 'NONE',  ( -66.46442418998211110, -288.3629186996745943, -337.6916125377663889 ) ) ;
#45083 = CARTESIAN_POINT ( 'NONE',  ( 195.4004353698729233, 278.2073661579722739, -125.7789885842296229 ) ) ;
#45084 = ORIENTED_EDGE ( 'NONE', *, *, #56630, .T. ) ;
#45085 = CARTESIAN_POINT ( 'NONE',  ( -34.70546589103574320, -287.5943666202287545, -346.7264017395094697 ) ) ;
#45086 = CARTESIAN_POINT ( 'NONE',  ( -56.07510881051521068, -288.9667453944787781, -340.9909315912261150 ) ) ;
#45087 = VERTEX_POINT ( 'NONE', #56419 ) ;
#45088 = CARTESIAN_POINT ( 'NONE',  ( -114.0317253597367966, -285.6363934468266734, -269.9970591442449290 ) ) ;
#45089 = CARTESIAN_POINT ( 'NONE',  ( 13.50833973054514736, -275.1216850459047691, -217.9553842017454031 ) ) ;
#45090 = CARTESIAN_POINT ( 'NONE',  ( 35.99542715519331892, -292.1896969670812609, -247.9299282753309512 ) ) ;
#45091 = CARTESIAN_POINT ( 'NONE',  ( -18.93474397697080747, -283.4727574689422340, -345.0785568775221464 ) ) ;
#45092 = CARTESIAN_POINT ( 'NONE',  ( 38.10619305724723205, -282.9238836683733211, -258.6030662491696717 ) ) ;
#45093 = CARTESIAN_POINT ( 'NONE',  ( 15.74202247268584287, -282.6582080530882877, -326.1093259026982309 ) ) ;
#45094 = CARTESIAN_POINT ( 'NONE',  ( 0.4072476377180442864, -280.9030664345736454, -207.7957530287029329 ) ) ;
#45095 = CARTESIAN_POINT ( 'NONE',  ( -82.13390479932374433, -293.1952119285919025, -326.4764044574609443 ) ) ;
#45096 = CARTESIAN_POINT ( 'NONE',  ( 185.9028033071117250, 263.4317942799772254, -153.4147630842123249 ) ) ;
#45097 = ORIENTED_EDGE ( 'NONE', *, *, #18207, .F. ) ;
#45098 = CARTESIAN_POINT ( 'NONE',  ( 1.852823970357027950, -278.5270857293184008, -334.1700977949444109 ) ) ;
#45099 = CARTESIAN_POINT ( 'NONE',  ( -64.53519957046890454, -182.2411953823292095, -361.8101628955362798 ) ) ;
#45100 = CARTESIAN_POINT ( 'NONE',  ( -57.92555012658558411, -297.1277065808350244, -200.2169964387891525 ) ) ;
#45101 = CARTESIAN_POINT ( 'NONE',  ( 28.00340991085941766, -292.5269609810044358, -229.6458648847749942 ) ) ;
#45102 = CARTESIAN_POINT ( 'NONE',  ( -62.10227321110217957, -183.1506894771875977, -358.8537685376919057 ) ) ;
#45104 = CARTESIAN_POINT ( 'NONE',  ( -31.83174353413192037, -287.3814744144756901, -344.0063226517897306 ) ) ;
#45103 = CARTESIAN_POINT ( 'NONE',  ( -46.04460757818183936, -296.5185567687674961, -194.4475770690140735 ) ) ;
#45105 = CARTESIAN_POINT ( 'NONE',  ( -3.757000792347619189, -296.4646659525153609, -336.5790818086119884 ) ) ;
#45106 = CARTESIAN_POINT ( 'NONE',  ( -65.29621206716205961, -286.9942735139140950, -202.3379125434092884 ) ) ;
#45107 = ORIENTED_EDGE ( 'NONE', *, *, #13517, .T. ) ;
#45108 = CARTESIAN_POINT ( 'NONE',  ( 19.36399297508274842, -295.1996923153037073, -322.1810412333751970 ) ) ;
#45109 = CARTESIAN_POINT ( 'NONE',  ( -82.82813988057930032, -284.1857026193267188, -327.6009592705700015 ) ) ;
#45110 = CARTESIAN_POINT ( 'NONE',  ( -93.36183478589195772, -296.0637447864519913, -218.0367225798047457 ) ) ;
#45111 = CARTESIAN_POINT ( 'NONE',  ( -42.05429359205262330, -292.7969977072485790, -193.6672441497979378 ) ) ;
#45112 = CARTESIAN_POINT ( 'NONE',  ( 39.65003539072439054, -294.0437803179181060, -270.3037412548086991 ) ) ;
#45113 = CARTESIAN_POINT ( 'NONE',  ( -70.22261759564466388, -291.7729128456326180, -205.1856220425692072 ) ) ;
#45114 = VERTEX_POINT ( 'NONE', #68746 ) ;
#45115 = CARTESIAN_POINT ( 'NONE',  ( 159.4572718888341285, 15.57755555264331271, 9.020884447463151545 ) ) ;
#45116 = CARTESIAN_POINT ( 'NONE',  ( -46.01241218824748813, -299.8037154092144760, -195.0940984342157662 ) ) ;
#45117 = CARTESIAN_POINT ( 'NONE',  ( -3.985067533389323291, -273.2772448064072819, -201.3876818897225576 ) ) ;
#45118 = ORIENTED_EDGE ( 'NONE', *, *, #42879, .T. ) ;
#45119 = ADVANCED_FACE ( 'NONE', ( #86202 ), #20889, .T. ) ;
#45120 = CARTESIAN_POINT ( 'NONE',  ( 22.58911660123931142, -275.7071640074176457, -318.6294844103896367 ) ) ;
#45121 = AXIS2_PLACEMENT_3D ( 'NONE', #92092, #41899, #56623 ) ;
#45122 = CARTESIAN_POINT ( 'NONE',  ( -105.1062881034619210, -271.3420952495238794, -241.0015554501175643 ) ) ;
#45123 = CARTESIAN_POINT ( 'NONE',  ( -111.5133269532062030, -280.3727286162280734, -273.4328034817352773 ) ) ;
#45124 = CARTESIAN_POINT ( 'NONE',  ( -8.276533417617695676, -274.8070813492064985, -338.6836097568491937 ) ) ;
#45125 = CARTESIAN_POINT ( 'NONE',  ( -55.40615617779363333, -299.0197282926562252, -199.1691780537907448 ) ) ;
#45126 = CARTESIAN_POINT ( 'NONE',  ( -69.60538474506611806, -274.5578717543543803, -204.6156762861326115 ) ) ;
#45127 = CARTESIAN_POINT ( 'NONE',  ( 52.39383663106224986, -300.7580296876250827, -194.1371264346019814 ) ) ;
#45128 = CARTESIAN_POINT ( 'NONE',  ( -64.28785766289425396, -271.7224101341118967, -199.9745765261779127 ) ) ;
#45129 = CARTESIAN_POINT ( 'NONE',  ( -55.82107744325771392, -295.9477058935856917, -341.1412566901580590 ) ) ;
#45130 = CARTESIAN_POINT ( 'NONE',  ( -34.81905062895935288, -290.6591863297728082, -196.8151380928799199 ) ) ;
#45131 = DIRECTION ( 'NONE',  ( 0.000000000000000000, 0.000000000000000000, -1.000000000000000000 ) ) ;
#45132 = CARTESIAN_POINT ( 'NONE',  ( -1.490841160238415286, -277.0820623854073119, -338.4363911341824291 ) ) ;
#45133 = CARTESIAN_POINT ( 'NONE',  ( 29.08516528249147726, -275.3092062763931267, -239.9655620876989701 ) ) ;
#45134 = CARTESIAN_POINT ( 'NONE',  ( -110.4497822562913569, -283.5240382705361526, -247.6328437178648869 ) ) ;
#45135 = CARTESIAN_POINT ( 'NONE',  ( -83.04969576014880772, -297.6758264022215599, -330.0992282372083650 ) ) ;
#45136 = PLANE ( 'NONE',  #23300 ) ;
#45137 = CARTESIAN_POINT ( 'NONE',  ( -22.41692696702421728, -285.4451909607376479, -198.6861297509074120 ) ) ;
#45138 = CARTESIAN_POINT ( 'NONE',  ( -55.28970393811566453, -281.2823606132413943, -343.3535667886935698 ) ) ;
#45139 = EDGE_CURVE ( 'NONE', #25330, #31000, #79826, .T. ) ;
#45140 = ADVANCED_FACE ( 'NONE', ( #6219 ), #20886, .T. ) ;
#45141 = CARTESIAN_POINT ( 'NONE',  ( -74.54171139353850606, -275.7942126176051261, -334.3465317551691669 ) ) ;
#45142 = CARTESIAN_POINT ( 'NONE',  ( -40.54947208601370789, -275.6679677826193711, -343.8929667267901209 ) ) ;
#45143 = CARTESIAN_POINT ( 'NONE',  ( -85.87190686309902787, -281.3805979028120419, -213.1114240415199674 ) ) ;
#45144 = CARTESIAN_POINT ( 'NONE',  ( 36.03957926435236914, -276.7372576975240577, -268.8385089166466742 ) ) ;
#45145 = DIRECTION ( 'NONE',  ( -0.000000000000000000, -0.000000000000000000, -1.000000000000000000 ) ) ;
#45146 = CARTESIAN_POINT ( 'NONE',  ( -15.98186973581476522, -272.7236324264439986, -197.1613009186945362 ) ) ;
#45147 = CARTESIAN_POINT ( 'NONE',  ( -103.1998488902101485, -281.0330144565799060, -234.1294651699267888 ) ) ;
#45148 = DIRECTION ( 'NONE',  ( 0.000000000000000000, 0.000000000000000000, -1.000000000000000000 ) ) ;
#45149 = CARTESIAN_POINT ( 'NONE',  ( -32.42500672069236600, -288.0338125280613326, -194.9483283104614770 ) ) ;
#45150 = PRESENTATION_STYLE_ASSIGNMENT (( #38046 ) ) ;
#45151 = CARTESIAN_POINT ( 'NONE',  ( -112.0305735846379065, -288.6465747594858158, -262.9945332178206741 ) ) ;
#45152 = CARTESIAN_POINT ( 'NONE',  ( 175.2296996224749250, 250.0000000000000568, -24.99999999999999289 ) ) ;
#45153 = CARTESIAN_POINT ( 'NONE',  ( -104.8259387609394366, -271.6270037598856675, -241.1268748806968176 ) ) ;
#45154 = CARTESIAN_POINT ( 'NONE',  ( -70.75583332890995791, -289.7461448569948743, -204.0711399638371404 ) ) ;
#45155 = CARTESIAN_POINT ( 'NONE',  ( 197.9738562182569694, 291.4636489450775798, -54.00000000000003553 ) ) ;
#45156 = CARTESIAN_POINT ( 'NONE',  ( 199.0143093133017373, 16.83012701892205598, -10.00000000000000000 ) ) ;
#45157 = CARTESIAN_POINT ( 'NONE',  ( -2.137956578368298999, -287.0745336519088937, -338.0619613635256542 ) ) ;
#45158 = CARTESIAN_POINT ( 'NONE',  ( -108.3639379111494918, -282.4438314177967868, -297.5229566074983723 ) ) ;
#45159 = CARTESIAN_POINT ( 'NONE',  ( -98.29953875658031848, -291.1102732204710719, -230.1053603160897296 ) ) ;
#45160 = CARTESIAN_POINT ( 'NONE',  ( 11.68498045918677875, -282.1741220505050478, -215.4816181093974592 ) ) ;
#45161 = CARTESIAN_POINT ( 'NONE',  ( 34.86457395050867092, -282.5100915984523340, -282.1448232936455156 ) ) ;
#45162 = CARTESIAN_POINT ( 'NONE',  ( -102.3660952171709084, -292.0243634817274483, -308.5462183513867558 ) ) ;
#45163 = CARTESIAN_POINT ( 'NONE',  ( -113.0482804226602696, -273.0633504042322102, -256.1387965711674610 ) ) ;
#45164 = CARTESIAN_POINT ( 'NONE',  ( -34.74133241795624372, -287.0995648637727982, -345.8763633856726756 ) ) ;
#45165 = CARTESIAN_POINT ( 'NONE',  ( 39.31730914938719224, -275.4548428485513796, -262.5803437234296211 ) ) ;
#45166 = CARTESIAN_POINT ( 'NONE',  ( -78.17554969086438632, -293.4799359874670586, -207.8755714062629352 ) ) ;
#45167 = DIRECTION ( 'NONE',  ( 0.000000000000000000, 0.000000000000000000, 1.000000000000000000 ) ) ;
#45168 = CARTESIAN_POINT ( 'NONE',  ( 21.27581636871892101, -283.4090924074130839, -223.5744983911110353 ) ) ;
#45169 = CARTESIAN_POINT ( 'NONE',  ( -102.0410611639040326, -276.0402284917197449, -308.7257748394039254 ) ) ;
#45170 = DIRECTION ( 'NONE',  ( -0.8457827187922972723, -0.5335274993777825436, -0.000000000000000000 ) ) ;
#45171 = CARTESIAN_POINT ( 'NONE',  ( -54.39609823113228515, -296.2364642377705763, -196.0941137428946206 ) ) ;
#45172 = CARTESIAN_POINT ( 'NONE',  ( -2.858256813195671597, -273.8693321143777553, -205.9034977537036752 ) ) ;
#45173 = CARTESIAN_POINT ( 'NONE',  ( -103.4590441213144629, -291.6354102548813216, -302.9065412210857176 ) ) ;
#45174 = CARTESIAN_POINT ( 'NONE',  ( -14.78528043257007418, -293.2929906924616716, -200.6860408154362005 ) ) ;
#45175 = CARTESIAN_POINT ( 'NONE',  ( -79.91016644144995951, -287.2280987407146426, -209.7515123138486217 ) ) ;
#45176 = CARTESIAN_POINT ( 'NONE',  ( -4.871144274710508704, -293.8966889868850672, -201.1927054094255425 ) ) ;
#45177 = CARTESIAN_POINT ( 'NONE',  ( 8.623319933707730200, -295.7521033646198134, -331.5208694714384023 ) ) ;
#45178 = CARTESIAN_POINT ( 'NONE',  ( 34.90804216963066153, -293.2477622781119635, -259.9220211623784849 ) ) ;
#45179 = CARTESIAN_POINT ( 'NONE',  ( 34.95045258370333130, -289.2954485910140647, -250.3900061662970984 ) ) ;
#45180 = CARTESIAN_POINT ( 'NONE',  ( 38.42595106142651673, -281.8913462562447307, -284.1552629618122410 ) ) ;
#45181 = CARTESIAN_POINT ( 'NONE',  ( -77.41760543113989002, -295.5988218694389502, -206.3046115909482694 ) ) ;
#45182 = CARTESIAN_POINT ( 'NONE',  ( -104.0393957065789294, -284.8868602709550828, -231.7788981355775491 ) ) ;
#45183 = CARTESIAN_POINT ( 'NONE',  ( 25.15719256819412308, -276.9789252480536561, -229.5476984485566732 ) ) ;
#45184 = CARTESIAN_POINT ( 'NONE',  ( -52.15415638363281658, -284.6531892598639502, -198.4742510087044707 ) ) ;
#45185 = CARTESIAN_POINT ( 'NONE',  ( 37.60438749050560858, -285.6031122645583764, -274.3428293336386332 ) ) ;
#45186 = CARTESIAN_POINT ( 'NONE',  ( -112.4887899456751086, -276.8195169561793705, -260.3078896419380044 ) ) ;
#45187 = FACE_OUTER_BOUND ( 'NONE', #60970, .T. ) ;
#45188 = CARTESIAN_POINT ( 'NONE',  ( -96.62108632582739176, -284.6567839485662716, -227.6321340575879901 ) ) ;
#45189 = CARTESIAN_POINT ( 'NONE',  ( -2.584091417435443905, -281.7065309206264487, -202.0828801514105066 ) ) ;
#45190 = CARTESIAN_POINT ( 'NONE',  ( -78.02191298294135891, -288.6430846323341370, -335.5225966575035272 ) ) ;
#45191 = CARTESIAN_POINT ( 'NONE',  ( 2.128938100842102887, -296.2763321718879297, -333.0320720919074802 ) ) ;
#45192 = CARTESIAN_POINT ( 'NONE',  ( -28.67161096172971568, -278.5442133670671865, -346.1192893458318736 ) ) ;
#45193 = CARTESIAN_POINT ( 'NONE',  ( 18.55442737433081390, -277.5843618685881324, -322.6001953383675414 ) ) ;
#45194 = CARTESIAN_POINT ( 'NONE',  ( -109.4923855583653989, -278.2390031494974210, -281.4642074827985994 ) ) ;
#45195 = CARTESIAN_POINT ( 'NONE',  ( -89.41943742115684302, -299.3172587378270464, -216.5492110200560489 ) ) ;
#45196 = CARTESIAN_POINT ( 'NONE',  ( 26.52840834090303090, -285.0279146709298743, -231.3657635262516123 ) ) ;
#45197 = CARTESIAN_POINT ( 'NONE',  ( -103.0976650903270553, -291.6446608309042858, -308.9698980875317034 ) ) ;
#45198 = CARTESIAN_POINT ( 'NONE',  ( -12.91816565755876134, -293.6476051672784138, -339.5356289783023271 ) ) ;
#45199 = ORIENTED_EDGE ( 'NONE', *, *, #80212, .T. ) ;
#45200 = CARTESIAN_POINT ( 'NONE',  ( 33.79505645823167015, -293.4368859832928820, -286.8979776332712390 ) ) ;
#45201 = CARTESIAN_POINT ( 'NONE',  ( -68.21698315878484209, -292.7357517187491567, -200.1456008121224386 ) ) ;
#45202 = CARTESIAN_POINT ( 'NONE',  ( -110.2693882551973559, -279.1280336688301986, -276.0951271893612784 ) ) ;
#45203 = ADVANCED_FACE ( 'NONE', ( #47 ), #51156, .T. ) ;
#45204 = CARTESIAN_POINT ( 'NONE',  ( -104.0191940012461629, -272.1076835389779376, -232.2159098541459343 ) ) ;
#45205 = CARTESIAN_POINT ( 'NONE',  ( 24.61621338543899284, -287.5977422319871835, -224.8141121545608883 ) ) ;
#45206 = B_SPLINE_CURVE_WITH_KNOTS ( 'NONE', 3,
 ( #81685, #9728, #16834, #38607, #67511, #2641, #59947, #23935, #42542, #86099, #91798, #20326 ),
 .UNSPECIFIED., .F., .F.,
 ( 4, 2, 2, 2, 2, 4 ),
 ( 0.000000000000000000, 0.002337776193942625591, 0.004675552387885251182, 0.007013328581827875906, 0.008182216678799194773, 0.009351104775770512773 ),
 .UNSPECIFIED. ) ;
#45207 = CARTESIAN_POINT ( 'NONE',  ( -51.67720643867760089, -289.5640194169581605, -345.9933700332452418 ) ) ;
#45208 = CARTESIAN_POINT ( 'NONE',  ( -79.32490777258617243, -285.8014683859145180, -210.5537660729611105 ) ) ;
#45209 = DIRECTION ( 'NONE',  ( 0.000000000000000000, 0.000000000000000000, 1.000000000000000000 ) ) ;
#45210 = CARTESIAN_POINT ( 'NONE',  ( 192.1024244148038918, 278.6331814114806207, -125.0969603314121201 ) ) ;
#45211 = CARTESIAN_POINT ( 'NONE',  ( -98.16163818206972280, -246.2973920797244887, -331.2694274904645795 ) ) ;
#45212 = CARTESIAN_POINT ( 'NONE',  ( -29.70671712946214882, -276.1503186283218838, -343.1741368637249820 ) ) ;
#45213 = CARTESIAN_POINT ( 'NONE',  ( -74.18045072629446679, -276.4745726304826121, -333.7419709915359931 ) ) ;
#45214 = CARTESIAN_POINT ( 'NONE',  ( -67.52344105919280537, -273.3336134654401803, -199.5458173340413737 ) ) ;
#45215 = CARTESIAN_POINT ( 'NONE',  ( 86.16957582609755661, 81.18500878458667103, -299.8392340653068118 ) ) ;
#45216 = CARTESIAN_POINT ( 'NONE',  ( -100.0708240539403135, -276.6542903988497528, -314.1601509010688460 ) ) ;
#45217 = CARTESIAN_POINT ( 'NONE',  ( -65.21070511493633148, -297.1715164502279549, -341.0666820218505109 ) ) ;
#45218 = CARTESIAN_POINT ( 'NONE',  ( -75.01671131628461353, -292.0283216296084561, -207.7034720250236433 ) ) ;
#45219 = CARTESIAN_POINT ( 'NONE',  ( -80.54270086535738926, -298.2858554099896651, -206.7531993858468695 ) ) ;
#45220 = CARTESIAN_POINT ( 'NONE',  ( -37.25995188159799909, -298.5454960940853653, -193.4218861848133599 ) ) ;
#45221 = CARTESIAN_POINT ( 'NONE',  ( -107.6022320872742597, -296.4569541852046086, -290.1716619763398057 ) ) ;
#45222 = ORIENTED_EDGE ( 'NONE', *, *, #31573, .F. ) ;
#45223 = LINE ( 'NONE', #66124, #43210 ) ;
#45224 = CARTESIAN_POINT ( 'NONE',  ( -110.0481147711410159, -280.2095909619072813, -290.9303053588366765 ) ) ;
#45225 = CARTESIAN_POINT ( 'NONE',  ( -34.48753625672294021, -282.5248316686867156, -347.2466215055856651 ) ) ;
#45226 = CARTESIAN_POINT ( 'NONE',  ( -108.2751534594444536, -279.8757811649951464, -251.8003907085040112 ) ) ;
#45227 = CARTESIAN_POINT ( 'NONE',  ( -113.3644698981806158, -280.3323564312751159, -268.7780245387174318 ) ) ;
#45228 = CARTESIAN_POINT ( 'NONE',  ( -89.72150370778508943, -271.7763627424086508, -218.5242206126879694 ) ) ;
#45229 = LINE ( 'NONE', #17781, #77447 ) ;
#45230 = CARTESIAN_POINT ( 'NONE',  ( 159.4851178187871312, 3.000000000000000000, 10.00000000000000000 ) ) ;
#45231 = CARTESIAN_POINT ( 'NONE',  ( -41.05330788521634844, -280.1708210584948802, -197.4555353953860788 ) ) ;
#45232 = CARTESIAN_POINT ( 'NONE',  ( 38.76283091420440741, -276.2221955361566756, -259.7658749341599105 ) ) ;
#45233 = CARTESIAN_POINT ( 'NONE',  ( 32.84101506552177341, -277.2087980024358558, -243.9151894687832680 ) ) ;
#45234 = CARTESIAN_POINT ( 'NONE',  ( 37.01424852486154293, -274.3493631398964681, -288.0185317296443372 ) ) ;
#45235 = ORIENTED_EDGE ( 'NONE', *, *, #86265, .F. ) ;
#45236 = LINE ( 'NONE', #38136, #21773 ) ;
#45237 = CARTESIAN_POINT ( 'NONE',  ( 37.16449658841762016, -283.3835796849227222, -258.7436466575366580 ) ) ;
#45238 = CARTESIAN_POINT ( 'NONE',  ( -91.78650233036469785, -290.4473968438287557, -221.4714791713576858 ) ) ;
#45239 = CARTESIAN_POINT ( 'NONE',  ( 34.76153699912342887, -286.5623655861349448, -243.6321826845998828 ) ) ;
#45240 = CARTESIAN_POINT ( 'NONE',  ( -96.74831270752116552, -282.1813059380716027, -314.5066545328163556 ) ) ;
#45242 = CARTESIAN_POINT ( 'NONE',  ( 33.65420008368713667, -285.3405648149401941, -247.9376844576008523 ) ) ;
#45241 = CARTESIAN_POINT ( 'NONE',  ( 12.30091423030655662, -280.9193401043354470, -324.6840942958812093 ) ) ;
#45243 = VECTOR ( 'NONE', #47625, 1000.000000000000000 ) ;
#45244 = CARTESIAN_POINT ( 'NONE',  ( -30.23915376342894135, -281.3489422889599041, -197.2578755905713592 ) ) ;
#45245 = CARTESIAN_POINT ( 'NONE',  ( -105.0270502363382406, -270.9772121191051042, -238.0548643102111726 ) ) ;
#45246 = CARTESIAN_POINT ( 'NONE',  ( -52.77570573118055819, -281.6464738944534361, -345.0356331423077449 ) ) ;
#45247 = CARTESIAN_POINT ( 'NONE',  ( 35.16963451458115486, -295.7985704197388941, -289.5211545130006243 ) ) ;
#45248 = CONICAL_SURFACE ( 'NONE', #4453, 4.999999999999990230, 1.029744258676656754 ) ;
#45249 = CARTESIAN_POINT ( 'NONE',  ( -82.20262215928330818, -287.4423929164352671, -209.9842883921245971 ) ) ;
#45250 = FACE_OUTER_BOUND ( 'NONE', #46570, .T. ) ;
#45251 = CARTESIAN_POINT ( 'NONE',  ( -25.27593629765922145, -294.1249765053227634, -195.7706927332011446 ) ) ;
#45252 = CARTESIAN_POINT ( 'NONE',  ( 35.78947479807442988, -273.3376967054872466, -253.6653443411174180 ) ) ;
#45253 = EDGE_CURVE ( 'NONE', #47701, #52349, #43134, .T. ) ;
#45254 = CARTESIAN_POINT ( 'NONE',  ( -59.98945543448800777, -288.5355610431782338, -343.7861682017015141 ) ) ;
#45255 = CARTESIAN_POINT ( 'NONE',  ( 31.32248278641987937, -292.3114859966649988, -297.5502463081921860 ) ) ;
#45256 = CARTESIAN_POINT ( 'NONE',  ( -43.34342893628492277, -268.6218111412664484, -433.7479087153366208 ) ) ;
#45257 = CARTESIAN_POINT ( 'NONE',  ( -108.6546515332806422, -277.0034601100138616, -288.1811759551610521 ) ) ;
#45258 = CARTESIAN_POINT ( 'NONE',  ( -106.1149816647575079, -294.3235976247425469, -298.3093062014407337 ) ) ;
#45259 = CARTESIAN_POINT ( 'NONE',  ( -104.4915344164712536, -291.4664256507214759, -300.3555002621342283 ) ) ;
#45260 = DIRECTION ( 'NONE',  ( -0.5941640067486159138, 0.8043439146810467122, 0.000000000000000000 ) ) ;
#45261 = DIRECTION ( 'NONE',  ( -1.000000000000000000, 0.000000000000000000, 0.000000000000000000 ) ) ;
#45262 = CARTESIAN_POINT ( 'NONE',  ( 38.54538599346576433, -292.1390015054272453, -278.8372595960646549 ) ) ;
#45263 = CARTESIAN_POINT ( 'NONE',  ( 25.62276755908332859, -288.6276234087768557, -231.8654529919994332 ) ) ;
#45264 = CARTESIAN_POINT ( 'NONE',  ( -99.19301482913152768, -289.3844882588369387, -226.2205597104584740 ) ) ;
#45265 = CARTESIAN_POINT ( 'NONE',  ( 17.31619302659392901, -288.2773176330660476, -221.0686912890308804 ) ) ;
#45266 = ADVANCED_FACE ( 'NONE', ( #29861 ), #28468, .F. ) ;
#45267 = DIRECTION ( 'NONE',  ( 0.000000000000000000, 0.000000000000000000, 1.000000000000000000 ) ) ;
#45268 = CARTESIAN_POINT ( 'NONE',  ( 10.22799617783092074, -289.1793204394008399, -326.0134130377272186 ) ) ;
#45269 = CARTESIAN_POINT ( 'NONE',  ( -33.49307446567431867, -296.9838493624466764, -345.6308163123198938 ) ) ;
#45270 = CARTESIAN_POINT ( 'NONE',  ( 200.2349812190172713, 66.43136063442170780, -7.741079165001072404 ) ) ;
#45271 = CARTESIAN_POINT ( 'NONE',  ( -31.83989572058621675, -290.1893869203370286, -346.8184997918723980 ) ) ;
#45272 = CARTESIAN_POINT ( 'NONE',  ( -9.446048453272680945, -278.4350352833361626, -200.3594078527704028 ) ) ;
#45273 = CARTESIAN_POINT ( 'NONE',  ( -51.30461677501067186, -277.5592812958528270, -346.0630416711411499 ) ) ;
#45274 = CARTESIAN_POINT ( 'NONE',  ( -6.235019267237946750, -280.1164900257368799, -199.9329394121948837 ) ) ;
#45275 = CARTESIAN_POINT ( 'NONE',  ( -99.83819656525525943, -299.0863136954325796, -229.4504473590564828 ) ) ;
#45276 = CARTESIAN_POINT ( 'NONE',  ( -72.08263087683934600, -283.5925013757965871, -203.8925661531843900 ) ) ;
#45277 = CARTESIAN_POINT ( 'NONE',  ( -110.5272221829468009, -271.6842131151094577, -270.3500670393695486 ) ) ;
#45278 = CARTESIAN_POINT ( 'NONE',  ( -21.91497456255137521, -278.3913552543355650, -197.6937699094292782 ) ) ;
#45279 = CARTESIAN_POINT ( 'NONE',  ( -91.02056166489622058, -281.8143853665579854, -322.7403168332483574 ) ) ;
#45280 = CARTESIAN_POINT ( 'NONE',  ( 194.7510731661265595, -164.3527196417747689, -21.50000000000000000 ) ) ;
#45281 = CARTESIAN_POINT ( 'NONE',  ( -20.29995273181706850, -275.3170959679144971, -344.7946832512226933 ) ) ;
#45282 = CARTESIAN_POINT ( 'NONE',  ( -90.89792542045735502, -297.3492718299288526, -321.0551192429788898 ) ) ;
#45283 = CARTESIAN_POINT ( 'NONE',  ( -65.15296244275525339, -282.3274957100301776, -341.8457227189608716 ) ) ;
#45284 = CARTESIAN_POINT ( 'NONE',  ( -106.2043489005842076, -297.1606414831994698, -295.4369382468241838 ) ) ;
#45285 = CARTESIAN_POINT ( 'NONE',  ( -15.00614236063741203, -299.6414511227042112, -193.8493901701033337 ) ) ;
#45286 = CARTESIAN_POINT ( 'NONE',  ( -62.03285450581438454, -273.3887881194525562, -201.6411472153219222 ) ) ;
#45287 = CARTESIAN_POINT ( 'NONE',  ( 33.43570360707399658, -295.8754012357659349, -295.3272527403886443 ) ) ;
#45288 = CARTESIAN_POINT ( 'NONE',  ( 20.57430203005223390, -288.4054981593803859, -321.1228455589242685 ) ) ;
#45289 = CARTESIAN_POINT ( 'NONE',  ( -42.31047902625270041, -278.0697983300320857, -194.9646629263701527 ) ) ;
#45290 = CARTESIAN_POINT ( 'NONE',  ( -109.8662678751797159, -290.0571767206755567, -296.3878539220891639 ) ) ;
#45291 = CARTESIAN_POINT ( 'NONE',  ( -90.77260697509257170, -288.8918211602427846, -320.5205821211498005 ) ) ;
#45292 = CARTESIAN_POINT ( 'NONE',  ( 32.57754153347347881, -291.9049435989788890, -297.4959718076015633 ) ) ;
#45293 = ORIENTED_EDGE ( 'NONE', *, *, #35319, .F. ) ;
#45294 = CARTESIAN_POINT ( 'NONE',  ( 197.3688982409817072, 70.32660332368789113, 11.79193394828015151 ) ) ;
#45295 = CARTESIAN_POINT ( 'NONE',  ( -108.4117365732641645, -289.8364762266366483, -287.3033244962084041 ) ) ;
#45296 = CARTESIAN_POINT ( 'NONE',  ( -83.63170945779077670, -296.0521521680024080, -417.1172536214571096 ) ) ;
#45297 = CARTESIAN_POINT ( 'NONE',  ( -30.91553340198313293, -287.0727096231913151, -193.8526052109661748 ) ) ;
#45298 = CARTESIAN_POINT ( 'NONE',  ( -102.0455923789670294, -287.4805209788416391, -239.2376011013261916 ) ) ;
#45299 = CARTESIAN_POINT ( 'NONE',  ( -65.52829258352753072, -294.4705592145330115, -341.7779320447328928 ) ) ;
#45300 = CARTESIAN_POINT ( 'NONE',  ( 0.6381908120249473182, -283.8720357133968264, -336.7903051716934328 ) ) ;
#45301 = CARTESIAN_POINT ( 'NONE',  ( -108.7205108743162327, -284.1828665431768286, -285.7196913973003234 ) ) ;
#45302 = CARTESIAN_POINT ( 'NONE',  ( 34.37817999008198910, -277.0783432684659715, -286.4652776280779563 ) ) ;
#45303 = CARTESIAN_POINT ( 'NONE',  ( 26.26231454023571388, -291.0444558292219881, -231.1940771457058474 ) ) ;
#45304 = CARTESIAN_POINT ( 'NONE',  ( 21.81024513933711972, -273.7415758298365631, -226.9079492056313256 ) ) ;
#45305 = ORIENTED_EDGE ( 'NONE', *, *, #65063, .T. ) ;
#45306 = CARTESIAN_POINT ( 'NONE',  ( 196.6738303916082202, 40.98441723029247186, 12.63306117497344516 ) ) ;
#45307 = CARTESIAN_POINT ( 'NONE',  ( 0.8876039443801369000, -288.4861503455589400, -206.4274523369742838 ) ) ;
#45308 = CARTESIAN_POINT ( 'NONE',  ( -103.5897455579518009, -298.1377378446680950, -231.6210984090975273 ) ) ;
#45309 = CARTESIAN_POINT ( 'NONE',  ( -70.03545256445691791, -286.2611240578390834, -204.9635837788331116 ) ) ;
#45310 = CARTESIAN_POINT ( 'NONE',  ( -109.3812106364152044, -277.9488011015175175, -243.6911362088033286 ) ) ;
#45311 = CARTESIAN_POINT ( 'NONE',  ( 6.431390130924254045, -293.2813503129785886, -207.1374724414909565 ) ) ;
#45312 = CARTESIAN_POINT ( 'NONE',  ( -2.765125299495188038, -284.6438363744840103, -202.9317207452971559 ) ) ;
#45313 = AXIS2_PLACEMENT_3D ( 'NONE', #6204, #7140, #36013 ) ;
#45314 = CARTESIAN_POINT ( 'NONE',  ( -19.28811968887323047, -295.1594244674266747, -345.2478843144521647 ) ) ;
#45315 = CARTESIAN_POINT ( 'NONE',  ( -44.30644667947097304, -292.2950602546472965, -197.6220482425636931 ) ) ;
#45316 = CARTESIAN_POINT ( 'NONE',  ( -43.18343439339132317, -486.4924983417995463, -435.6442049081568939 ) ) ;
#45317 = DIRECTION ( 'NONE',  ( 0.000000000000000000, -0.000000000000000000, 1.000000000000000000 ) ) ;
#45318 = CARTESIAN_POINT ( 'NONE',  ( 201.7602898703401593, 289.7935802246203707, -82.39453363547674769 ) ) ;
#45319 = TOROIDAL_SURFACE ( 'NONE', #33309, 3.342139515347635204, 0.5000000000000000000 ) ;
#45320 = CARTESIAN_POINT ( 'NONE',  ( -106.0631733072216889, -286.5016716867549462, -237.1938619162372959 ) ) ;
#45321 = CARTESIAN_POINT ( 'NONE',  ( 36.57525178469694538, -279.4809262143061233, -305.9938812882205070 ) ) ;
#45322 = EDGE_LOOP ( 'NONE', ( #85559, #61687, #4318, #91194 ) ) ;
#45323 = EDGE_CURVE ( 'NONE', #33370, #62133, #87134, .T. ) ;
#45324 = CARTESIAN_POINT ( 'NONE',  ( -26.71148304544562180, -281.8342226617896813, -342.9469328395128400 ) ) ;
#45325 = CARTESIAN_POINT ( 'NONE',  ( -114.0224314397881642, -278.3108114621884397, -263.0117211945404847 ) ) ;
#45326 = CARTESIAN_POINT ( 'NONE',  ( 37.39821335018235260, -283.6004216167411300, -274.0992668617450363 ) ) ;
#45327 = CARTESIAN_POINT ( 'NONE',  ( 204.8861976254081014, 293.2992890834860304, -54.00000000000341061 ) ) ;
#45328 = EDGE_CURVE ( 'NONE', #20911, #15284, #35088, .T. ) ;
#45329 = CARTESIAN_POINT ( 'NONE',  ( -38.74010266070690278, -281.6441037679083479, -346.7590941683267829 ) ) ;
#45330 = CARTESIAN_POINT ( 'NONE',  ( -30.35272573237195814, -284.1609529146971340, -195.9922780480186475 ) ) ;
#45331 = CARTESIAN_POINT ( 'NONE',  ( 20.88612265193818018, -276.7498957291303441, -221.8861126911111228 ) ) ;
#45332 = CARTESIAN_POINT ( 'NONE',  ( -40.52692408626661802, -298.5034039385015490, -197.3564852134321654 ) ) ;
#45333 = CARTESIAN_POINT ( 'NONE',  ( -53.27248478009627775, -293.9454227737210772, -342.1592126568729100 ) ) ;
#45334 = CARTESIAN_POINT ( 'NONE',  ( -112.9638711985142265, -279.0279628279747612, -284.3833336986024278 ) ) ;
#45335 = CARTESIAN_POINT ( 'NONE',  ( 22.46583636945384654, -276.1369269143394831, -312.3055003260388958 ) ) ;
#45336 = CARTESIAN_POINT ( 'NONE',  ( -111.5228456925401588, -273.8787118613371376, -250.6988033055215226 ) ) ;
#45337 = CARTESIAN_POINT ( 'NONE',  ( -75.19563939159630195, -276.4647871765138234, -337.0587325738197819 ) ) ;
#45338 = CARTESIAN_POINT ( 'NONE',  ( 102.7371733171515018, 116.6117108516616980, -282.8160689237882366 ) ) ;
#45339 = CARTESIAN_POINT ( 'NONE',  ( -62.26366848851381519, -275.3759840907413832, -341.1531895201201792 ) ) ;
#45340 = CARTESIAN_POINT ( 'NONE',  ( -34.85549540849656580, -296.4467579933129286, -346.7314334226518326 ) ) ;
#45341 = CARTESIAN_POINT ( 'NONE',  ( -95.95921662488163406, -280.4090924074130839, -317.1477375740089997 ) ) ;
#45342 = CARTESIAN_POINT ( 'NONE',  ( 122.2132510144744231, 146.9671518294229884, -260.0597590233358574 ) ) ;
#45343 = CARTESIAN_POINT ( 'NONE',  ( -108.7231442090566560, -285.4117889738186591, -287.1166838504625503 ) ) ;
#45344 = CARTESIAN_POINT ( 'NONE',  ( -44.30374784430958357, -284.8990630343463977, -346.0808320929590423 ) ) ;
#45345 = CARTESIAN_POINT ( 'NONE',  ( -95.92031844025744647, -276.3273690398260669, -315.2497122343116303 ) ) ;
#45346 = CARTESIAN_POINT ( 'NONE',  ( -110.8384229624914070, -286.5480659844130287, -259.9161568516495890 ) ) ;
#45347 = CARTESIAN_POINT ( 'NONE',  ( -27.44628998427068112, -278.6598804190817873, -197.2834946226149668 ) ) ;
#45348 = CARTESIAN_POINT ( 'NONE',  ( -9.859778334522250276, -277.7642882091117258, -338.3377473352047673 ) ) ;
#45349 = CARTESIAN_POINT ( 'NONE',  ( 207.5217838046588099, 35.61973263570791204, 14.46447120960655752 ) ) ;
#45350 = CARTESIAN_POINT ( 'NONE',  ( -62.05640394789998737, -274.2142833789010297, -201.6066864400953875 ) ) ;
#45351 = CARTESIAN_POINT ( 'NONE',  ( 17.10146738478125172, -281.6070190068512034, -216.0638285496460185 ) ) ;
#45352 = CARTESIAN_POINT ( 'NONE',  ( 10.77963033762923928, -281.1892422867358050, -210.2606409147305158 ) ) ;
#45353 = ORIENTED_EDGE ( 'NONE', *, *, #91573, .T. ) ;
#45354 = ORIENTED_EDGE ( 'NONE', *, *, #49001, .F. ) ;
#45355 = CARTESIAN_POINT ( 'NONE',  ( 200.7304780712264289, 15.47998366482157984, -9.999999999999360512 ) ) ;
#45356 = CARTESIAN_POINT ( 'NONE',  ( 11.26667213596453010, -288.5773619600907978, -212.1761412293852516 ) ) ;
#45357 = CARTESIAN_POINT ( 'NONE',  ( -88.23073484802083044, -296.5147172052627980, -217.7270274236295791 ) ) ;
#45358 = CARTESIAN_POINT ( 'NONE',  ( -77.10943649907028430, -290.8828963689570628, -204.4829958289571721 ) ) ;
#45359 = CARTESIAN_POINT ( 'NONE',  ( -3.060934746067260015, -287.0708642305584135, -335.6521006424450206 ) ) ;
#45360 = CARTESIAN_POINT ( 'NONE',  ( 31.02592621283743313, -286.4898793797690359, -297.7242367025642693 ) ) ;
#45361 = CARTESIAN_POINT ( 'NONE',  ( -52.18414238861056731, -287.0629528568209707, -198.4804362149092753 ) ) ;
#45362 = CARTESIAN_POINT ( 'NONE',  ( -100.4288371088549496, -276.0045833872349021, -311.0147015159300281 ) ) ;
#45363 = CARTESIAN_POINT ( 'NONE',  ( -41.73501447955607802, -287.5064768702104629, -346.4474516866881117 ) ) ;
#45364 = CARTESIAN_POINT ( 'NONE',  ( 0.4902437843262560935, -288.5564003803668811, -205.5870525946830014 ) ) ;
#45365 = CARTESIAN_POINT ( 'NONE',  ( -86.21227576637539869, -287.7276120389186076, -327.5407576198914512 ) ) ;
#45366 = CARTESIAN_POINT ( 'NONE',  ( -1.125255847982187030, -283.5000870675737588, -334.0146929964590186 ) ) ;
#45367 = CARTESIAN_POINT ( 'NONE',  ( -72.59692621455712924, -293.5867174684779002, -203.9605973817307358 ) ) ;
#45368 = DIRECTION ( 'NONE',  ( 0.000000000000000000, 0.000000000000000000, -1.000000000000000000 ) ) ;
#45369 = CARTESIAN_POINT ( 'NONE',  ( 196.0143093133015384, 20.19615242270663913, -11.99999999999998579 ) ) ;
#45370 = CARTESIAN_POINT ( 'NONE',  ( -109.8269366098551387, -298.1990455389077397, -291.7422298079723078 ) ) ;
#45371 = CARTESIAN_POINT ( 'NONE',  ( 7.248817477734777803, -279.8745120617452358, -212.2945343135737915 ) ) ;
#45372 = CARTESIAN_POINT ( 'NONE',  ( 8.381231125308847396, -278.6773768312384618, -210.8444522835007717 ) ) ;
#45373 = CARTESIAN_POINT ( 'NONE',  ( -24.94396379846014256, -294.0951829077525872, -346.2468234505490727 ) ) ;
#45374 = CARTESIAN_POINT ( 'NONE',  ( -67.12369655905537513, -296.0549657981457017, -202.8234196150576452 ) ) ;
#45375 = CARTESIAN_POINT ( 'NONE',  ( -18.67908428978831736, -274.8897727197424388, -342.4237363438489297 ) ) ;
#45376 = CARTESIAN_POINT ( 'NONE',  ( -6.543092194914787996, -295.9541643134278956, -337.0895918812256582 ) ) ;
#45377 = DIRECTION ( 'NONE',  ( 0.000000000000000000, 1.000000000000000000, 0.000000000000000000 ) ) ;
#45378 = CARTESIAN_POINT ( 'NONE',  ( -37.58583968854548374, -296.5290322190484176, -194.0548393963825049 ) ) ;
#45379 = CARTESIAN_POINT ( 'NONE',  ( -108.8890936950013497, -295.1193790189228707, -244.7692347713699519 ) ) ;
#45380 = CARTESIAN_POINT ( 'NONE',  ( -7.044103201143063764, -293.8829664374374033, -203.2982330228936974 ) ) ;
#45381 = CARTESIAN_POINT ( 'NONE',  ( 201.2104617360081704, 25.32700003806617772, 10.49999999999999822 ) ) ;
#45382 = CARTESIAN_POINT ( 'NONE',  ( 23.46979387138168960, -293.7913299739117861, -229.6847867250788227 ) ) ;
#45383 = AXIS2_PLACEMENT_3D ( 'NONE', #41579, #50092, #77585 ) ;
#45384 = DIRECTION ( 'NONE',  ( 0.000000000000000000, 0.000000000000000000, -1.000000000000000000 ) ) ;
#45386 = CARTESIAN_POINT ( 'NONE',  ( -9.230880848015225126, -294.6741361445097027, -337.7452057936255869 ) ) ;
#45385 = CARTESIAN_POINT ( 'NONE',  ( -88.74541761781200933, -283.3554055588260212, -215.1896759589265571 ) ) ;
#45387 = CARTESIAN_POINT ( 'NONE',  ( 37.54836979103883721, -281.7766961099754894, -288.3192426046718424 ) ) ;
#45388 = CARTESIAN_POINT ( 'NONE',  ( 19.95782821964991172, -282.7945567765212900, -221.0862162384978546 ) ) ;
#45389 = AXIS2_PLACEMENT_3D ( 'NONE', #7573, #36458, #65373 ) ;
#45390 = CARTESIAN_POINT ( 'NONE',  ( -37.97801149621697192, -285.7111050242172041, -193.3848917857536378 ) ) ;
#45391 = CARTESIAN_POINT ( 'NONE',  ( -110.2068935356522985, -288.7721169223410129, -253.2556226922589246 ) ) ;
#45392 = CYLINDRICAL_SURFACE ( 'NONE', #333, 1.000000000000000888 ) ;
#45393 = CARTESIAN_POINT ( 'NONE',  ( -35.93159539721197149, -281.5146868155068205, -346.6677561198292778 ) ) ;
#45394 = CARTESIAN_POINT ( 'NONE',  ( -38.61677816059080470, -284.7206912621533661, -196.8664610464527414 ) ) ;
#45395 = ADVANCED_FACE ( 'NONE', ( #7155 ), #51094, .T. ) ;
#45396 = CARTESIAN_POINT ( 'NONE',  ( -93.37638247032192851, -288.7549199201504280, -322.7980247665507818 ) ) ;
#45397 = CARTESIAN_POINT ( 'NONE',  ( 206.8859853974219618, 30.07047180831808220, 15.00000000000000000 ) ) ;
#45398 = CARTESIAN_POINT ( 'NONE',  ( -61.25331234156099214, -296.9678810366415291, -340.2341483074748112 ) ) ;
#45399 = CARTESIAN_POINT ( 'NONE',  ( -108.1038782663013365, -279.6084029904442332, -299.1937459700258728 ) ) ;
#45401 = CARTESIAN_POINT ( 'NONE',  ( 34.35581212509651294, -281.0354769907095829, -256.4549142522089937 ) ) ;
#45400 = CARTESIAN_POINT ( 'NONE',  ( 20.09720686897920316, -292.2441604142200049, -319.1379441269964445 ) ) ;
#45402 = CARTESIAN_POINT ( 'NONE',  ( 8.907849977643639505, -294.6037942475798559, -331.9239242823300629 ) ) ;
#45403 = CARTESIAN_POINT ( 'NONE',  ( -72.91307199997635280, -283.6648833478634515, -203.6399051195407424 ) ) ;
#45404 = CARTESIAN_POINT ( 'NONE',  ( -31.57787329713963942, -278.9796750358146937, -345.1905724855724884 ) ) ;
#45405 = CARTESIAN_POINT ( 'NONE',  ( 14.47431131801815773, -293.3602318227935939, -322.1867267386405729 ) ) ;
#45406 = CARTESIAN_POINT ( 'NONE',  ( -45.87632707952064948, -295.9437612409752205, -195.8482949895318654 ) ) ;
#45407 = ORIENTED_EDGE ( 'NONE', *, *, #35371, .T. ) ;
#45408 = CARTESIAN_POINT ( 'NONE',  ( -74.94434090351494149, -282.8906705383787994, 30.50000000000000000 ) ) ;
#45409 = CARTESIAN_POINT ( 'NONE',  ( 18.27179841713029873, -282.8353548065690575, -220.5717056173164963 ) ) ;
#45410 = CARTESIAN_POINT ( 'NONE',  ( -108.8380507295385513, -296.2588415518927150, -255.2590379625973469 ) ) ;
#45411 = DIRECTION ( 'NONE',  ( 0.000000000000000000, 0.000000000000000000, 1.000000000000000000 ) ) ;
#45412 = CARTESIAN_POINT ( 'NONE',  ( -106.6662871844225293, -275.6237833571633473, -303.7098442033569086 ) ) ;
#45413 = CARTESIAN_POINT ( 'NONE',  ( -92.04691142711175189, -272.4920690627170075, -216.4028129959773139 ) ) ;
#45414 = CARTESIAN_POINT ( 'NONE',  ( 38.48426874166048606, -288.7391327601870898, -260.1767811132301631 ) ) ;
#45415 = ADVANCED_FACE ( 'NONE', ( #49760 ), #79593, .T. ) ;
#45416 = CARTESIAN_POINT ( 'NONE',  ( -110.1228250358153247, -290.3028032226767436, -276.6277950747634122 ) ) ;
#45417 = CARTESIAN_POINT ( 'NONE',  ( -7.738527266000467364, -281.9674289834452452, -202.8613197309283578 ) ) ;
#45418 = CARTESIAN_POINT ( 'NONE',  ( 9.982640443567225574, -276.3166800180622431, -213.6651805570843692 ) ) ;
#45419 = CARTESIAN_POINT ( 'NONE',  ( -77.02369962265692038, -278.3027550229815574, -208.5553415596722573 ) ) ;
#45420 = CARTESIAN_POINT ( 'NONE',  ( -43.34239183861888733, -279.1281170144687849, -345.1206815714283493 ) ) ;
#45421 = ORIENTED_EDGE ( 'NONE', *, *, #57376, .F. ) ;
#45422 = CARTESIAN_POINT ( 'NONE',  ( -97.81174707469406826, -273.0230473028275924, -222.6916998320212144 ) ) ;
#45423 = CARTESIAN_POINT ( 'NONE',  ( -33.45727403043565573, -294.0215543308391943, -196.0097927622392149 ) ) ;
#45424 = CARTESIAN_POINT ( 'NONE',  ( 113.5000000000000568, -218.8335761803644743, -447.4016117689005796 ) ) ;
#45425 = CARTESIAN_POINT ( 'NONE',  ( 196.0143093133015384, 73.40565171261609123, 11.99999999999998757 ) ) ;
#45426 = CARTESIAN_POINT ( 'NONE',  ( -7.652043227905751976, -290.5767405007836146, -200.6417173057225227 ) ) ;
#45427 = CARTESIAN_POINT ( 'NONE',  ( -35.81076516078687177, -297.7385550635263485, -197.3400633275124108 ) ) ;
#45428 = DIRECTION ( 'NONE',  ( -0.000000000000000000, -1.000000000000000000, -0.000000000000000000 ) ) ;
#45429 = CARTESIAN_POINT ( 'NONE',  ( -110.9689653101546583, -292.3261470910621824, -250.2681969408431257 ) ) ;
#45430 = CARTESIAN_POINT ( 'NONE',  ( -72.02372285203398405, -285.9805209788416391, -342.4524372437778652 ) ) ;
#45431 = EDGE_CURVE ( 'NONE', #30016, #15179, #87522, .T. ) ;
#45432 = CARTESIAN_POINT ( 'NONE',  ( -5.029538327203971093, -288.4785857742228927, -202.8491923921184252 ) ) ;
#45433 = CARTESIAN_POINT ( 'NONE',  ( 29.66092597828588140, -273.9942016153243571, -303.8046688338029639 ) ) ;
#45434 = CARTESIAN_POINT ( 'NONE',  ( 23.44281826100330690, -276.8838097012996968, -227.3674839435452952 ) ) ;
#45435 = CARTESIAN_POINT ( 'NONE',  ( -86.86923170313787068, -289.4370025524622747, -214.7189427761151137 ) ) ;
#45436 = CARTESIAN_POINT ( 'NONE',  ( -99.25353038713504361, -280.9998170667708450, -226.6892648562441082 ) ) ;
#45437 = ORIENTED_EDGE ( 'NONE', *, *, #47255, .F. ) ;
#45438 = CARTESIAN_POINT ( 'NONE',  ( -7.219043887351488387, -281.9948741418995155, -336.9820435281337723 ) ) ;
#45439 = CARTESIAN_POINT ( 'NONE',  ( -105.9054158762234152, -280.0768918527389246, -235.8842601998994724 ) ) ;
#45440 = CARTESIAN_POINT ( 'NONE',  ( -65.12256794548457606, -282.2021116134155818, -341.7631486531930136 ) ) ;
#45441 = CARTESIAN_POINT ( 'NONE',  ( -98.60836983153294000, -278.8753012676129401, -316.6343406940106320 ) ) ;
#45442 = DIRECTION ( 'NONE',  ( 0.000000000000000000, 0.000000000000000000, 1.000000000000000000 ) ) ;
#45443 = CARTESIAN_POINT ( 'NONE',  ( 38.93726004563531973, -277.0463237552338001, -268.3049113418917955 ) ) ;
#45444 = CARTESIAN_POINT ( 'NONE',  ( 34.45848030099739390, -284.0519495502702512, -270.3284710469131937 ) ) ;
#45445 = ORIENTED_EDGE ( 'NONE', *, *, #87845, .T. ) ;
#45446 = ORIENTED_EDGE ( 'NONE', *, *, #3450, .T. ) ;
#45447 = CARTESIAN_POINT ( 'NONE',  ( -109.8981155163390611, -298.3076993857250159, -289.4004353956036084 ) ) ;
#45448 = TOROIDAL_SURFACE ( 'NONE', #16676, 2.500000000000000000, 0.5000000000000000000 ) ;
#45449 = CARTESIAN_POINT ( 'NONE',  ( -103.1167475618589577, -291.1950305726215333, -302.7319259384336760 ) ) ;
#45450 = CARTESIAN_POINT ( 'NONE',  ( -3.135702224652512360, -274.6180511108425435, -336.7071541350728694 ) ) ;
#45451 = CARTESIAN_POINT ( 'NONE',  ( -75.13990664688658683, -291.3088004263742050, -336.2797769341530625 ) ) ;
#45452 = CARTESIAN_POINT ( 'NONE',  ( -7.220676772660138631, -291.8066168539365890, -203.7531858684164945 ) ) ;
#45453 = CARTESIAN_POINT ( 'NONE',  ( 30.30559247667618550, -287.5355847231087409, -307.1245452848033892 ) ) ;
#45454 = DIRECTION ( 'NONE',  ( 0.2456588035076220367, -0.9693563597868450898, 0.000000000000000000 ) ) ;
#45455 = CARTESIAN_POINT ( 'NONE',  ( -107.2840283442263427, -283.2633246017062447, -246.6531743785229480 ) ) ;
#45456 = CARTESIAN_POINT ( 'NONE',  ( -59.02771209627567117, -291.1960282464961551, -341.4118680977248914 ) ) ;
#45457 = CARTESIAN_POINT ( 'NONE',  ( -104.7552833872145754, -282.6352037471804124, -300.1288277159952145 ) ) ;
#45458 = CARTESIAN_POINT ( 'NONE',  ( 36.05928883990203104, -282.9155454294988772, -274.0405602370758515 ) ) ;
#45459 = CARTESIAN_POINT ( 'NONE',  ( 32.65525296594349669, -288.8971886022393392, -301.8769357547007530 ) ) ;
#45460 = CARTESIAN_POINT ( 'NONE',  ( -109.9644671599078265, -278.9332314735262912, -278.8031483391190477 ) ) ;
#45461 = CARTESIAN_POINT ( 'NONE',  ( -70.71080952674611808, -290.4167097496552401, -201.4081538796177711 ) ) ;
#45462 = CARTESIAN_POINT ( 'NONE',  ( -21.02823705958982003, -287.0591935928943599, -195.2743032764545319 ) ) ;
#45463 = CARTESIAN_POINT ( 'NONE',  ( 27.39641412987663571, -288.5914458608899622, -312.0346382350710996 ) ) ;
#45464 = CARTESIAN_POINT ( 'NONE',  ( -53.68760389515414744, -283.4343448557227134, -341.5596103751664145 ) ) ;
#45465 = ORIENTED_EDGE ( 'NONE', *, *, #87897, .F. ) ;
#45466 = LINE ( 'NONE', #53051, #74604 ) ;
#45467 = CARTESIAN_POINT ( 'NONE',  ( -37.81153215191077521, -293.9067358323311510, -194.5977710222705355 ) ) ;
#45468 = CARTESIAN_POINT ( 'NONE',  ( 32.95677424236795616, -292.6255138529586475, -300.6846207049000554 ) ) ;
#45469 = CARTESIAN_POINT ( 'NONE',  ( 9.806408841652247688, -275.4427696346846233, -326.4009633426164214 ) ) ;
#45470 = CARTESIAN_POINT ( 'NONE',  ( -93.58252795655131706, -296.6173179792022552, -217.8403250770251418 ) ) ;
#45471 = CARTESIAN_POINT ( 'NONE',  ( 36.22816785272396345, -291.9657259607729429, -265.2877138855499197 ) ) ;
#45472 = CARTESIAN_POINT ( 'NONE',  ( -60.81634480758365413, -295.9833257022187922, -200.1149254197238747 ) ) ;
#45473 = CARTESIAN_POINT ( 'NONE',  ( -95.43804753559827247, -292.3853043251716031, -225.5064089325556722 ) ) ;
#45474 = CARTESIAN_POINT ( 'NONE',  ( -0.5911293696887359728, -295.6315310635115452, -333.8510845245479004 ) ) ;
#45475 = FACE_OUTER_BOUND ( 'NONE', #60016, .T. ) ;
#45476 = CARTESIAN_POINT ( 'NONE',  ( -80.83221744197234671, -293.6402437757760708, -331.7321535198165066 ) ) ;
#45477 = CARTESIAN_POINT ( 'NONE',  ( -109.3684315644258902, -298.8220211762325107, -249.4074323243745823 ) ) ;
#45478 = CARTESIAN_POINT ( 'NONE',  ( 31.19055395851106027, -288.1482299247048218, -244.3967453701713168 ) ) ;
#45479 = CARTESIAN_POINT ( 'NONE',  ( -12.38658042349540800, -278.7091946457800304, -341.5189435734233712 ) ) ;
#45480 = CARTESIAN_POINT ( 'NONE',  ( -97.62597504121067971, -276.7120119533249181, -317.6243692314821487 ) ) ;
#45481 = CARTESIAN_POINT ( 'NONE',  ( -78.77963635257771102, -272.8579550380201226, -205.5829563239488493 ) ) ;
#45482 = CARTESIAN_POINT ( 'NONE',  ( 14.91855299223730036, -280.3887284966206721, -323.4448021484951141 ) ) ;
#45483 = CARTESIAN_POINT ( 'NONE',  ( -99.01440295012493209, -276.3517975608069719, -315.1372864597314560 ) ) ;
#45484 = CARTESIAN_POINT ( 'NONE',  ( -106.2625019978786867, -295.5766965628918683, -244.6964534859231719 ) ) ;
#45485 = CARTESIAN_POINT ( 'NONE',  ( 160.6539576904058606, 293.9636489450775230, 7.999911143031724237 ) ) ;
#45486 = CARTESIAN_POINT ( 'NONE',  ( -51.58943670903502721, -274.5166287149664299, -198.6092223286751164 ) ) ;
#45487 = CARTESIAN_POINT ( 'NONE',  ( 197.2824889331299687, 25.87897341259697370, 12.13121414925255337 ) ) ;
#45488 = CARTESIAN_POINT ( 'NONE',  ( -109.9637240354653045, -288.3148092801115467, -290.4720217006682219 ) ) ;
#45489 = CARTESIAN_POINT ( 'NONE',  ( -98.15960609521329161, -289.9214753919098939, -317.5859241099873884 ) ) ;
#45490 = CARTESIAN_POINT ( 'NONE',  ( -101.1758787357383795, -275.0841720462387912, -230.6720002450604738 ) ) ;
#45491 = CARTESIAN_POINT ( 'NONE',  ( -103.0899219365449113, -294.0761666370108287, -306.0990495510316123 ) ) ;
#45492 = CARTESIAN_POINT ( 'NONE',  ( 11.38229625971367298, -281.5938503460535003, -329.8448683623522584 ) ) ;
#45493 = CARTESIAN_POINT ( 'NONE',  ( 175.2296996224749250, 275.0000000000000568, -24.99999999999999289 ) ) ;
#45494 = CARTESIAN_POINT ( 'NONE',  ( 13.69608000795611247, -280.3372934617109422, -325.3870031258165341 ) ) ;
#45495 = CARTESIAN_POINT ( 'NONE',  ( -43.18343439339132317, -283.1093320178187582, -435.6442049081568939 ) ) ;
#45496 = CARTESIAN_POINT ( 'NONE',  ( -97.07562347925731672, -289.9407734637303520, -227.6255677367136059 ) ) ;
#45497 = CARTESIAN_POINT ( 'NONE',  ( -111.3287460388996095, -282.6130557288284422, -276.4259770799287708 ) ) ;
#45498 = CARTESIAN_POINT ( 'NONE',  ( 169.7306087885279453, 250.5000000000000568, -24.89999999999999147 ) ) ;
#45499 = FACE_OUTER_BOUND ( 'NONE', #44198, .T. ) ;
#45500 = CARTESIAN_POINT ( 'NONE',  ( -25.05707924998244351, -290.2085090192244934, -196.3211412705609575 ) ) ;
#45501 = CARTESIAN_POINT ( 'NONE',  ( 24.36356781804805038, -276.5192291745055968, -230.0725630325194402 ) ) ;
#45502 = CARTESIAN_POINT ( 'NONE',  ( -93.13177514333392537, -285.0368290790923993, -322.8729742429882776 ) ) ;
#45504 = CARTESIAN_POINT ( 'NONE',  ( -79.30928351290206990, -285.4682408560149156, -210.5686499560788150 ) ) ;
#45503 = CARTESIAN_POINT ( 'NONE',  ( 1.695377242281931540, -272.6497519348476999, -205.6662898434930469 ) ) ;
#45505 = CARTESIAN_POINT ( 'NONE',  ( 24.48924943086669970, -277.5265145920085388, -310.3588523930935139 ) ) ;
#45506 = CARTESIAN_POINT ( 'NONE',  ( 18.43814199061066361, -277.0266233068542761, -317.7025474139956032 ) ) ;
#45507 = CARTESIAN_POINT ( 'NONE',  ( -109.7959477539794619, -286.8036344190833802, -250.7908744896595294 ) ) ;
#45508 = EDGE_LOOP ( 'NONE', ( #28838, #91941, #91513, #52660 ) ) ;
#45509 = CARTESIAN_POINT ( 'NONE',  ( -110.7022369792162806, -271.4005444928837960, -270.3464552583088789 ) ) ;
#45510 = CARTESIAN_POINT ( 'NONE',  ( -61.59357835053622665, -295.1919222595469137, -343.4979522127525229 ) ) ;
#45512 = CARTESIAN_POINT ( 'NONE',  ( -52.44584541453723858, -287.8376446061049023, -197.2604230830446852 ) ) ;
#45511 = TOROIDAL_SURFACE ( 'NONE', #27378, 5.343514653206205445, 0.5000000000000000000 ) ;
#45513 = CARTESIAN_POINT ( 'NONE',  ( -57.23711263161519724, -331.8906705383788562, 52.50000000000000711 ) ) ;
#45514 = CARTESIAN_POINT ( 'NONE',  ( -55.56934967048407970, -289.3380690714490129, -190.3538533559490702 ) ) ;
#45515 = CARTESIAN_POINT ( 'NONE',  ( -67.22926379071574843, -278.5896601590897603, -199.7337433422399613 ) ) ;
#45516 = CARTESIAN_POINT ( 'NONE',  ( 3.727702009367767300, -290.9944322968904089, -206.1133273080681363 ) ) ;
#45517 = CARTESIAN_POINT ( 'NONE',  ( -109.3939081053258917, -285.8693955373045128, -285.8866541636337502 ) ) ;
#45518 = CARTESIAN_POINT ( 'NONE',  ( -88.24358142193966614, -281.0880971204780963, -216.5597149117222102 ) ) ;
#45519 = CARTESIAN_POINT ( 'NONE',  ( 11.68550559822367418, -288.1422883373899708, -211.6837322850167880 ) ) ;
#45520 = CARTESIAN_POINT ( 'NONE',  ( 35.26596656028086585, -283.7943648840376909, -289.2040261545441808 ) ) ;
#45521 = CARTESIAN_POINT ( 'NONE',  ( 21.73199087537919283, -276.3834763413260021, -319.7503783106523088 ) ) ;
#45522 = CARTESIAN_POINT ( 'NONE',  ( -94.86531623999313467, -295.2319974161572418, -222.7714986767394691 ) ) ;
#45523 = CARTESIAN_POINT ( 'NONE',  ( -110.5490224080664206, -278.6876476061310655, -246.3237672694672824 ) ) ;
#45524 = CARTESIAN_POINT ( 'NONE',  ( -91.10244640925002102, -299.2016006828159789, -218.7985242846185940 ) ) ;
#45525 = CARTESIAN_POINT ( 'NONE',  ( 159.3464669004306984, 15.95758591462588249, 10.08665682397413299 ) ) ;
#45526 = EDGE_CURVE ( 'NONE', #71459, #9221, #36487, .T. ) ;
#45527 = CARTESIAN_POINT ( 'NONE',  ( -114.2704648735229114, -281.0519495502701943, -270.3937649182068981 ) ) ;
#45528 = CARTESIAN_POINT ( 'NONE',  ( -77.52692868663658032, -295.6585503666685213, -206.1314294800253606 ) ) ;
#45529 = DIRECTION ( 'NONE',  ( 0.000000000000000000, 0.000000000000000000, 1.000000000000000000 ) ) ;
#45530 = CARTESIAN_POINT ( 'NONE',  ( -76.39400632000348423, -277.0971558784729609, -332.1693527646413600 ) ) ;
#45531 = CARTESIAN_POINT ( 'NONE',  ( -27.06506123191228497, -275.3849648292562051, -194.3974945961427068 ) ) ;
#45532 = CARTESIAN_POINT ( 'NONE',  ( 37.63312293349971327, -280.8184052323802007, -286.9019539993181525 ) ) ;
#45533 = CARTESIAN_POINT ( 'NONE',  ( -10.33372124884548882, -290.4550891440062514, -339.3257673219179651 ) ) ;
#45534 = CARTESIAN_POINT ( 'NONE',  ( -62.63365738748202460, -299.2489763132401777, -198.3678915657765742 ) ) ;
#45535 = CARTESIAN_POINT ( 'NONE',  ( -104.2485767827878647, -297.2698683459170752, -307.7720448142459873 ) ) ;
#45536 = CARTESIAN_POINT ( 'NONE',  ( -2.812418280082969790, -294.5098884634415981, -203.9701763978480642 ) ) ;
#45537 = CARTESIAN_POINT ( 'NONE',  ( 18.96799823851717548, -280.2380545079076910, -319.6485027626505939 ) ) ;
#45538 = CARTESIAN_POINT ( 'NONE',  ( 24.87285246547894957, -282.9154631487069196, -229.3944512481102436 ) ) ;
#45539 = CARTESIAN_POINT ( 'NONE',  ( 97.70547898648123919, -297.8351309912462739, -195.9657595870598072 ) ) ;
#45540 = CARTESIAN_POINT ( 'NONE',  ( -110.1675683560323620, -286.4388702932819228, -247.7594187457609962 ) ) ;
#45541 = CARTESIAN_POINT ( 'NONE',  ( -29.15218374684615910, -287.8662535896716577, -343.2113609113800408 ) ) ;
#45542 = CARTESIAN_POINT ( 'NONE',  ( -112.2161628243665348, -274.5480466014206513, -270.3865304996752457 ) ) ;
#45543 = VERTEX_POINT ( 'NONE', #72943 ) ;
#45544 = CARTESIAN_POINT ( 'NONE',  ( -23.43711449686069059, -287.4526104916761255, -345.5498203864059974 ) ) ;
#45545 = CARTESIAN_POINT ( 'NONE',  ( -10.73831514386218799, -286.0756019894115525, -202.3450335072697897 ) ) ;
#45546 = ORIENTED_EDGE ( 'NONE', *, *, #24741, .T. ) ;
#45547 = CARTESIAN_POINT ( 'NONE',  ( -95.09286514771430632, -284.9465771351677859, -320.8219488241056183 ) ) ;
#45548 = CARTESIAN_POINT ( 'NONE',  ( 34.64578401469587732, -275.7229976875547663, -258.0439336295440285 ) ) ;
#45549 = ADVANCED_FACE ( 'NONE', ( #42647 ), #71564, .F. ) ;
#45550 = CARTESIAN_POINT ( 'NONE',  ( -13.94761148858195376, -291.2689298221384320, -197.2696940767142451 ) ) ;
#45551 = CARTESIAN_POINT ( 'NONE',  ( 32.30359780815243198, -282.6229670549323032, -303.0879064200020139 ) ) ;
#45552 = CARTESIAN_POINT ( 'NONE',  ( 37.98654798598295201, -283.2270188642872881, -282.6232919335828910 ) ) ;
#45553 = CARTESIAN_POINT ( 'NONE',  ( -10.70536642750085754, -283.0474915632215129, -342.6413612009325789 ) ) ;
#45554 = CARTESIAN_POINT ( 'NONE',  ( -6.769419487506960209, -280.4649844485543326, -204.0576869032705929 ) ) ;
#45555 = CARTESIAN_POINT ( 'NONE',  ( -102.0172624299487154, -294.4809262143061801, -239.1787733560258289 ) ) ;
#45556 = CARTESIAN_POINT ( 'NONE',  ( -21.71499588232236633, -108.4839169218780910, -362.8552879306906220 ) ) ;
#45557 = ORIENTED_EDGE ( 'NONE', *, *, #76503, .T. ) ;
#45558 = CARTESIAN_POINT ( 'NONE',  ( 28.38897529805340980, -278.0298666294149257, -306.2397041744081889 ) ) ;
#45559 = CARTESIAN_POINT ( 'NONE',  ( -78.66963864116488026, -208.0198793462769515, -356.7005032217571738 ) ) ;
#45560 = CARTESIAN_POINT ( 'NONE',  ( -95.36492100020704754, -296.5256593477964202, -225.8750241165226385 ) ) ;
#45561 = CARTESIAN_POINT ( 'NONE',  ( 29.42535123994730739, -292.5626858866151565, -232.1290927326580515 ) ) ;
#45562 = CARTESIAN_POINT ( 'NONE',  ( 202.9738562182569694, 291.9636489450776367, -53.99999999998589573 ) ) ;
#45564 = CARTESIAN_POINT ( 'NONE',  ( -104.7870325975018773, -288.5515923591688647, -300.4468319604254702 ) ) ;
#45563 = CARTESIAN_POINT ( 'NONE',  ( -87.06496004988078141, -295.9505321715118953, -212.2723867604173051 ) ) ;
#45565 = CARTESIAN_POINT ( 'NONE',  ( -70.25069252932814834, -297.3509958966904492, -336.9033128876343426 ) ) ;
#45566 = CARTESIAN_POINT ( 'NONE',  ( 29.24977685218440371, -288.4502730639962351, -239.2674100956153325 ) ) ;
#45567 = EDGE_LOOP ( 'NONE', ( #76448, #51478 ) ) ;
#45568 = CARTESIAN_POINT ( 'NONE',  ( -0.9260767199387287540, -293.4648587388385295, -202.7835878029266325 ) ) ;
#45569 = CARTESIAN_POINT ( 'NONE',  ( -71.43204248231860731, -284.0076091134063745, -334.9818344748679806 ) ) ;
#45570 = CARTESIAN_POINT ( 'NONE',  ( -75.56837538139504318, -296.3492994282260042, -203.9170414095896149 ) ) ;
#45571 = CARTESIAN_POINT ( 'NONE',  ( -36.39065828649177803, -292.8666198832204373, -193.5154746173393221 ) ) ;
#45572 = CARTESIAN_POINT ( 'NONE',  ( 23.05585864486166869, -293.4062756309799056, -222.6781143594909338 ) ) ;
#45573 = CARTESIAN_POINT ( 'NONE',  ( -84.68341567097189682, -289.8923715197121851, -325.9954713532284245 ) ) ;
#45574 = ORIENTED_EDGE ( 'NONE', *, *, #9361, .T. ) ;
#45575 = DIRECTION ( 'NONE',  ( -1.000000000000000000, 2.441433246481030855E-15, 0.000000000000000000 ) ) ;
#45576 = CARTESIAN_POINT ( 'NONE',  ( -72.72520418568217337, -299.4494606519844524, -203.3083307234081758 ) ) ;
#45577 = CARTESIAN_POINT ( 'NONE',  ( -64.74363624956751551, -272.4971015828929808, -198.8128007990508479 ) ) ;
#45578 = CARTESIAN_POINT ( 'NONE',  ( 20.35897310022778228, -281.2445800340760798, -315.4614589779540097 ) ) ;
#45579 = EDGE_LOOP ( 'NONE', ( #92238, #72496, #17179, #13427 ) ) ;
#45580 = CARTESIAN_POINT ( 'NONE',  ( -67.69010906387433124, -276.9475107146832897, -341.0611956234716899 ) ) ;
#45581 = CARTESIAN_POINT ( 'NONE',  ( -99.94848574848113287, -271.4855134177338982, -231.2864355309620237 ) ) ;
#45582 = CARTESIAN_POINT ( 'NONE',  ( -110.2520349925624146, -280.2305774530794906, -284.3905712111647972 ) ) ;
#45583 = CARTESIAN_POINT ( 'NONE',  ( -48.82184626111737202, -275.3393451219001236, -343.7555340053512509 ) ) ;
#45584 = VECTOR ( 'NONE', #14073, 1000.000000000000000 ) ;
#45585 = CARTESIAN_POINT ( 'NONE',  ( -88.41299835021102638, -298.5223020756208143, -217.5753179060691025 ) ) ;
#45586 = CARTESIAN_POINT ( 'NONE',  ( -36.74615914089810786, -275.0010696616401447, -197.1157895607177579 ) ) ;
#45587 = CARTESIAN_POINT ( 'NONE',  ( -34.10992547473529868, -299.6920951693327311, -194.1602496597243714 ) ) ;
#45588 = CIRCLE ( 'NONE', #81890, 9.103929867429224387 ) ;
#45589 = CARTESIAN_POINT ( 'NONE',  ( 27.10913097588206355, -273.0503477253616325, -231.2165018471380620 ) ) ;
#45590 = CARTESIAN_POINT ( 'NONE',  ( 34.31476452488585238, -294.0130126873669383, -255.8958581531105096 ) ) ;
#45591 = CARTESIAN_POINT ( 'NONE',  ( 33.19907940913238775, -291.8496140260870675, -249.2241389348397718 ) ) ;
#45592 = DIRECTION ( 'NONE',  ( 1.124465274301078034E-16, 1.000000000000000000, 0.000000000000000000 ) ) ;
#45593 = ADVANCED_FACE ( 'NONE', ( #80043 ), #75354, .F. ) ;
#45594 = CARTESIAN_POINT ( 'NONE',  ( 19.83567369699905569, -276.7440212757485938, -321.8616561260699314 ) ) ;
#45595 = CARTESIAN_POINT ( 'NONE',  ( 23.79233879896182202, -275.1660055240000133, -230.4658890827383857 ) ) ;
#45596 = ORIENTED_EDGE ( 'NONE', *, *, #91565, .T. ) ;
#45597 = AXIS2_PLACEMENT_3D ( 'NONE', #62801, #32949, #89759 ) ;
#45598 = CARTESIAN_POINT ( 'NONE',  ( -95.90371218205980597, -282.5696191288851082, -319.6133856714011472 ) ) ;
#45599 = CARTESIAN_POINT ( 'NONE',  ( -32.11396708536629774, -296.9865349880702183, -345.3587169459429447 ) ) ;
#45600 = DIRECTION ( 'NONE',  ( 0.000000000000000000, 1.000000000000000000, 0.000000000000000000 ) ) ;
#45601 = CARTESIAN_POINT ( 'NONE',  ( -91.63419927090286876, -284.4508091940504073, -221.2466430781530278 ) ) ;
#45602 = CARTESIAN_POINT ( 'NONE',  ( -73.41899128812953279, -281.5290120294010876, -336.3620371340252859 ) ) ;
#45603 = CARTESIAN_POINT ( 'NONE',  ( 32.65307508127736469, -274.4258757261377468, -293.0790923753674520 ) ) ;
#45604 = CARTESIAN_POINT ( 'NONE',  ( 24.69688571741018634, -282.9815485281977772, -228.1932928273363927 ) ) ;
#45605 = CARTESIAN_POINT ( 'NONE',  ( 7.561795982442758302, -275.8857644787175332, -212.3024705588175607 ) ) ;
#45606 = LINE ( 'NONE', #66949, #86623 ) ;
#45607 = CARTESIAN_POINT ( 'NONE',  ( 196.2522475779649369, 20.68155234470936676, 13.54449592192992569 ) ) ;
#45608 = CARTESIAN_POINT ( 'NONE',  ( -60.60727323487409279, -272.1552965188378153, -197.7446938302877584 ) ) ;
#45609 = CARTESIAN_POINT ( 'NONE',  ( -53.39439349756933950, -281.8470233089592512, -196.8752943729790275 ) ) ;
#45610 = DIRECTION ( 'NONE',  ( 1.000000000000000000, 0.000000000000000000, 0.000000000000000000 ) ) ;
#45611 = CARTESIAN_POINT ( 'NONE',  ( -57.39770104258494854, -287.7155760488382725, -197.4571499221765976 ) ) ;
#45612 = LINE ( 'NONE', #59396, #92439 ) ;
#45613 = CARTESIAN_POINT ( 'NONE',  ( -78.96141488463774749, -289.4913040063623271, -207.9071417150786658 ) ) ;
#45614 = CARTESIAN_POINT ( 'NONE',  ( 61.37083282337847123, -250.8548725835408391, 22.50000000000000000 ) ) ;
#45615 = CARTESIAN_POINT ( 'NONE',  ( -96.73873518117028425, -294.7466845591411584, -313.5001213031345060 ) ) ;
#45616 = CARTESIAN_POINT ( 'NONE',  ( -59.07296906801516201, -287.4757954551026842, -341.3980409767154356 ) ) ;
#45617 = CARTESIAN_POINT ( 'NONE',  ( -104.5266604826868644, -260.4492150524036447, -315.3738353148558531 ) ) ;
#45618 = CARTESIAN_POINT ( 'NONE',  ( 28.11386210744392855, -285.5147603550024087, -231.0382941334338227 ) ) ;
#45619 = CARTESIAN_POINT ( 'NONE',  ( -45.71016593656803195, -284.7599787550973929, -343.7366713543623860 ) ) ;
#45620 = CARTESIAN_POINT ( 'NONE',  ( -68.78783806396161538, -281.6997171945549781, -339.5498661768355646 ) ) ;
#45621 = CARTESIAN_POINT ( 'NONE',  ( -49.68872445679357241, -291.8904214331853382, -198.3615401739482422 ) ) ;
#45622 = CARTESIAN_POINT ( 'NONE',  ( 3.012051695335717039, -282.0305610147144080, -208.7617864277644628 ) ) ;
#45623 = CARTESIAN_POINT ( 'NONE',  ( 34.39102420502452162, -282.5452018680484798, -284.8123269644436846 ) ) ;
#45624 = CARTESIAN_POINT ( 'NONE',  ( -73.61300428380712901, -291.5108948859240172, -336.4273373719661322 ) ) ;
#45625 = CARTESIAN_POINT ( 'NONE',  ( -62.84704857234799391, -297.8957525566902405, -197.7079886264569097 ) ) ;
#45626 = CARTESIAN_POINT ( 'NONE',  ( 19.47367773497335008, -286.3190012204545951, -320.1935226074151046 ) ) ;
#45627 = CARTESIAN_POINT ( 'NONE',  ( 23.63284201288958641, -274.9243643140495124, -223.3172659238111066 ) ) ;
#45628 = CARTESIAN_POINT ( 'NONE',  ( 23.12255955888526771, -294.9329017549430887, -226.5681673112793248 ) ) ;
#45629 = CARTESIAN_POINT ( 'NONE',  ( 200.1126601882106968, 250.5000000000000568, -2.416251949619912409 ) ) ;
#45630 = CARTESIAN_POINT ( 'NONE',  ( 10.59707575819634329, -289.1948066931273615, -210.1954327657594490 ) ) ;
#45631 = CARTESIAN_POINT ( 'NONE',  ( -87.99589381103636754, -275.7586119622723686, -325.8965218836639792 ) ) ;
#45632 = DIRECTION ( 'NONE',  ( -0.000000000000000000, -0.000000000000000000, 1.000000000000000000 ) ) ;
#45633 = CARTESIAN_POINT ( 'NONE',  ( -34.77229958908775131, -296.4836907700839106, -194.1617984748187951 ) ) ;
#45634 = CARTESIAN_POINT ( 'NONE',  ( -108.1687548953238718, -292.4241675039580173, -249.5805152551563424 ) ) ;
#45635 = CARTESIAN_POINT ( 'NONE',  ( -92.98598755200396226, -272.5743308168722479, -222.9328754195846045 ) ) ;
#45636 = CARTESIAN_POINT ( 'NONE',  ( -98.88916998517707668, -292.6301500274031469, -229.7391823582665609 ) ) ;
#45637 = CARTESIAN_POINT ( 'NONE',  ( -79.67645885818227214, -292.4057722322374957, -210.5396295467203629 ) ) ;
#45638 = CARTESIAN_POINT ( 'NONE',  ( -101.2652043455636317, -285.8072700437970184, -307.6674126302619925 ) ) ;
#45639 = CARTESIAN_POINT ( 'NONE',  ( -14.06336502786892417, -293.7734700788188320, -197.5269704734126890 ) ) ;
#45640 = CARTESIAN_POINT ( 'NONE',  ( -66.84087041418604258, -292.9887558954102929, -199.7700617090935111 ) ) ;
#45641 = CARTESIAN_POINT ( 'NONE',  ( -9.232842586139812013, -294.5074830280550486, -337.7460241464402202 ) ) ;
#45642 = CARTESIAN_POINT ( 'NONE',  ( 32.35290214813241505, -289.9147606742875496, -298.2080427116193277 ) ) ;
#45643 = CARTESIAN_POINT ( 'NONE',  ( 39.64055341967383583, -281.6774875402339831, -267.0552597894484279 ) ) ;
#45644 = CARTESIAN_POINT ( 'NONE',  ( -23.66001027692723113, -296.3020032288601442, -194.8055446936759267 ) ) ;
#45645 = CARTESIAN_POINT ( 'NONE',  ( -109.0277035254822096, -284.7434153487417348, -242.1071058771530033 ) ) ;
#45646 = CARTESIAN_POINT ( 'NONE',  ( 32.65208208140603574, -277.1937960940956032, -244.4243245598644023 ) ) ;
#45647 = EDGE_CURVE ( 'NONE', #33225, #79497, #93529, .T. ) ;
#45648 = CARTESIAN_POINT ( 'NONE',  ( -106.9037408604303749, -283.6583135665346731, -246.7872725094422890 ) ) ;
#45649 = CARTESIAN_POINT ( 'NONE',  ( 21.44067657335259369, -284.9118906800316608, -223.7613209704549035 ) ) ;
#45650 = CARTESIAN_POINT ( 'NONE',  ( -31.15067829409903410, -278.2690247337371261, -194.7978381986755210 ) ) ;
#45652 = CIRCLE ( 'NONE', #56307, 24.00000000000000355 ) ;
#45651 = FACE_OUTER_BOUND ( 'NONE', #70902, .T. ) ;
#45653 = CARTESIAN_POINT ( 'NONE',  ( -53.70954836035492974, -282.7754236523094846, -341.6177555141230187 ) ) ;
#45654 = AXIS2_PLACEMENT_3D ( 'NONE', #31327, #65476, #59758 ) ;
#45655 = CARTESIAN_POINT ( 'NONE',  ( -31.12138616649496825, -281.3340218728075683, -193.9587387820884032 ) ) ;
#45656 = CARTESIAN_POINT ( 'NONE',  ( 31.47116832282170051, -287.0508315903869061, -304.5046216165504802 ) ) ;
#45657 = CARTESIAN_POINT ( 'NONE',  ( -26.03073724693619440, -296.6663055088438341, -343.5050591555380493 ) ) ;
#45658 = CARTESIAN_POINT ( 'NONE',  ( -6.875639856457484100, -278.2590755929206239, -340.2197667536778454 ) ) ;
#45659 = CARTESIAN_POINT ( 'NONE',  ( 22.26738191377638287, -277.5143925991428091, -318.3407413579136573 ) ) ;
#45660 = CARTESIAN_POINT ( 'NONE',  ( -104.2722381377984249, -277.9921105565053381, -299.6305959823988587 ) ) ;
#45661 = CARTESIAN_POINT ( 'NONE',  ( -73.76084226763950369, -299.5675580647859988, -204.9877708626372907 ) ) ;
#45662 = CARTESIAN_POINT ( 'NONE',  ( 29.30215902541796424, -285.0995438386668184, -236.2082168952213692 ) ) ;
#45663 = AXIS2_PLACEMENT_3D ( 'NONE', #86279, #29937, #80575 ) ;
#45664 = CARTESIAN_POINT ( 'NONE',  ( -112.0793132728468180, -291.9636826002020484, -285.2841397491514499 ) ) ;
#45665 = CARTESIAN_POINT ( 'NONE',  ( -63.69289178503709081, -294.3241125446313617, -338.8242694400125856 ) ) ;
#45666 = VERTEX_POINT ( 'NONE', #22734 ) ;
#45667 = CARTESIAN_POINT ( 'NONE',  ( 12.36616173313047362, -294.0038836915295519, -323.9207518809613475 ) ) ;
#45668 = EDGE_LOOP ( 'NONE', ( #27629, #9379, #623, #71071, #79018 ) ) ;
#45669 = CARTESIAN_POINT ( 'NONE',  ( -48.80914246965920000, -290.2744646820648313, -346.2435348289337185 ) ) ;
#45670 = CARTESIAN_POINT ( 'NONE',  ( -87.60672713312604287, -279.9795476664357352, -217.2127247687157876 ) ) ;
#45671 = EDGE_CURVE ( 'NONE', #19571, #25512, #45885, .T. ) ;
#45672 = EDGE_CURVE ( 'NONE', #50719, #15573, #91972, .T. ) ;
#45673 = CARTESIAN_POINT ( 'NONE',  ( -109.5551561951845798, -295.7997391763244082, -244.5404039696304892 ) ) ;
#45674 = CARTESIAN_POINT ( 'NONE',  ( 27.04786786660995901, -287.6505331443672162, -228.3218943935549134 ) ) ;
#45675 = CARTESIAN_POINT ( 'NONE',  ( 7.925507525896447802, -288.7859810419243445, -332.6893961040652243 ) ) ;
#45676 = CARTESIAN_POINT ( 'NONE',  ( -69.01449666444777620, -283.8138239349079868, -336.1694640855753278 ) ) ;
#45677 = CARTESIAN_POINT ( 'NONE',  ( 44.71985729441861679, 12.68782823283341976, -331.8881429784326542 ) ) ;
#45678 = CARTESIAN_POINT ( 'NONE',  ( -57.44685790939539061, -168.5996598868645151, -362.8288648292558491 ) ) ;
#45679 = CARTESIAN_POINT ( 'NONE',  ( 5.477995611911152807, -59.15194608217792194, -350.9341101783960539 ) ) ;
#45680 = CARTESIAN_POINT ( 'NONE',  ( 5.483046864865452008, -275.6530729825468597, -329.7418210916221710 ) ) ;
#45681 = CARTESIAN_POINT ( 'NONE',  ( -48.66911171699923244, -276.1199639527063709, -342.8414206653997098 ) ) ;
#45682 = CARTESIAN_POINT ( 'NONE',  ( -3.437894570502412428, -297.9736291090912914, -193.4253938243076902 ) ) ;
#45683 = CARTESIAN_POINT ( 'NONE',  ( -110.3499271114021809, -272.7333562712346406, -270.3634251448670511 ) ) ;
#45684 = CARTESIAN_POINT ( 'NONE',  ( -108.2059980171341493, -276.8683979385705243, -299.1977189667084644 ) ) ;
#45685 = CARTESIAN_POINT ( 'NONE',  ( -92.45401980446736445, -290.3604962665202152, -318.4014999859691102 ) ) ;
#45686 = CARTESIAN_POINT ( 'NONE',  ( -34.06580258553204743, -298.8950159181937920, -193.5221595209639531 ) ) ;
#45687 = CARTESIAN_POINT ( 'NONE',  ( 34.76476796316281082, -286.4240113453520280, -284.6352770580871265 ) ) ;
#45688 = CARTESIAN_POINT ( 'NONE',  ( -99.48958076887087998, -273.8064184119138531, -224.9853538378266649 ) ) ;
#45689 = CARTESIAN_POINT ( 'NONE',  ( -107.4599590130346627, -296.9874427276698157, -250.0527508532690604 ) ) ;
#45690 = ORIENTED_EDGE ( 'NONE', *, *, #58679, .F. ) ;
#45691 = CARTESIAN_POINT ( 'NONE',  ( 188.7149167944524493, 8.542400036368780647, 10.00000000000000178 ) ) ;
#45692 = CARTESIAN_POINT ( 'NONE',  ( -23.18427210332027499, -278.7927552466910583, -344.6361315474793514 ) ) ;
#45693 = CARTESIAN_POINT ( 'NONE',  ( 6.884506129449763812, -281.9759780573676835, -333.3831494306261902 ) ) ;
#45694 = CARTESIAN_POINT ( 'NONE',  ( -108.5933385423970918, -279.8584088728788402, -253.1149561518478208 ) ) ;
#45695 = CARTESIAN_POINT ( 'NONE',  ( -69.84692176516939810, -279.2343948595678853, -339.0585829547333674 ) ) ;
#45696 = CARTESIAN_POINT ( 'NONE',  ( -98.93084734932266144, -295.6816983144295818, -229.9929908724099050 ) ) ;
#45697 = DIRECTION ( 'NONE',  ( 1.000000000000000000, 0.000000000000000000, 0.000000000000000000 ) ) ;
#45698 = CARTESIAN_POINT ( 'NONE',  ( -72.13157725982077295, -279.7450106879030045, -206.1842962033713889 ) ) ;
#45699 = CARTESIAN_POINT ( 'NONE',  ( 2.325868589020117394, -275.3722994125948276, -204.5534982684129659 ) ) ;
#45700 = CARTESIAN_POINT ( 'NONE',  ( 6.056408941011271807, -276.6406331761798469, -209.1287396833405126 ) ) ;
#45701 = CARTESIAN_POINT ( 'NONE',  ( 38.55013076045835874, -274.2445042629233285, -279.6940805236175152 ) ) ;
#45702 = VERTEX_POINT ( 'NONE', #52088 ) ;
#45703 = DIRECTION ( 'NONE',  ( 0.000000000000000000, 0.000000000000000000, 1.000000000000000000 ) ) ;
#45704 = CARTESIAN_POINT ( 'NONE',  ( -22.69833766112011730, -291.4415620824499342, -198.6800628696826436 ) ) ;
#45705 = CARTESIAN_POINT ( 'NONE',  ( -114.2532078311111121, -283.8697264757878429, -272.8376627250395927 ) ) ;
#45706 = CARTESIAN_POINT ( 'NONE',  ( 36.04048113988255864, -279.6615427907082108, -260.3340283629655687 ) ) ;
#45708 = CARTESIAN_POINT ( 'NONE',  ( -73.04357601725816096, -283.6550168022467346, -205.0267161194683752 ) ) ;
#45707 = CARTESIAN_POINT ( 'NONE',  ( 35.94089608900212340, -280.0320006008110454, -263.1111990805325149 ) ) ;
#45709 = CARTESIAN_POINT ( 'NONE',  ( -5.853555897882434245, -290.6383817648881518, -338.4448159084312806 ) ) ;
#45710 = CARTESIAN_POINT ( 'NONE',  ( -39.72944173616106411, -281.2266120858207614, -196.9903051133822771 ) ) ;
#45711 = FACE_OUTER_BOUND ( 'NONE', #25920, .T. ) ;
#45712 = AXIS2_PLACEMENT_3D ( 'NONE', #77426, #12565, #70349 ) ;
#45713 = CARTESIAN_POINT ( 'NONE',  ( -41.54559616467430061, -281.5040041371852340, -346.4968517232152294 ) ) ;
#45714 = CARTESIAN_POINT ( 'NONE',  ( 35.52318391697206579, -295.7811210881617967, -288.1831435745842782 ) ) ;
#45715 = CARTESIAN_POINT ( 'NONE',  ( -39.53524766614383879, -278.2648610296914740, -194.3932365179788064 ) ) ;
#45716 = AXIS2_PLACEMENT_3D ( 'NONE', #2232, #24454, #60002 ) ;
#45717 = CARTESIAN_POINT ( 'NONE',  ( -108.2689656642828879, -278.9697291758607207, -288.1105972686424366 ) ) ;
#45718 = CARTESIAN_POINT ( 'NONE',  ( -108.2562835291710712, -286.8743724088337217, -245.4382311826703926 ) ) ;
#45719 = CIRCLE ( 'NONE', #53303, 4.000000000000003553 ) ;
#45720 = FACE_OUTER_BOUND ( 'NONE', #65284, .T. ) ;
#45721 = CARTESIAN_POINT ( 'NONE',  ( -108.1334674485389229, -292.8144647908335969, -243.7952220366863685 ) ) ;
#45722 = VECTOR ( 'NONE', #35059, 1000.000000000000000 ) ;
#45723 = CARTESIAN_POINT ( 'NONE',  ( 37.59901702092596310, -273.6044406513971126, -274.4462853850380384 ) ) ;
#45724 = CARTESIAN_POINT ( 'NONE',  ( -26.17813813494850805, -288.1106463963140527, -346.3843624788316902 ) ) ;
#45725 = CARTESIAN_POINT ( 'NONE',  ( -22.56069930672988377, -290.6443945941650782, -198.0564678708298914 ) ) ;
#45726 = CARTESIAN_POINT ( 'NONE',  ( -43.28619158486827700, -274.0006242052569405, -431.8396057366803120 ) ) ;
#45727 = CARTESIAN_POINT ( 'NONE',  ( -109.9820225922646699, -277.0906945545703479, -281.5247657138087902 ) ) ;
#45728 = CARTESIAN_POINT ( 'NONE',  ( -93.66638592701164612, -295.3688994145142601, -221.9846166831470100 ) ) ;
#45729 = CARTESIAN_POINT ( 'NONE',  ( -82.83852812958338063, -291.0047492365516177, -328.0783781251117261 ) ) ;
#45730 = DIRECTION ( 'NONE',  ( 0.000000000000000000, 0.000000000000000000, 1.000000000000000000 ) ) ;
#45731 = CARTESIAN_POINT ( 'NONE',  ( 38.12793609700450759, -292.1742775381973161, -281.6323983360254033 ) ) ;
#45732 = CARTESIAN_POINT ( 'NONE',  ( -9.207062669472854566, -288.0263425686655410, -202.1207639795974842 ) ) ;
#45733 = CARTESIAN_POINT ( 'NONE',  ( 26.58006272377040347, -286.3393205788928526, -311.5431540319728470 ) ) ;
#45734 = EDGE_CURVE ( 'NONE', #29017, #41118, #80496, .T. ) ;
#45735 = CARTESIAN_POINT ( 'NONE',  ( 24.01539413042885585, -288.4171301277321504, -229.6403089738427070 ) ) ;
#45736 = DIRECTION ( 'NONE',  ( 0.000000000000000000, 0.000000000000000000, 1.000000000000000000 ) ) ;
#45737 = CARTESIAN_POINT ( 'NONE',  ( 23.64975031538770978, -288.9146848615072258, -310.7900036098784540 ) ) ;
#45738 = CARTESIAN_POINT ( 'NONE',  ( -19.64847687873387017, -296.8057705281709673, -343.6634301530109497 ) ) ;
#45739 = DIRECTION ( 'NONE',  ( 2.312964634635742267E-15, 0.000000000000000000, 1.000000000000000000 ) ) ;
#45740 = CARTESIAN_POINT ( 'NONE',  ( 26.79686661275973236, -288.2041063739244464, -228.4773147319844497 ) ) ;
#45741 = CARTESIAN_POINT ( 'NONE',  ( -105.0657823815663789, -276.1918128503554044, -303.9865664869094530 ) ) ;
#45742 = CARTESIAN_POINT ( 'NONE',  ( -114.3636775844629909, -278.8697807752670315, -271.6122899129514394 ) ) ;
#45743 = CARTESIAN_POINT ( 'NONE',  ( 23.73312251748550494, -280.5934339566821905, -223.4822426775248516 ) ) ;
#45744 = CARTESIAN_POINT ( 'NONE',  ( -102.6658987951841624, -299.0147943810757170, -234.2419282270451788 ) ) ;
#45745 = CARTESIAN_POINT ( 'NONE',  ( -89.05561611617861217, -283.3248562402314974, -216.0410338509788630 ) ) ;
#45746 = DIRECTION ( 'NONE',  ( 1.000000000000000000, -0.000000000000000000, -0.000000000000000000 ) ) ;
#45747 = CARTESIAN_POINT ( 'NONE',  ( -88.36265214200426499, -277.4681230353219803, -216.3667475058300340 ) ) ;
#45748 = CARTESIAN_POINT ( 'NONE',  ( -55.24996249445619867, -281.2823606113562391, -343.1917076044891246 ) ) ;
#45749 = CARTESIAN_POINT ( 'NONE',  ( 154.1407330040854333, 275.0000000000000568, 13.42592592592592915 ) ) ;
#45750 = CARTESIAN_POINT ( 'NONE',  ( 35.82311797338002179, -274.3069072277313580, -292.0778300268077032 ) ) ;
#45751 =( BOUNDED_CURVE ( )  B_SPLINE_CURVE ( 3, ( #91399, #26554, #24680, #39789 ),
 .UNSPECIFIED., .F., .T. ) 
 B_SPLINE_CURVE_WITH_KNOTS ( ( 4, 4 ),
 ( 3.871320309816760563, 4.712388980384689674 ),
 .UNSPECIFIED. ) 
 CURVE ( )  GEOMETRIC_REPRESENTATION_ITEM ( )  RATIONAL_B_SPLINE_CURVE ( ( 1.000000000000000000, 0.9419139527835179715, 0.9419139527835179715, 1.000000000000000000 ) ) 
 REPRESENTATION_ITEM ( '' )  );
#45752 = CARTESIAN_POINT ( 'NONE',  ( -109.2643544692940054, -297.8624451583949053, -286.4185009329046352 ) ) ;
#45753 = AXIS2_PLACEMENT_3D ( 'NONE', #19929, #84310, #19006 ) ;
#45754 = CARTESIAN_POINT ( 'NONE',  ( 13.46567483052855785, -281.2811382490925212, -327.8783178160979901 ) ) ;
#45755 = CARTESIAN_POINT ( 'NONE',  ( -107.0896943760818800, -297.1962788232704042, -292.8551309309443127 ) ) ;
#45756 = CARTESIAN_POINT ( 'NONE',  ( -49.64241171197495817, -275.3236409969477450, -194.8935412771584481 ) ) ;
#45757 = CARTESIAN_POINT ( 'NONE',  ( -54.21230415684278370, -273.4961626341039391, -199.3155677603087952 ) ) ;
#45758 = CARTESIAN_POINT ( 'NONE',  ( 36.68395610587595712, -295.3965629750618973, -258.2309605837090771 ) ) ;
#45759 = CARTESIAN_POINT ( 'NONE',  ( 22.08882082376648626, -287.0610279596776309, -221.4018166811355854 ) ) ;
#45760 =( BOUNDED_CURVE ( )  B_SPLINE_CURVE ( 3, ( #47204, #69476, #62385, #47686 ),
 .UNSPECIFIED., .F., .F. ) 
 B_SPLINE_CURVE_WITH_KNOTS ( ( 4, 4 ),
 ( 3.141592653589793116, 4.712388980384689674 ),
 .UNSPECIFIED. ) 
 CURVE ( )  GEOMETRIC_REPRESENTATION_ITEM ( )  RATIONAL_B_SPLINE_CURVE ( ( 1.000000000000000000, 0.8047378541243649375, 0.8047378541243649375, 1.000000000000000000 ) ) 
 REPRESENTATION_ITEM ( '' )  );
#45761 = CARTESIAN_POINT ( 'NONE',  ( -94.79466800568168594, -277.3067975407060999, -221.2650810117346794 ) ) ;
#45762 = CARTESIAN_POINT ( 'NONE',  ( -107.2595396599919439, -290.7995431253098104, -237.9773744700004272 ) ) ;
#45763 = CARTESIAN_POINT ( 'NONE',  ( -109.6533385077990346, -289.4573971865952444, -282.0347029890415911 ) ) ;
#45764 = CARTESIAN_POINT ( 'NONE',  ( 36.38635201542622610, -291.7294831584885628, -284.1844761798510604 ) ) ;
#45765 = ORIENTED_EDGE ( 'NONE', *, *, #80305, .T. ) ;
#45766 = CARTESIAN_POINT ( 'NONE',  ( 5.045406874201050940, -57.93311274753654061, -355.0152878038887820 ) ) ;
#45767 = CARTESIAN_POINT ( 'NONE',  ( -31.87300104025324288, -288.4890768506405720, -343.2683674209994820 ) ) ;
#45768 = CYLINDRICAL_SURFACE ( 'NONE', #61072, 4.025000000000000355 ) ;
#45769 = CARTESIAN_POINT ( 'NONE',  ( -92.25701923106899471, -284.7553235442392179, -323.9999839339699292 ) ) ;
#45770 = CARTESIAN_POINT ( 'NONE',  ( -3.414509733504233591, -291.5478656417370189, -201.4861414817669072 ) ) ;
#45771 = CARTESIAN_POINT ( 'NONE',  ( -19.02015581277936818, -284.1364114620302530, -344.6964056223281432 ) ) ;
#45772 = CARTESIAN_POINT ( 'NONE',  ( 7.792294985536637242, -282.2495523118050755, -327.8009524001496402 ) ) ;
#45773 = CARTESIAN_POINT ( 'NONE',  ( -108.8885982330457693, -296.9147991848542461, -241.7566077735413046 ) ) ;
#45774 = CARTESIAN_POINT ( 'NONE',  ( 16.90640573333437757, -277.5739549105646233, -319.9620116658109623 ) ) ;
#45775 = CARTESIAN_POINT ( 'NONE',  ( 16.06967236478934780, -290.8338130546777052, -218.1423366041460383 ) ) ;
#45776 = CARTESIAN_POINT ( 'NONE',  ( 26.99192173424906116, -273.8658235307314044, -234.9236410926782241 ) ) ;
#45777 = VERTEX_POINT ( 'NONE', #80972 ) ;
#45778 = CARTESIAN_POINT ( 'NONE',  ( 195.2223182338679806, 41.98397561837970215, 13.27870513978759526 ) ) ;
#45779 = CARTESIAN_POINT ( 'NONE',  ( -46.93419291606023336, -287.8496922318884117, -196.4899774052231294 ) ) ;
#45780 = AXIS2_PLACEMENT_3D ( 'NONE', #86611, #21780, #13283 ) ;
#45781 = CARTESIAN_POINT ( 'NONE',  ( -112.0016977470587562, -297.4109568845370859, -287.9500546963178067 ) ) ;
#45782 = CARTESIAN_POINT ( 'NONE',  ( -106.6315861683758754, -285.5145032322628822, -246.9043986513040920 ) ) ;
#45783 = CARTESIAN_POINT ( 'NONE',  ( -62.34072999955220240, -276.4281698334281714, -342.9973423688041976 ) ) ;
#45784 = CARTESIAN_POINT ( 'NONE',  ( 39.12383935974016680, -294.0954653115360315, -261.7291093873472505 ) ) ;
#45785 = CARTESIAN_POINT ( 'NONE',  ( 34.68234878705622748, -285.3891839350876580, -246.6805822762495097 ) ) ;
#45786 = CARTESIAN_POINT ( 'NONE',  ( 39.63469959446032931, -293.8488046098257200, -267.4331719496009896 ) ) ;
#45788 = CARTESIAN_POINT ( 'NONE',  ( -110.3890624587668583, -290.9104354157870489, -268.4654437844370136 ) ) ;
#45787 = VECTOR ( 'NONE', #45592, 1000.000000000000000 ) ;
#45789 = CARTESIAN_POINT ( 'NONE',  ( 175.2296996224749250, 249.5000000000000568, -24.99999999999999289 ) ) ;
#45790 = VECTOR ( 'NONE', #40336, 1000.000000000000000 ) ;
#45791 = CARTESIAN_POINT ( 'NONE',  ( 113.5000000000000568, -190.7866584945343504, -447.4016117689005796 ) ) ;
#45792 = CARTESIAN_POINT ( 'NONE',  ( 103.3612552652909073, 114.3676014650440607, -279.5696956816383931 ) ) ;
#45793 = CARTESIAN_POINT ( 'NONE',  ( -54.82472594265806265, -287.3514688123764813, -196.0842604881143529 ) ) ;
#45794 = CARTESIAN_POINT ( 'NONE',  ( -111.2586520408596868, -270.4809262143062369, -234.7283546768995564 ) ) ;
#45795 = ORIENTED_EDGE ( 'NONE', *, *, #34350, .T. ) ;
#45797 = CARTESIAN_POINT ( 'NONE',  ( -87.14889238244082037, -282.6857330485477746, -324.2215609949718669 ) ) ;
#45796 = VECTOR ( 'NONE', #30394, 1000.000000000000000 ) ;
#45798 = CARTESIAN_POINT ( 'NONE',  ( -96.13578908915418708, -277.5490490629295550, -320.0704915305914824 ) ) ;
#45799 = CARTESIAN_POINT ( 'NONE',  ( 12.50860946794144901, -282.7489176731266980, -214.5491563876983321 ) ) ;
#45800 = CARTESIAN_POINT ( 'NONE',  ( -87.72729469658391110, -231.2803686896094746, -346.7935326881681135 ) ) ;
#45801 = CARTESIAN_POINT ( 'NONE',  ( -1.923499357700632295, -281.1670612415235837, -338.0675235028114685 ) ) ;
#45803 = AXIS2_PLACEMENT_3D ( 'NONE', #4906, #25283, #31920 ) ;
#45802 = CARTESIAN_POINT ( 'NONE',  ( 19.03463836886439964, -284.8902242445822139, -221.4371436695146826 ) ) ;
#45804 = CARTESIAN_POINT ( 'NONE',  ( -64.48012981312817260, -275.5620986860499784, -199.6095362881306130 ) ) ;
#45805 = CARTESIAN_POINT ( 'NONE',  ( -38.33684707318784746, -295.5573083508033960, -343.4158791170682434 ) ) ;
#45806 = EDGE_CURVE ( 'NONE', #26669, #1911, #32179, .T. ) ;
#45807 = CARTESIAN_POINT ( 'NONE',  ( 25.27677249996951758, -291.7090668972056164, -231.7914899641262991 ) ) ;
#45808 = CARTESIAN_POINT ( 'NONE',  ( -108.5589040043047362, -278.8346685094983286, -299.3684042804711680 ) ) ;
#45809 = CARTESIAN_POINT ( 'NONE',  ( 7.580393323300029351, -276.4197835862396460, -327.9668672037786905 ) ) ;
#45810 = CARTESIAN_POINT ( 'NONE',  ( 23.26527609928194096, -275.1027384632600956, -317.3748252414483204 ) ) ;
#45811 = CARTESIAN_POINT ( 'NONE',  ( 159.4851178187871312, 3.000000000000000000, 9.000000000000001776 ) ) ;
#45812 = CARTESIAN_POINT ( 'NONE',  ( 14.80310999835316466, -274.3177913255401563, -324.3390232105376754 ) ) ;
#45813 = VECTOR ( 'NONE', #36780, 1000.000000000000000 ) ;
#45814 = ADVANCED_FACE ( 'NONE', ( #15643 ), #1432, .F. ) ;
#45815 = CARTESIAN_POINT ( 'NONE',  ( 22.71987118897137492, -295.6141513449050535, -317.6178438562093902 ) ) ;
#45816 = CARTESIAN_POINT ( 'NONE',  ( 152.4536156746142410, 129.7208004331680797, 12.50000000000000000 ) ) ;
#45817 = CARTESIAN_POINT ( 'NONE',  ( 193.8665746513534316, 275.1768195097669150, -123.9090917457166938 ) ) ;
#45818 = CIRCLE ( 'NONE', #64064, 3.342139515347647638 ) ;
#45819 = CARTESIAN_POINT ( 'NONE',  ( -102.0375808334600833, -285.1626734958675229, -304.9462029551175988 ) ) ;
#45820 = CARTESIAN_POINT ( 'NONE',  ( -78.59059452445588079, -285.3596057438592766, -334.1772814792511781 ) ) ;
#45821 = CARTESIAN_POINT ( 'NONE',  ( -8.206709036857517958, -285.7926714755894295, -203.3160214985641687 ) ) ;
#45822 = CARTESIAN_POINT ( 'NONE',  ( -62.07694774708168239, -275.7789239439487687, -339.9467985368535778 ) ) ;
#45823 = CARTESIAN_POINT ( 'NONE',  ( 34.85693152696198638, -283.6372873841950195, -287.6844053778939951 ) ) ;
#45824 = CARTESIAN_POINT ( 'NONE',  ( -59.42099449088976826, -275.8231556305547088, -340.6691012535990239 ) ) ;
#45825 = CARTESIAN_POINT ( 'NONE',  ( -4.917039185721430172, -277.6945688171628603, -336.1235848688297665 ) ) ;
#45826 = CARTESIAN_POINT ( 'NONE',  ( 184.8939426562960193, 2.965303559109565334, -9.000000000000001776 ) ) ;
#45827 = CARTESIAN_POINT ( 'NONE',  ( -6.304983870383714439, -281.2524201205200143, -200.0554756385484154 ) ) ;
#45828 = PRODUCT_DEFINITION ( 'UNKNOWN', '', #61340, #55170 ) ;
#45829 = VECTOR ( 'NONE', #52532, 1000.000000000000000 ) ;
#45830 = CARTESIAN_POINT ( 'NONE',  ( 38.19307660566169460, -281.8613876325513274, -255.7315449472019679 ) ) ;
#45831 = VERTEX_POINT ( 'NONE', #73867 ) ;
#45832 = ORIENTED_EDGE ( 'NONE', *, *, #30385, .F. ) ;
#45833 = CARTESIAN_POINT ( 'NONE',  ( 195.0811277904324186, 39.56745693038991618, 15.19607843137254477 ) ) ;
#45834 = CARTESIAN_POINT ( 'NONE',  ( -18.51228436096628727, -288.1524655174525833, -196.9191759970179305 ) ) ;
#45835 = CARTESIAN_POINT ( 'NONE',  ( -93.73149797201128308, -296.4088662294325900, -223.7284102769064873 ) ) ;
#45836 = CARTESIAN_POINT ( 'NONE',  ( -95.57828409341681208, -290.5799529695241858, -220.1233369751405746 ) ) ;
#45837 = CARTESIAN_POINT ( 'NONE',  ( 24.07674667750978514, -286.5921050256698663, -311.1086244163666947 ) ) ;
#45839 = CARTESIAN_POINT ( 'NONE',  ( -33.43280970683300524, -290.3418535259674513, -196.4384086568110206 ) ) ;
#45838 = CARTESIAN_POINT ( 'NONE',  ( -78.51903429613874152, -288.1928983510649118, -331.4126532901306064 ) ) ;
#45840 = CARTESIAN_POINT ( 'NONE',  ( 15.30367478487448096, -288.0217514732802897, -219.2182298651522103 ) ) ;
#45841 = CARTESIAN_POINT ( 'NONE',  ( -61.77904512899903011, -275.3694319698432196, -341.3230706764480260 ) ) ;
#45842 = CARTESIAN_POINT ( 'NONE',  ( 37.03954081327553638, -286.1619242342672464, -286.9696773643391339 ) ) ;
#45843 = CARTESIAN_POINT ( 'NONE',  ( 34.76121546066352153, -289.2844816214762318, -249.5330454387054715 ) ) ;
#45844 = CARTESIAN_POINT ( 'NONE',  ( -99.18702230774165685, -287.9740693104869251, -313.0832966707152423 ) ) ;
#45845 = CARTESIAN_POINT ( 'NONE',  ( -34.82649141581372731, -283.9610732389572263, -343.5656854178866411 ) ) ;
#45846 = CARTESIAN_POINT ( 'NONE',  ( -107.7653581308673409, -292.8944583262457400, -243.9345845901370353 ) ) ;
#45847 = DIRECTION ( 'NONE',  ( 0.000000000000000000, -0.000000000000000000, 1.000000000000000000 ) ) ;
#45848 = DIRECTION ( 'NONE',  ( -1.000000000000000000, 0.000000000000000000, 0.000000000000000000 ) ) ;
#45849 = CARTESIAN_POINT ( 'NONE',  ( -51.55418979226446652, -299.7920416901529279, -196.0964761880312892 ) ) ;
#45850 = CARTESIAN_POINT ( 'NONE',  ( 19.80854811423548512, -280.1054384290501957, -224.6834335686284874 ) ) ;
#45851 = CARTESIAN_POINT ( 'NONE',  ( 24.21203716334796496, -280.1333512500673351, -313.2112997231605505 ) ) ;
#45852 = CARTESIAN_POINT ( 'NONE',  ( -8.458242663589526700, -293.8808533643207852, -341.6207406232411472 ) ) ;
#45853 = CARTESIAN_POINT ( 'NONE',  ( -66.18769575042942677, -271.9091563394021591, -202.2004067812819414 ) ) ;
#45854 = CARTESIAN_POINT ( 'NONE',  ( 19.39030544968409231, -274.3040769767682150, -318.5564885447232655 ) ) ;
#45855 = CARTESIAN_POINT ( 'NONE',  ( -36.97638875489376886, -296.3626272252347462, -343.8658710738158675 ) ) ;
#45856 = CARTESIAN_POINT ( 'NONE',  ( 153.8610353528599717, 19.40315322326054215, 11.71374297039772649 ) ) ;
#45857 = CARTESIAN_POINT ( 'NONE',  ( -112.9584881692930622, -271.2698876741405911, -259.0141153792110913 ) ) ;
#45858 = CARTESIAN_POINT ( 'NONE',  ( -61.29369259105054368, -293.5987177744076462, -342.5290694644327232 ) ) ;
#45859 = VECTOR ( 'NONE', #10210, 1000.000000000000000 ) ;
#45860 = CARTESIAN_POINT ( 'NONE',  ( -41.64529874297971190, -293.4223034525724074, -196.8475866883864001 ) ) ;
#45861 = DIRECTION ( 'NONE',  ( -0.000000000000000000, -0.000000000000000000, -1.000000000000000000 ) ) ;
#45862 = CARTESIAN_POINT ( 'NONE',  ( 4.587837591657516256, -293.4368019563875123, -210.3447421683638368 ) ) ;
#45863 = CARTESIAN_POINT ( 'NONE',  ( 202.9738562182569694, 293.9636489450776367, -54.00000000000000000 ) ) ;
#45864 = AXIS2_PLACEMENT_3D ( 'NONE', #63611, #27126, #37364 ) ;
#45866 = CARTESIAN_POINT ( 'NONE',  ( -18.22050160756444015, -294.7987543605601672, -340.8123760773518711 ) ) ;
#45865 = CARTESIAN_POINT ( 'NONE',  ( -54.56368117419859942, -283.8520179393777880, -197.0002962274434708 ) ) ;
#45867 = AXIS2_PLACEMENT_3D ( 'NONE', #78130, #14668, #87068 ) ;
#45868 = CARTESIAN_POINT ( 'NONE',  ( -30.21489245098734244, -282.9643364679990327, -347.0305943883221289 ) ) ;
#45869 = CARTESIAN_POINT ( 'NONE',  ( 30.71365686633813041, -283.0417141345947130, -237.4112278355908074 ) ) ;
#45870 = CARTESIAN_POINT ( 'NONE',  ( -109.9559027117777390, -284.5413068590451644, -244.8087819912287841 ) ) ;
#45871 = CARTESIAN_POINT ( 'NONE',  ( -71.02363831306909958, -289.6064229106113999, -203.5363061957213517 ) ) ;
#45872 = CARTESIAN_POINT ( 'NONE',  ( 24.53363169025510260, -280.6298012115865959, -315.0392095006142199 ) ) ;
#45873 = CIRCLE ( 'NONE', #51956, 0.5000000000000004441 ) ;
#45874 = CARTESIAN_POINT ( 'NONE',  ( -39.97492824810908019, -284.7031986767851208, -196.9151542489718452 ) ) ;
#45875 = CARTESIAN_POINT ( 'NONE',  ( 23.88708881022347441, -287.0899104031517481, -316.5404197950383605 ) ) ;
#45876 = DIRECTION ( 'NONE',  ( 0.000000000000000000, 0.000000000000000000, -1.000000000000000000 ) ) ;
#45877 = CARTESIAN_POINT ( 'NONE',  ( 21.98155716331697107, -295.7610955023091606, -314.2609079715049347 ) ) ;
#45878 = CARTESIAN_POINT ( 'NONE',  ( -90.90296427159208292, -279.2192378610400283, -324.9310422228321045 ) ) ;
#45880 = CARTESIAN_POINT ( 'NONE',  ( -99.48349378287102240, -278.7486433588338741, -231.9177623336884437 ) ) ;
#45879 = CARTESIAN_POINT ( 'NONE',  ( 36.17359573761282832, -291.7845088181169331, -286.9694433173270909 ) ) ;
#45881 = CARTESIAN_POINT ( 'NONE',  ( 29.47458809792505008, -293.2216069896527415, -232.0912390672972094 ) ) ;
#45882 = CARTESIAN_POINT ( 'NONE',  ( -70.41347731427335077, -283.6994612225033165, -202.4231186276373364 ) ) ;
#45883 = CARTESIAN_POINT ( 'NONE',  ( -106.7945155903076540, -280.1831986214629069, -298.6684857622784648 ) ) ;
#45884 = CARTESIAN_POINT ( 'NONE',  ( -58.48759460446007097, -294.3911035599885508, -340.4771617555622925 ) ) ;
#45885 = B_SPLINE_CURVE_WITH_KNOTS ( 'NONE', 3,
 ( #59206, #30790, #61080, #17040, #23209, #16570, #89922, #73418, #25078, #67704, #2380, #45425 ),
 .UNSPECIFIED., .F., .F.,
 ( 4, 2, 2, 2, 2, 4 ),
 ( 0.000000000000000000, 0.002380535361927522270, 0.004761070723855044540, 0.007141606085782566810, 0.008331873766746348761, 0.009522141447710128978 ),
 .UNSPECIFIED. ) ;
#45886 = CARTESIAN_POINT ( 'NONE',  ( -64.78580409222807646, -295.6937435337983402, -200.5071804452682613 ) ) ;
#45887 = VERTEX_POINT ( 'NONE', #88531 ) ;
#45888 = CARTESIAN_POINT ( 'NONE',  ( -74.94434090351494149, -232.1443419142230766, 25.50000000000000000 ) ) ;
#45889 = AXIS2_PLACEMENT_3D ( 'NONE', #68016, #3145, #24933 ) ;
#45890 = CARTESIAN_POINT ( 'NONE',  ( 5.854930572371969788, -282.6209403198982386, -209.4850315757792316 ) ) ;
#45891 = CARTESIAN_POINT ( 'NONE',  ( -106.0471977359698172, -295.7272732527312655, -295.3603277282201702 ) ) ;
#45892 = CARTESIAN_POINT ( 'NONE',  ( 169.7306087885279453, 250.5000000000000568, -24.89999999999999147 ) ) ;
#45893 = CARTESIAN_POINT ( 'NONE',  ( 21.27581636871891391, -279.6952119285918457, -317.1477375740089997 ) ) ;
#45894 = CARTESIAN_POINT ( 'NONE',  ( -62.75581443872281540, -296.7879991201994585, -197.9253325829729988 ) ) ;
#45895 = CARTESIAN_POINT ( 'NONE',  ( 29.93705700826656013, -289.3428149920859482, -306.8981455190537986 ) ) ;
#45896 = CARTESIAN_POINT ( 'NONE',  ( -73.54680841647082445, -289.3802493337931310, -333.7647253963722846 ) ) ;
#45897 = CARTESIAN_POINT ( 'NONE',  ( -41.10577650072614375, -281.5240443333827329, -196.7639748144416671 ) ) ;
#45898 = CARTESIAN_POINT ( 'NONE',  ( -39.21615291765332501, -299.7884859192655540, -196.3589403066428645 ) ) ;
#45899 = AXIS2_PLACEMENT_3D ( 'NONE', #72359, #57688, #92240 ) ;
#45900 = CARTESIAN_POINT ( 'NONE',  ( -32.92386311034271529, -278.9039707970329687, -197.0971212214262778 ) ) ;
#45901 = VERTEX_POINT ( 'NONE', #23680 ) ;
#45902 = CARTESIAN_POINT ( 'NONE',  ( -111.0365049882156825, -272.6676781684890329, -247.8612628006189311 ) ) ;
#45903 = CARTESIAN_POINT ( 'NONE',  ( -99.51547383516302148, -293.0301176080004097, -229.3316865498255481 ) ) ;
#45904 = DIRECTION ( 'NONE',  ( 0.000000000000000000, 0.000000000000000000, 1.000000000000000000 ) ) ;
#45905 = CARTESIAN_POINT ( 'NONE',  ( -98.19092879092313808, -290.6416895204583852, -310.8964199128417363 ) ) ;
#45906 = LINE ( 'NONE', #88984, #39039 ) ;
#45907 = CARTESIAN_POINT ( 'NONE',  ( -39.15794629669244387, -290.1692097272985507, -194.6052606195188162 ) ) ;
#45908 = CARTESIAN_POINT ( 'NONE',  ( -37.81839704686878889, -297.7127365549954447, -197.3415298782453249 ) ) ;
#45909 = CARTESIAN_POINT ( 'NONE',  ( 9.339199855150265961, 0.000000000000000000, 74.50000000000001421 ) ) ;
#45910 = CARTESIAN_POINT ( 'NONE',  ( -109.7789112840558658, -292.3788669462162488, -246.2048394368796664 ) ) ;
#45911 = CARTESIAN_POINT ( 'NONE',  ( -2.659677404128715672, -288.9805209788416391, -198.2697987213421698 ) ) ;
#45912 = CARTESIAN_POINT ( 'NONE',  ( 36.36884218355848475, -289.3823685569780650, -257.1548739022682071 ) ) ;
#45913 = CARTESIAN_POINT ( 'NONE',  ( -36.46974125550492829, -275.0410765159518292, -345.2021562146079532 ) ) ;
#45914 = CARTESIAN_POINT ( 'NONE',  ( 25.20739260042890351, -278.0213165684791079, -310.8161546156699728 ) ) ;
#45915 = CARTESIAN_POINT ( 'NONE',  ( -49.90821954616613709, -289.9705764420085643, -196.9371472859167795 ) ) ;
#45916 = CARTESIAN_POINT ( 'NONE',  ( -42.37208488492256464, -281.8497579877422368, -194.7634942742383544 ) ) ;
#45917 = ORIENTED_EDGE ( 'NONE', *, *, #62258, .T. ) ;
#45918 = CARTESIAN_POINT ( 'NONE',  ( 33.42009158973589678, -281.1432199458240575, -288.7592941108543414 ) ) ;
#45919 = CARTESIAN_POINT ( 'NONE',  ( -98.54838335215242751, -279.0136982938760752, -316.5912634602032654 ) ) ;
#45920 = CARTESIAN_POINT ( 'NONE',  ( 8.956557551945696360, -281.2275180892643220, -331.3896363430529277 ) ) ;
#45921 = CARTESIAN_POINT ( 'NONE',  ( -28.61584149352048811, -277.8854431548829780, -346.6816896795406819 ) ) ;
#45922 = SHAPE_DEFINITION_REPRESENTATION ( #58649, #54338 ) ;
#45923 = CARTESIAN_POINT ( 'NONE',  ( -7.975466246460860553, -275.9499268648332873, -199.8754128566471593 ) ) ;
#45924 = CARTESIAN_POINT ( 'NONE',  ( 17.36665895637874613, -277.4090924074130839, -226.6919474004047572 ) ) ;
#45925 = ORIENTED_EDGE ( 'NONE', *, *, #45647, .T. ) ;
#45926 = CARTESIAN_POINT ( 'NONE',  ( -112.0903010805062507, -298.4657364787361189, -277.1041267494484828 ) ) ;
#45927 = CIRCLE ( 'NONE', #5139, 0.5000000000000000000 ) ;
#45928 = CARTESIAN_POINT ( 'NONE',  ( -5.646392611005856210, -289.7048503962845984, -336.4643218091442805 ) ) ;
#45929 = B_SPLINE_CURVE_WITH_KNOTS ( 'NONE', 3,
 ( #61267, #53677, #18152, #82545, #17695, #90102, #25253, #54129 ),
 .UNSPECIFIED., .F., .F.,
 ( 4, 2, 2, 4 ),
 ( 0.000000000000000000, 0.001370196721548361165, 0.002055295082322501198, 0.002740393443096640798 ),
 .UNSPECIFIED. ) ;
#45930 = CARTESIAN_POINT ( 'NONE',  ( 9.619521467656575453, -290.1766850936639912, -330.1659808181854032 ) ) ;
#45931 = CARTESIAN_POINT ( 'NONE',  ( -81.78444966438175356, -290.7773877344970970, -212.2562668699495987 ) ) ;
#45932 = CARTESIAN_POINT ( 'NONE',  ( 35.88725746498300140, -287.3568517540419975, -293.9629542044079358 ) ) ;
#45933 = CARTESIAN_POINT ( 'NONE',  ( 165.0704140682094589, 2.965303559109564890, -9.000000000000001776 ) ) ;
#45934 = CARTESIAN_POINT ( 'NONE',  ( -108.1164052708368928, -283.2278443668674299, -249.2703813498126522 ) ) ;
#45935 = CARTESIAN_POINT ( 'NONE',  ( 13.01072771616956558, -290.2007919822636950, -324.9791207377601268 ) ) ;
#45936 = CARTESIAN_POINT ( 'NONE',  ( -111.0017759286312611, -283.0609517610884041, -268.1473014485541739 ) ) ;
#45937 = CARTESIAN_POINT ( 'NONE',  ( 29.41365656777395543, -282.4539380225591572, -239.4989223355257479 ) ) ;
#45938 = CARTESIAN_POINT ( 'NONE',  ( 30.16151492831187397, -288.9689531535798892, -307.0255158180120247 ) ) ;
#45939 = AXIS2_PLACEMENT_3D ( 'NONE', #82880, #46888, #39779 ) ;
#45940 = CARTESIAN_POINT ( 'NONE',  ( -70.97557322295419624, -280.0881748828659852, -205.4875467505660538 ) ) ;
#45941 = CARTESIAN_POINT ( 'NONE',  ( -7.331543346083324586, -291.2319748177312704, -199.8670899874738609 ) ) ;
#45942 = CARTESIAN_POINT ( 'NONE',  ( -49.32964241029981167, -286.7060347371389071, -194.4098784383886027 ) ) ;
#45943 = CARTESIAN_POINT ( 'NONE',  ( -26.63587631261986033, -286.6770725324439013, -194.1176874726934329 ) ) ;
#45944 = CARTESIAN_POINT ( 'NONE',  ( -76.12532518708461282, -283.7525309730459639, -332.2661121931763546 ) ) ;
#45945 = ORIENTED_EDGE ( 'NONE', *, *, #25613, .T. ) ;
#45946 = DIRECTION ( 'NONE',  ( 1.000000000000000000, 0.000000000000000000, 0.000000000000000000 ) ) ;
#45947 = CARTESIAN_POINT ( 'NONE',  ( 3.456124272871578196, -294.4544190179785801, -206.4566139546910506 ) ) ;
#45948 = CIRCLE ( 'NONE', #89806, 204.9779373800640485 ) ;
#45949 = CARTESIAN_POINT ( 'NONE',  ( 33.98564415706008646, -292.5898197490000712, -298.0325514292105709 ) ) ;
#45950 = CIRCLE ( 'NONE', #14231, 0.5000000000000004441 ) ;
#45951 = CARTESIAN_POINT ( 'NONE',  ( -39.17563080251730412, -276.1344749856385192, -343.5734471836745456 ) ) ;
#45952 = CARTESIAN_POINT ( 'NONE',  ( -73.22566530574209764, -296.9380390815718442, -202.2901947835876513 ) ) ;
#45953 = CARTESIAN_POINT ( 'NONE',  ( 36.40168529197755731, -292.0375356836797778, -270.7830303976644473 ) ) ;
#45954 = CARTESIAN_POINT ( 'NONE',  ( -69.68033450518434790, -295.8602609546283020, -203.7864475493039151 ) ) ;
#45955 = CARTESIAN_POINT ( 'NONE',  ( -28.07132527227859597, -293.3773816730426347, -197.5008183971281710 ) ) ;
#45956 = CARTESIAN_POINT ( 'NONE',  ( 15.08700164969075352, -293.8928834022941601, -219.0492086584748677 ) ) ;
#45957 = CARTESIAN_POINT ( 'NONE',  ( 207.8643778022843662, 35.72636131987241725, 15.02863188060180732 ) ) ;
#45958 = VECTOR ( 'NONE', #8578, 1000.000000000000000 ) ;
#45959 = CARTESIAN_POINT ( 'NONE',  ( -30.77705423703443799, -292.9691785520989811, -345.2405801251408661 ) ) ;
#45960 = CARTESIAN_POINT ( 'NONE',  ( -62.92172665743409254, -299.7194103601173651, -199.8042390801840327 ) ) ;
#45961 = CARTESIAN_POINT ( 'NONE',  ( 29.64511473172418476, -288.8919723450572405, -300.0872385647375609 ) ) ;
#45962 = CARTESIAN_POINT ( 'NONE',  ( -72.05995984717635849, -279.4887710521282997, -337.2563642446237964 ) ) ;
#45963 = CARTESIAN_POINT ( 'NONE',  ( -59.56455444407535538, -276.1286575108956072, -343.6697359188431733 ) ) ;
#45964 = CIRCLE ( 'NONE', #20311, 0.5000000000000004441 ) ;
#45965 = CARTESIAN_POINT ( 'NONE',  ( -41.17937187458611703, -273.3537660303379084, -193.5066806700255029 ) ) ;
#45966 = CARTESIAN_POINT ( 'NONE',  ( 23.75290934614115912, -280.2133447556296346, -312.8906711424514242 ) ) ;
#45967 = CARTESIAN_POINT ( 'NONE',  ( -5.636412383093002632, -275.0419647468469293, -339.6519192977364696 ) ) ;
#45968 = CARTESIAN_POINT ( 'NONE',  ( -108.4509589499655249, -294.9929009239556876, -288.9774694734548461 ) ) ;
#45969 = CARTESIAN_POINT ( 'NONE',  ( -52.77971442013231496, -275.8546258925118195, -196.9147094505850077 ) ) ;
#45970 = CARTESIAN_POINT ( 'NONE',  ( -99.37135208161900835, -273.7366921289921606, -231.6801802147334683 ) ) ;
#45971 = DIRECTION ( 'NONE',  ( 1.000000000000000000, 0.000000000000000000, -0.000000000000000000 ) ) ;
#45973 = CARTESIAN_POINT ( 'NONE',  ( -51.55938161639841866, -273.6986671010971008, -198.7072509640707096 ) ) ;
#45972 = CARTESIAN_POINT ( 'NONE',  ( -110.7099506468699559, -288.7919530733773286, -253.1708118962006040 ) ) ;
#45974 = CARTESIAN_POINT ( 'NONE',  ( -48.74649010364381496, -299.8876356916179589, -195.8214324643442694 ) ) ;
#45975 = CARTESIAN_POINT ( 'NONE',  ( -71.79703280473380289, -293.5084023905571939, -336.8048050875983677 ) ) ;
#45976 = EDGE_CURVE ( 'NONE', #42078, #71834, #54199, .T. ) ;
#45977 = CARTESIAN_POINT ( 'NONE',  ( -86.00800855783791121, -282.9043949343772510, -329.8232844736725724 ) ) ;
#45978 = EDGE_CURVE ( 'NONE', #80198, #17402, #8985, .T. ) ;
#45979 = DIRECTION ( 'NONE',  ( 0.000000000000000000, 0.000000000000000000, 1.000000000000000000 ) ) ;
#45980 = CARTESIAN_POINT ( 'NONE',  ( 30.87753300788812183, -279.1415337807155765, -239.0746429105897732 ) ) ;
#45981 = CARTESIAN_POINT ( 'NONE',  ( 196.0143093133017658, 19.33012701892200624, -12.49999999999967315 ) ) ;
#45982 = CARTESIAN_POINT ( 'NONE',  ( -103.2084863280474281, -288.9106511079204438, -302.7447091870444638 ) ) ;
#45983 = CARTESIAN_POINT ( 'NONE',  ( -91.66117231297106116, -281.9762546710836659, -320.9601340027639367 ) ) ;
#45984 = DIRECTION ( 'NONE',  ( -1.000000000000000000, -0.000000000000000000, -0.000000000000000000 ) ) ;
#45985 = PLANE ( 'NONE',  #59418 ) ;
#45986 = CARTESIAN_POINT ( 'NONE',  ( -110.6221983677623371, -288.3462594548779521, -286.3886721057824616 ) ) ;
#45987 = CARTESIAN_POINT ( 'NONE',  ( 19.52161254829543324, -276.4141706651243453, -223.4860561065499382 ) ) ;
#45988 = CARTESIAN_POINT ( 'NONE',  ( -76.54144285373151035, -284.7690313170608079, -336.2358997747855369 ) ) ;
#45990 = CARTESIAN_POINT ( 'NONE',  ( -107.3919204476066795, -284.2798477619337518, -290.9475754062262354 ) ) ;
#45989 = CARTESIAN_POINT ( 'NONE',  ( -10.82952857014549508, -272.4748834278478284, -199.5493953235641413 ) ) ;
#45991 = CARTESIAN_POINT ( 'NONE',  ( -9.750733390642082554, -278.1098333078696783, -338.5958580393216835 ) ) ;
#45992 = CARTESIAN_POINT ( 'NONE',  ( 33.05602157532531749, -276.6182799060567277, -290.3258855133137786 ) ) ;
#45993 = CARTESIAN_POINT ( 'NONE',  ( -37.28939128864118402, -285.0516177112871787, -345.3738304341111416 ) ) ;
#45994 = ORIENTED_EDGE ( 'NONE', *, *, #17361, .T. ) ;
#45995 = AXIS2_PLACEMENT_3D ( 'NONE', #23848, #74501, #78145 ) ;
#45996 = CARTESIAN_POINT ( 'NONE',  ( 17.56005642389565224, -294.1273675208043983, -324.4258141224889869 ) ) ;
#45997 = CARTESIAN_POINT ( 'NONE',  ( 20.78037711548910949, -288.8841746420984009, -223.5042331719720323 ) ) ;
#45998 = DIRECTION ( 'NONE',  ( -0.000000000000000000, -1.000000000000000000, -0.000000000000000000 ) ) ;
#45999 = CARTESIAN_POINT ( 'NONE',  ( -55.56934967048407970, -295.3380690714490129, -190.3538533559490702 ) ) ;
#46000 = CARTESIAN_POINT ( 'NONE',  ( -109.4508417376092950, -277.1396206639161619, -296.6271607061277109 ) ) ;
#46001 = CARTESIAN_POINT ( 'NONE',  ( -50.40892337213931285, -290.2878514513459436, -195.2898978625418920 ) ) ;
#46002 = AXIS2_PLACEMENT_3D ( 'NONE', #61035, #53912, #4651 ) ;
#46003 = CARTESIAN_POINT ( 'NONE',  ( -73.91640162869806829, -287.0771190218803781, -206.3699321987036797 ) ) ;
#46004 = CARTESIAN_POINT ( 'NONE',  ( -108.0785445288762077, -280.0257549532776125, -292.3103683882536643 ) ) ;
#46005 = CARTESIAN_POINT ( 'NONE',  ( -12.90942351202142646, -287.7888671328199734, -197.9617384870416288 ) ) ;
#46006 = CARTESIAN_POINT ( 'NONE',  ( -2.674892394259778428, -284.5939880993105362, -336.8827497383002765 ) ) ;
#46007 = CARTESIAN_POINT ( 'NONE',  ( -37.12483438741440267, -277.2161514853956419, -347.3738713174889767 ) ) ;
#46008 = CARTESIAN_POINT ( 'NONE',  ( -96.03517150947493519, -271.1910895208134207, -223.9380111457722080 ) ) ;
#46009 = CARTESIAN_POINT ( 'NONE',  ( -113.7168233998692131, -278.5129797113544328, -260.1657597266293465 ) ) ;
#46010 = CARTESIAN_POINT ( 'NONE',  ( -63.61006337088689833, -299.6273817880021397, -200.6553922133440153 ) ) ;
#46011 = CIRCLE ( 'NONE', #71748, 5.103083949679981579 ) ;
#46012 = DIRECTION ( 'NONE',  ( -0.000000000000000000, 1.000000000000000000, -0.000000000000000000 ) ) ;
#46013 = CARTESIAN_POINT ( 'NONE',  ( 201.0776230153480526, -147.7221692137691775, -8.778910157967986905 ) ) ;
#46014 = CARTESIAN_POINT ( 'NONE',  ( -92.74309304641960239, -295.4085103196869113, -218.6029864861167482 ) ) ;
#46015 = CARTESIAN_POINT ( 'NONE',  ( 199.2296996224750103, 68.12454877777268791, 0.000000000000000000 ) ) ;
#46016 = CARTESIAN_POINT ( 'NONE',  ( -106.3243856189835839, -277.7380675174173348, -294.5848521435137286 ) ) ;
#46017 = AXIS2_PLACEMENT_3D ( 'NONE', #4608, #40563, #11710 ) ;
#46018 = CARTESIAN_POINT ( 'NONE',  ( -85.57019588733435000, -274.6068311208042019, -210.8462382106869484 ) ) ;
#46019 = CARTESIAN_POINT ( 'NONE',  ( 33.34456714679389933, -280.9946341135021157, -300.4346157586739992 ) ) ;
#46020 = CARTESIAN_POINT ( 'NONE',  ( 8.626594219994279555, -290.1724069398224515, -328.3687892476896764 ) ) ;
#46021 = CARTESIAN_POINT ( 'NONE',  ( -71.74396915942027420, -297.0186300703443862, -338.4727296244728336 ) ) ;
#46022 = CARTESIAN_POINT ( 'NONE',  ( -106.7998472985595697, -297.3416221479740216, -302.6655218481404290 ) ) ;
#46023 = CARTESIAN_POINT ( 'NONE',  ( 3.213180428380350229, -294.5981021519840510, -207.4083307871703994 ) ) ;
#46024 = CARTESIAN_POINT ( 'NONE',  ( 35.55184951805858162, -279.3341532099237270, -253.4330687393945425 ) ) ;
#46025 = CARTESIAN_POINT ( 'NONE',  ( -43.90188982336593426, -281.8888858114062259, -196.1595181270847092 ) ) ;
#46026 = CARTESIAN_POINT ( 'NONE',  ( -102.4627073117620597, -295.1153760193253675, -234.2977207662815715 ) ) ;
#46027 = CARTESIAN_POINT ( 'NONE',  ( -109.4608866148854531, -285.8390332502436308, -294.9632186082106386 ) ) ;
#46028 = CARTESIAN_POINT ( 'NONE',  ( 34.87431323413013473, -286.3030342111105142, -257.4620365605622396 ) ) ;
#46029 = CARTESIAN_POINT ( 'NONE',  ( 27.14702362586025686, -24.06158745657470632, -344.5372108056291154 ) ) ;
#46030 = EDGE_LOOP ( 'NONE', ( #62204, #59342, #13492, #40912, #9704, #49632 ) ) ;
#46031 = CARTESIAN_POINT ( 'NONE',  ( 33.48925405325685034, -286.4952012631553657, -299.1652243932525153 ) ) ;
#46032 = CARTESIAN_POINT ( 'NONE',  ( 35.47262882870926148, -287.2996604936064386, -276.4873326521638432 ) ) ;
#46033 = VERTEX_POINT ( 'NONE', #52545 ) ;
#46034 = CARTESIAN_POINT ( 'NONE',  ( -109.9276649085463475, -285.3186601792354509, -295.1153141182892341 ) ) ;
#46035 = CARTESIAN_POINT ( 'NONE',  ( 25.39590465244069506, -276.3989775775290241, -307.7252777231987579 ) ) ;
#46036 = CARTESIAN_POINT ( 'NONE',  ( -53.31147274504701272, -290.7724350610319561, -195.2971156415540293 ) ) ;
#46037 = CARTESIAN_POINT ( 'NONE',  ( 21.53732274481225772, -282.8704325085367373, -319.8239671978680576 ) ) ;
#46038 = LINE ( 'NONE', #10053, #2323 ) ;
#46039 = CARTESIAN_POINT ( 'NONE',  ( -106.7961564113329587, -280.4813262075144280, -238.6302487405615693 ) ) ;
#46040 = CARTESIAN_POINT ( 'NONE',  ( 35.30632078384844874, -281.5624724457769048, -244.7459096834286925 ) ) ;
#46041 = CARTESIAN_POINT ( 'NONE',  ( 30.89617123739170168, -279.2666405000204009, -285.9686137636504668 ) ) ;
#46042 = CARTESIAN_POINT ( 'NONE',  ( 168.7673636147504510, 232.2389198171512135, -192.7723113846432739 ) ) ;
#46043 = ORIENTED_EDGE ( 'NONE', *, *, #86610, .F. ) ;
#46044 = CARTESIAN_POINT ( 'NONE',  ( 25.53837903002381893, -278.1013100879092121, -311.0291679278843162 ) ) ;
#46045 = CARTESIAN_POINT ( 'NONE',  ( -108.3824614259837631, -261.6036692187849440, -317.2910301733635947 ) ) ;
#46046 = CARTESIAN_POINT ( 'NONE',  ( 5.895960732329615261, -278.6617934428740568, -209.5141666752244021 ) ) ;
#46047 = CARTESIAN_POINT ( 'NONE',  ( -108.5744972866913258, -296.1171096757910846, -253.9360981180980161 ) ) ;
#46048 = CARTESIAN_POINT ( 'NONE',  ( 36.30895030370150067, -293.3413636572570340, -292.7925800508041903 ) ) ;
#46049 = DIRECTION ( 'NONE',  ( 0.000000000000000000, 0.000000000000000000, 1.000000000000000000 ) ) ;
#46051 = CARTESIAN_POINT ( 'NONE',  ( -107.7211338833747760, -288.6588367221238514, -292.7378521487297576 ) ) ;
#46050 = CARTESIAN_POINT ( 'NONE',  ( -30.53152898055697406, -296.7105726661367271, -193.9519552065307835 ) ) ;
#46052 = CARTESIAN_POINT ( 'NONE',  ( -80.86004922154192798, -297.5103707697078903, -330.5027738455837039 ) ) ;
#46053 = CARTESIAN_POINT ( 'NONE',  ( -30.50195517935300771, -287.4554877727456415, -197.1357917279403864 ) ) ;
#46054 = CARTESIAN_POINT ( 'NONE',  ( 38.12814325710726138, -294.6704202427430914, -284.4722503976491339 ) ) ;
#46055 = CARTESIAN_POINT ( 'NONE',  ( -109.0386762002837457, -284.8592535442434155, -284.4157280420699294 ) ) ;
#46056 = CARTESIAN_POINT ( 'NONE',  ( -95.26074806815006468, -296.0285323846819097, -220.1482243354519994 ) ) ;
#46057 = CARTESIAN_POINT ( 'NONE',  ( -61.64721639579236268, -292.5471606104630382, -197.4119989845897862 ) ) ;
#46058 = CARTESIAN_POINT ( 'NONE',  ( -77.14280097261693925, -292.0264723446757102, -204.4559232188687474 ) ) ;
#46059 = CARTESIAN_POINT ( 'NONE',  ( -58.68710308437942302, -289.5025650551257286, -340.2234750382236825 ) ) ;
#46060 = EDGE_LOOP ( 'NONE', ( #1463, #59820, #14056, #10365 ) ) ;
#46061 = CARTESIAN_POINT ( 'NONE',  ( 157.3397966316789791, 16.44589409474655639, 9.145321187104725524 ) ) ;
#46062 = CARTESIAN_POINT ( 'NONE',  ( -54.34142713924888568, -299.6964516281937563, -196.5280985446813702 ) ) ;
#46063 = CARTESIAN_POINT ( 'NONE',  ( -69.94873143957963180, -272.4271628616909879, -201.0301858255633931 ) ) ;
#46064 = CARTESIAN_POINT ( 'NONE',  ( 3.511569450750162247, -281.5468631406942563, -331.2041848219550388 ) ) ;
#46065 = VERTEX_POINT ( 'NONE', #9449 ) ;
#46066 = CARTESIAN_POINT ( 'NONE',  ( -31.46123135671274085, -276.4875695285002166, -347.1271073884383895 ) ) ;
#46067 = CARTESIAN_POINT ( 'NONE',  ( -35.77790516194551884, -296.5519523500449282, -196.6681930200876707 ) ) ;
#46068 = CARTESIAN_POINT ( 'NONE',  ( -109.9683794781587665, -280.2131890049852245, -285.7309237709808940 ) ) ;
#46069 = CARTESIAN_POINT ( 'NONE',  ( 31.41323946870123862, -274.0620890358339921, -298.4910705554410129 ) ) ;
#46070 = CARTESIAN_POINT ( 'NONE',  ( -109.5298882069641877, -297.5822606652396303, -283.6970119927557334 ) ) ;
#46071 = CARTESIAN_POINT ( 'NONE',  ( -109.3633214737600099, -273.6715681474125290, -256.8120217745229183 ) ) ;
#46072 = CARTESIAN_POINT ( 'NONE',  ( -94.97949383970086501, -298.8332832250812885, -220.4393361434963197 ) ) ;
#46073 = CARTESIAN_POINT ( 'NONE',  ( -21.67168307186484810, -272.2721735945495993, -196.6531986982309945 ) ) ;
#46074 = CARTESIAN_POINT ( 'NONE',  ( 34.04755592211761694, -293.9955752367482660, -254.5721886120804811 ) ) ;
#46075 = CARTESIAN_POINT ( 'NONE',  ( -47.05441299881726280, -290.5010844398804011, -197.4156717577427571 ) ) ;
#46076 = CARTESIAN_POINT ( 'NONE',  ( 115.2448031289451222, -299.5541904835127980, -195.3611179825600175 ) ) ;
#46077 = CARTESIAN_POINT ( 'NONE',  ( -75.30037756694086681, -278.0365520000658535, -337.2839519808595128 ) ) ;
#46078 = CARTESIAN_POINT ( 'NONE',  ( -47.27982467328074989, -298.2558154095355007, -197.9681949448096248 ) ) ;
#46079 = CARTESIAN_POINT ( 'NONE',  ( 6.627811149647447664, -281.1532837015721498, -333.0356375875309141 ) ) ;
#46080 = CARTESIAN_POINT ( 'NONE',  ( -58.31476465329029679, -297.3226295194288014, -342.5967924246133407 ) ) ;
#46081 = DIRECTION ( 'NONE',  ( 0.000000000000000000, 0.000000000000000000, 1.000000000000000000 ) ) ;
#46082 = CARTESIAN_POINT ( 'NONE',  ( -59.00567902545960663, -282.5367725711949447, -340.2948043582983360 ) ) ;
#46083 = AXIS2_PLACEMENT_3D ( 'NONE', #1403, #52061, #22 ) ;
#46084 = CARTESIAN_POINT ( 'NONE',  ( -69.70443733715549683, -281.4769820109128204, -338.2183035407334728 ) ) ;
#46085 = CARTESIAN_POINT ( 'NONE',  ( 34.08544686764336262, -273.8950887982017548, -252.6541252724424567 ) ) ;
#46086 = CARTESIAN_POINT ( 'NONE',  ( 31.97045156365387797, -283.1769049838175647, -241.5774200847378665 ) ) ;
#46087 = FACE_OUTER_BOUND ( 'NONE', #16809, .T. ) ;
#46088 = CARTESIAN_POINT ( 'NONE',  ( 197.5379522065468052, 250.5000000000000568, -11.97918851819044050 ) ) ;
#46089 = CARTESIAN_POINT ( 'NONE',  ( 0.8126862128197108737, -272.9520237599154484, -204.3862805540542809 ) ) ;
#46090 = TOROIDAL_SURFACE ( 'NONE', #11361, 154.4364916446740210, 1.000000000000000000 ) ;
#46091 = CARTESIAN_POINT ( 'NONE',  ( -112.5441497201053522, -280.5723370762114541, -268.7983991541806859 ) ) ;
#46092 = EDGE_CURVE ( 'NONE', #90266, #50020, #60607, .T. ) ;
#46093 = DIRECTION ( 'NONE',  ( 1.000000000000000000, 0.000000000000000000, 0.000000000000000000 ) ) ;
#46094 = CARTESIAN_POINT ( 'NONE',  ( 32.51853913141793129, -289.0978927903359477, -241.4345894216269244 ) ) ;
#46095 =( LENGTH_UNIT ( ) NAMED_UNIT ( * ) SI_UNIT ( .MILLI., .METRE. ) );
#46096 = CARTESIAN_POINT ( 'NONE',  ( -97.83258073832952562, -289.1567327142652175, -226.0017343830446634 ) ) ;
#46097 = CARTESIAN_POINT ( 'NONE',  ( 175.2296996224750103, 275.0000000000000568, -24.00000000000000355 ) ) ;
#46098 = CARTESIAN_POINT ( 'NONE',  ( -82.61674104850737876, -294.4812464764269180, -328.1953066264362064 ) ) ;
#46099 = CARTESIAN_POINT ( 'NONE',  ( -98.37777008258306921, -288.1125832734024357, -312.6382074147545040 ) ) ;
#46100 = CARTESIAN_POINT ( 'NONE',  ( 175.8323451578035872, 256.8656992060370499, -165.6361338323774817 ) ) ;
#46101 = CARTESIAN_POINT ( 'NONE',  ( -110.8499041012236432, -294.3600576685423675, -285.3095547068453470 ) ) ;
#46102 = CARTESIAN_POINT ( 'NONE',  ( 36.46880007786586475, -286.2765498069288128, -289.7187473239187057 ) ) ;
#46103 = CARTESIAN_POINT ( 'NONE',  ( 22.75321873640402970, -282.5603315451539856, -227.5237377775503376 ) ) ;
#46104 = CARTESIAN_POINT ( 'NONE',  ( -71.30618411785034993, -281.7343057551539118, -338.3345528254463375 ) ) ;
#46105 = CARTESIAN_POINT ( 'NONE',  ( -109.4191042533716001, -290.3984972085565346, -282.0090036074795989 ) ) ;
#46106 = CARTESIAN_POINT ( 'NONE',  ( 36.10685697529019933, -282.9179161881680216, -265.8131101515400019 ) ) ;
#46107 = CARTESIAN_POINT ( 'NONE',  ( 35.72770680629005113, -282.4032864712268633, -274.0303817727408955 ) ) ;
#46108 = CLOSED_SHELL ( 'NONE', ( #7407, #41066, #31463, #70445, #29564, #85656, #91968, #67860, #81368, #34993, #13470, #44102, #89366, #78399, #74868, #76860, #3072, #46345, #46385 ) ) ;
#46109 = CARTESIAN_POINT ( 'NONE',  ( 6.987731734248881388, -290.4323270380440363, -331.3623997911580545 ) ) ;
#46110 = CARTESIAN_POINT ( 'NONE',  ( -35.47404145034176537, -298.2416097282461465, -193.3610667654473048 ) ) ;
#46111 = EDGE_LOOP ( 'NONE', ( #90811, #30576, #3928, #90125, #72298 ) ) ;
#46112 = CARTESIAN_POINT ( 'NONE',  ( 36.49346288353235934, -275.8267837741274775, -292.2564064448038152 ) ) ;
#46113 = CARTESIAN_POINT ( 'NONE',  ( -17.00823401897600107, -294.2957439519510103, -198.4853655749896859 ) ) ;
#46114 = FACE_OUTER_BOUND ( 'NONE', #82391, .T. ) ;
#46115 = CARTESIAN_POINT ( 'NONE',  ( -54.49178911615187815, -288.3376638359845856, -195.3683826091709363 ) ) ;
#46116 = CARTESIAN_POINT ( 'NONE',  ( 34.72823422483048006, -273.8269462194310790, -291.7595326021432243 ) ) ;
#46117 = DIRECTION ( 'NONE',  ( -6.570707696761130958E-14, 0.000000000000000000, 1.000000000000000000 ) ) ;
#46118 = CARTESIAN_POINT ( 'NONE',  ( -59.89169825058520047, -296.1647467918778034, -197.5192424894375733 ) ) ;
#46119 = CARTESIAN_POINT ( 'NONE',  ( -109.1238519256437485, -291.9286130720112169, -287.5006366707467578 ) ) ;
#46120 = CARTESIAN_POINT ( 'NONE',  ( -6.478410830761558437, -273.8171486289658674, -204.0938557613360160 ) ) ;
#46121 = CARTESIAN_POINT ( 'NONE',  ( -88.42502221032009402, -292.8408530846274402, -217.1755890785530312 ) ) ;
#46122 = CARTESIAN_POINT ( 'NONE',  ( -95.30795483998606699, -292.1215232765439396, -225.6026353951364172 ) ) ;
#46123 = CARTESIAN_POINT ( 'NONE',  ( -109.9695987778565893, -286.1268425734511993, -284.6146211767700152 ) ) ;
#46124 = CARTESIAN_POINT ( 'NONE',  ( -113.8003228525353308, -291.9663440890844299, -271.2402333106921333 ) ) ;
#46125 = CARTESIAN_POINT ( 'NONE',  ( -37.80893251760928564, -293.3615821891834230, -193.8556935414138991 ) ) ;
#46126 = CARTESIAN_POINT ( 'NONE',  ( 6.061235767508152961, -294.2782533263938376, -329.1198124285405129 ) ) ;
#46127 = CARTESIAN_POINT ( 'NONE',  ( 33.29128194310850120, -289.8791274019168327, -295.5798112708931171 ) ) ;
#46128 = CARTESIAN_POINT ( 'NONE',  ( 29.76294148372031501, -282.2099935017037637, -308.2317696016779678 ) ) ;
#46129 = CARTESIAN_POINT ( 'NONE',  ( 6.960833408849198989, -296.6824680553923486, -194.8154681501593757 ) ) ;
#46130 = CARTESIAN_POINT ( 'NONE',  ( -60.50789903976123441, -285.5932377349557214, -196.8730753921845462 ) ) ;
#46131 = CARTESIAN_POINT ( 'NONE',  ( 37.34497197834174642, -277.5478703728319942, -271.5873799267992013 ) ) ;
#46132 = CARTESIAN_POINT ( 'NONE',  ( -87.20981319408446097, -282.5603489076043502, -324.2851145895770628 ) ) ;
#46133 = CARTESIAN_POINT ( 'NONE',  ( 20.56273307833539477, -284.8945380617355454, -222.6948063175437369 ) ) ;
#46134 = CARTESIAN_POINT ( 'NONE',  ( -77.18580578217274990, -275.7193696026913585, -334.8639504470550037 ) ) ;
#46135 = CARTESIAN_POINT ( 'NONE',  ( 153.6539576904058038, 130.0000000000000568, 12.50000000000000000 ) ) ;
#46136 = CARTESIAN_POINT ( 'NONE',  ( -4.805385398037338440, -282.1192531753392814, -335.7780627725132376 ) ) ;
#46137 = CARTESIAN_POINT ( 'NONE',  ( -35.36175165022358868, -281.2815239598371022, -193.7707118762414780 ) ) ;
#46138 = CARTESIAN_POINT ( 'NONE',  ( 37.15140899565254529, -286.3782900832634937, -251.8247508377432951 ) ) ;
#46139 = CARTESIAN_POINT ( 'NONE',  ( 8.878219529811792299, -296.1687571370302408, -328.2343802652337672 ) ) ;
#46140 = CARTESIAN_POINT ( 'NONE',  ( 38.58511446579264970, -277.2337496475062721, -276.8077635946577857 ) ) ;
#46141 = CARTESIAN_POINT ( 'NONE',  ( 39.21410212106193427, -276.8772512868949889, -271.1497358663002615 ) ) ;
#46142 = CARTESIAN_POINT ( 'NONE',  ( -95.27431517163964259, -277.7605854553406175, -314.7774676608826212 ) ) ;
#46143 = CARTESIAN_POINT ( 'NONE',  ( -42.00746948066868924, -299.9933605363592051, -195.6733745165925029 ) ) ;
#46144 = CARTESIAN_POINT ( 'NONE',  ( 32.17915235270469054, -285.9150837590440801, -298.1933438291356424 ) ) ;
#46145 = CARTESIAN_POINT ( 'NONE',  ( -111.5429616737715293, -292.3713940528133435, -253.0229172766923398 ) ) ;
#46146 = CARTESIAN_POINT ( 'NONE',  ( -71.08526816811954063, -294.4287426400462095, -335.4566322670959266 ) ) ;
#46147 = ORIENTED_EDGE ( 'NONE', *, *, #82544, .T. ) ;
#46148 = CARTESIAN_POINT ( 'NONE',  ( 29.87687044034836958, -292.8344390153208110, -241.7054125770505095 ) ) ;
#46149 = ORIENTED_EDGE ( 'NONE', *, *, #68345, .F. ) ;
#46150 = CARTESIAN_POINT ( 'NONE',  ( 0.5784681257780236452, -289.6390423541757855, -337.0811170808499355 ) ) ;
#46151 = CARTESIAN_POINT ( 'NONE',  ( -83.50852691119169435, -280.0512935461091502, -213.6165257675015141 ) ) ;
#46152 = CARTESIAN_POINT ( 'NONE',  ( -106.8918469178613577, -295.0572427316778317, -302.6762783627173690 ) ) ;
#46153 = CARTESIAN_POINT ( 'NONE',  ( 38.87313931373427067, -288.0754790186344394, -260.1331643561269971 ) ) ;
#46154 = CARTESIAN_POINT ( 'NONE',  ( 24.68371495242304547, -287.2796616143220376, -224.7695378862669600 ) ) ;
#46155 = CARTESIAN_POINT ( 'NONE',  ( -108.7398411792730144, -284.6827468380653272, -285.7303862886270167 ) ) ;
#46156 = CARTESIAN_POINT ( 'NONE',  ( -22.58273187487147382, -108.0340517555389539, -362.5798773164099202 ) ) ;
#46157 = CARTESIAN_POINT ( 'NONE',  ( -96.21878309525817485, -238.5862671180402970, -340.1699584742321463 ) ) ;
#46158 = CARTESIAN_POINT ( 'NONE',  ( -94.19091026945986300, -238.5270531376727092, -338.5184284098635885 ) ) ;
#46159 = PRODUCT_DEFINITION_FORMATION_WITH_SPECIFIED_SOURCE ( 'ANY', '', #83658, .NOT_KNOWN. ) ;
#46160 = CARTESIAN_POINT ( 'NONE',  ( -66.87720454847166707, -276.6465701445121113, -337.2958302476669132 ) ) ;
#46161 = CARTESIAN_POINT ( 'NONE',  ( -71.81163762643308246, -276.4393281188836227, -335.0749653636798939 ) ) ;
#46162 = CARTESIAN_POINT ( 'NONE',  ( -29.06155764960093535, -297.6608735929614227, -193.4233259703201213 ) ) ;
#46163 = CARTESIAN_POINT ( 'NONE',  ( -61.49889831844556909, -183.5886210442853326, -359.5431637745206785 ) ) ;
#46164 = CARTESIAN_POINT ( 'NONE',  ( -35.73874141804396487, -275.7173027604336539, -346.8642145531776464 ) ) ;
#46165 = CARTESIAN_POINT ( 'NONE',  ( -72.38287194409117831, -290.0216038275953565, -334.4712164034065154 ) ) ;
#46166 = CARTESIAN_POINT ( 'NONE',  ( -46.12159095762173422, -298.7463025151313332, -194.0258552446377394 ) ) ;
#46167 = CARTESIAN_POINT ( 'NONE',  ( -34.05652319490675950, -298.5845947084019372, -193.4223898508425918 ) ) ;
#46168 = CARTESIAN_POINT ( 'NONE',  ( 12.35642799949807191, -294.5037644111103532, -323.9009182221352603 ) ) ;
#46169 = VERTEX_POINT ( 'NONE', #88052 ) ;
#46170 = CARTESIAN_POINT ( 'NONE',  ( -38.49793388571393393, -278.9866928105701049, -345.9122749908211176 ) ) ;
#46171 = CARTESIAN_POINT ( 'NONE',  ( -47.25464769423852118, -282.6825557864519851, -346.6583025549425088 ) ) ;
#46172 = CARTESIAN_POINT ( 'NONE',  ( -109.7954839753122229, -279.4851534149324266, -281.5269265103479484 ) ) ;
#46173 = CARTESIAN_POINT ( 'NONE',  ( -42.71188665963277487, -278.8791768597490091, -346.1577875048786836 ) ) ;
#46174 = CARTESIAN_POINT ( 'NONE',  ( -47.33494322860493497, -296.4975451618913098, -197.4019512077545926 ) ) ;
#46175 = DIRECTION ( 'NONE',  ( 0.000000000000000000, -1.000000000000000000, 0.000000000000000000 ) ) ;
#46176 = CARTESIAN_POINT ( 'NONE',  ( -108.7643344056090626, -278.5197271859262287, -285.4544051458017861 ) ) ;
#46177 = CARTESIAN_POINT ( 'NONE',  ( -38.36553560907224636, -274.8424518016485081, -193.5294150068752401 ) ) ;
#46178 = CARTESIAN_POINT ( 'NONE',  ( 9.910132642451632279, -287.1018647103783792, -330.5996140805041819 ) ) ;
#46179 = CARTESIAN_POINT ( 'NONE',  ( -68.04912357407837931, -275.6491723184861939, -201.9215521663130630 ) ) ;
#46180 = CARTESIAN_POINT ( 'NONE',  ( 39.11759607059777011, -274.1372459535500639, -271.1835561986710559 ) ) ;
#46181 = DIRECTION ( 'NONE',  ( 1.000000000000000000, 0.000000000000000000, 0.000000000000000000 ) ) ;
#46182 = CARTESIAN_POINT ( 'NONE',  ( -74.80735642719723444, -288.7618933278195641, -333.2163215201099433 ) ) ;
#46183 = CARTESIAN_POINT ( 'NONE',  ( -69.74232232338688675, -284.9852853829084438, -200.6078844102750054 ) ) ;
#46184 = EDGE_CURVE ( 'NONE', #66186, #26725, #81420, .T. ) ;
#46185 = CARTESIAN_POINT ( 'NONE',  ( -15.85949873780902486, -281.0102811206787692, -341.1882952171815191 ) ) ;
#46187 = CARTESIAN_POINT ( 'NONE',  ( -60.40195178713290147, -283.8306126534583314, -199.5830211613755978 ) ) ;
#46186 = CARTESIAN_POINT ( 'NONE',  ( 22.27874692674471291, -280.7257744381483917, -313.5194134312836240 ) ) ;
#46188 = CARTESIAN_POINT ( 'NONE',  ( -32.53978009027839136, -290.9919073492675352, -345.2577204400344613 ) ) ;
#46189 = CARTESIAN_POINT ( 'NONE',  ( 19.13184210540476826, -282.0957184221804255, -223.4601759565237842 ) ) ;
#46190 = CARTESIAN_POINT ( 'NONE',  ( 201.7240241153841396, 293.7293971333333502, -83.18315278848760386 ) ) ;
#46191 = CARTESIAN_POINT ( 'NONE',  ( -16.38165683845463505, -281.1856673722065807, -343.6764346845136515 ) ) ;
#46192 = CARTESIAN_POINT ( 'NONE',  ( 12.09710782999317935, -296.3652147601297884, -326.8286230029559079 ) ) ;
#46193 = CARTESIAN_POINT ( 'NONE',  ( -95.12050561012156891, -277.4667845066937275, -220.9895076386954429 ) ) ;
#46194 = CARTESIAN_POINT ( 'NONE',  ( -33.13525807552652935, -284.9994731475740650, -345.4228192937957260 ) ) ;
#46195 = DIRECTION ( 'NONE',  ( 0.000000000000000000, 0.000000000000000000, 1.000000000000000000 ) ) ;
#46196 = CARTESIAN_POINT ( 'NONE',  ( -9.073077035165718840, -294.3391085262769593, -200.2883048003837132 ) ) ;
#46197 = CARTESIAN_POINT ( 'NONE',  ( -9.262593979212509154, -274.6849535548248582, -339.9204659320925543 ) ) ;
#46198 = CARTESIAN_POINT ( 'NONE',  ( 37.56451522790833053, -286.5340600598635206, -253.1790870622292573 ) ) ;
#46199 = CARTESIAN_POINT ( 'NONE',  ( -108.1572578066967196, -289.2244274860439646, -249.5413717850366311 ) ) ;
#46200 = CARTESIAN_POINT ( 'NONE',  ( -43.36966085509969560, -266.0730555875976506, -435.0432476903218344 ) ) ;
#46201 = CARTESIAN_POINT ( 'NONE',  ( -32.40404411641769400, -275.6735592464879687, -343.7385183722637407 ) ) ;
#46202 = CARTESIAN_POINT ( 'NONE',  ( -56.13857124124354669, -293.4362809411676949, -342.2304293144740654 ) ) ;
#46203 = CARTESIAN_POINT ( 'NONE',  ( -80.68493099996972262, -290.9688177891488863, -329.7759957522601439 ) ) ;
#46204 = DIRECTION ( 'NONE',  ( -0.8510748438184358999, -0.5250018354872690862, -0.006684530980050039546 ) ) ;
#46205 = DIRECTION ( 'NONE',  ( 0.000000000000000000, 0.000000000000000000, -1.000000000000000000 ) ) ;
#46206 = CARTESIAN_POINT ( 'NONE',  ( 30.29343671947234640, -291.5708014247982760, -234.9174954872486296 ) ) ;
#46207 = CARTESIAN_POINT ( 'NONE',  ( -37.30066544658166805, -287.6527672658560277, -196.5485513742615069 ) ) ;
#46208 = CARTESIAN_POINT ( 'NONE',  ( -38.92187258964147389, -287.3115867626428894, -346.3313560473806660 ) ) ;
#46209 = EDGE_CURVE ( 'NONE', #69284, #12630, #45906, .T. ) ;
#46210 = CARTESIAN_POINT ( 'NONE',  ( 35.57749773118361958, -288.8429135475420821, -260.0817373403651231 ) ) ;
#46211 = CARTESIAN_POINT ( 'NONE',  ( 209.4803090767392462, 35.69423656899339647, 14.26380412667038833 ) ) ;
#46212 = CARTESIAN_POINT ( 'NONE',  ( 35.61377461783489906, -288.4355912920238438, -276.4846964328231138 ) ) ;
#46213 = CARTESIAN_POINT ( 'NONE',  ( -70.07020273953243361, -297.4609553166690716, -338.2520569839953737 ) ) ;
#46214 = FACE_OUTER_BOUND ( 'NONE', #75969, .T. ) ;
#46215 = CARTESIAN_POINT ( 'NONE',  ( 32.34439647979730381, -288.3470231621623157, -238.4237866358001838 ) ) ;
#46216 = CARTESIAN_POINT ( 'NONE',  ( -68.44538412627868240, -275.5374287157678168, -339.2365295896872794 ) ) ;
#46217 = CARTESIAN_POINT ( 'NONE',  ( -65.08348895615139895, -277.7380180020664397, -342.2236364944200773 ) ) ;
#46218 = CARTESIAN_POINT ( 'NONE',  ( 12.98155465945337461, -280.3995669858319957, -212.1089564859341863 ) ) ;
#46219 = CARTESIAN_POINT ( 'NONE',  ( -33.73733337003511679, -300.0773764445695519, -195.7150858637083957 ) ) ;
#46220 = CARTESIAN_POINT ( 'NONE',  ( -43.41710851680167593, -261.3366415040296715, -500.0926372755047851 ) ) ;
#46221 = CARTESIAN_POINT ( 'NONE',  ( -95.66159568953476366, -283.2013669031691734, -223.1836902519604848 ) ) ;
#46222 = CARTESIAN_POINT ( 'NONE',  ( -48.18343439339131606, -256.8217696174598927, -487.2503612923801484 ) ) ;
#46223 = CARTESIAN_POINT ( 'NONE',  ( -106.6593017720220047, -277.0423655071184044, -243.6478120152501674 ) ) ;
#46224 = CARTESIAN_POINT ( 'NONE',  ( 35.59721309109747978, -279.7768593533121475, -287.8776510799567632 ) ) ;
#46225 = DIRECTION ( 'NONE',  ( -0.000000000000000000, 1.000000000000000000, 0.000000000000000000 ) ) ;
#46226 = CARTESIAN_POINT ( 'NONE',  ( -8.167785558938920332, -275.1568502994144865, -340.8847784349513290 ) ) ;
#46227 = CARTESIAN_POINT ( 'NONE',  ( -110.7885212765913394, -297.9857752888462983, -276.9810065763996363 ) ) ;
#46228 = CARTESIAN_POINT ( 'NONE',  ( -19.00568053621997322, -281.7419514220003407, -344.8825090160722766 ) ) ;
#46229 = CARTESIAN_POINT ( 'NONE',  ( -108.0660035123709690, -297.7442958759102112, -251.3001007439489172 ) ) ;
#46230 = CARTESIAN_POINT ( 'NONE',  ( -35.85699853961065031, -299.3855416260925040, -193.8539410945947452 ) ) ;
#46231 = CARTESIAN_POINT ( 'NONE',  ( -34.03547643599088701, -273.7615982031505268, -197.4148612470219746 ) ) ;
#46232 = CARTESIAN_POINT ( 'NONE',  ( 37.28268231497051488, -295.4496335698748908, -262.3640191090117355 ) ) ;
#46233 = CARTESIAN_POINT ( 'NONE',  ( 38.67532562284709030, -287.8762676522165407, -282.9495830547723472 ) ) ;
#46234 = CARTESIAN_POINT ( 'NONE',  ( -104.8773269271692641, -277.0775491069227883, -236.3587750604658879 ) ) ;
#46235 = CARTESIAN_POINT ( 'NONE',  ( -96.57750882963703987, -291.0471746808080979, -221.1460381611533705 ) ) ;
#46236 = CARTESIAN_POINT ( 'NONE',  ( 20.53605821534826603, -287.2410821642815790, -315.2542774257673273 ) ) ;
#46237 = CARTESIAN_POINT ( 'NONE',  ( -2.949655718037113239, -290.5064174255074363, -203.6969813962691944 ) ) ;
#46238 = ORIENTED_EDGE ( 'NONE', *, *, #10780, .F. ) ;
#46239 = CARTESIAN_POINT ( 'NONE',  ( -114.4693268140674434, -273.6886850827510216, -284.2063049943780015 ) ) ;
#46240 = CARTESIAN_POINT ( 'NONE',  ( 32.37044432901250701, -287.3513885459868789, -292.3973599499830129 ) ) ;
#46241 = CARTESIAN_POINT ( 'NONE',  ( 207.5863589332323329, 29.28491128719180026, 13.57731244650625513 ) ) ;
#46242 = CARTESIAN_POINT ( 'NONE',  ( -110.8791176002514902, -285.2156470433626509, -292.4310086095234738 ) ) ;
#46243 = CARTESIAN_POINT ( 'NONE',  ( 39.00173524470162789, -292.7177781905338634, -278.8806994840650191 ) ) ;
#46244 = CARTESIAN_POINT ( 'NONE',  ( 36.50458824150194204, -282.6146664768839400, -250.3108789574148716 ) ) ;
#46245 = CARTESIAN_POINT ( 'NONE',  ( -21.39028187699264194, -282.6752953878387302, -341.6490221656364952 ) ) ;
#46246 = CARTESIAN_POINT ( 'NONE',  ( -102.3163945606061134, -297.0937311082029169, -229.0417631545857375 ) ) ;
#46247 = CARTESIAN_POINT ( 'NONE',  ( -48.96986659486070437, -275.2162387408656627, -197.7421859769735022 ) ) ;
#46248 = CARTESIAN_POINT ( 'NONE',  ( -60.75140536285802995, -289.7671641781465155, -199.4278911509432533 ) ) ;
#46249 = CARTESIAN_POINT ( 'NONE',  ( -29.93461739507998942, -272.9429115437400810, -197.3387540790971570 ) ) ;
#46250 = ORIENTED_EDGE ( 'NONE', *, *, #67393, .F. ) ;
#46251 = CARTESIAN_POINT ( 'NONE',  ( 208.6208076322478746, 32.98517505407394168, 9.000000000000001776 ) ) ;
#46252 = CARTESIAN_POINT ( 'NONE',  ( -8.966684677925307767, -288.3463165669435853, -201.5274890656250193 ) ) ;
#46253 = CARTESIAN_POINT ( 'NONE',  ( -11.14980158982232794, -295.7984535440176046, -342.4971213971670636 ) ) ;
#46254 = CARTESIAN_POINT ( 'NONE',  ( -108.7662776926124479, -285.4094440141853397, -254.7327277577390987 ) ) ;
#46255 = CARTESIAN_POINT ( 'NONE',  ( 39.08426611691788111, -274.5137425103191617, -262.6160379171742534 ) ) ;
#46256 = CARTESIAN_POINT ( 'NONE',  ( -16.66200996197529349, -292.9639359549618121, -196.2958548632652764 ) ) ;
#46257 = CARTESIAN_POINT ( 'NONE',  ( 19.37805501915875084, -284.9995547954317203, -220.0524283685683997 ) ) ;
#46258 = CARTESIAN_POINT ( 'NONE',  ( 23.15769014751301214, -294.5223369966837481, -317.9802518562189562 ) ) ;
#46259 = CARTESIAN_POINT ( 'NONE',  ( -110.2670399689955190, -290.9463977190860078, -265.7385080512584636 ) ) ;
#46260 = LINE ( 'NONE', #89336, #39844 ) ;
#46261 = DIRECTION ( 'NONE',  ( 0.8457827187922972723, 0.5335274993777825436, 0.000000000000000000 ) ) ;
#46262 = CARTESIAN_POINT ( 'NONE',  ( -30.06861358815306318, -125.2304951651611020, -360.6161781973373763 ) ) ;
#46263 = CARTESIAN_POINT ( 'NONE',  ( -65.63840940208109487, -287.2088798734749844, -199.4809900978910946 ) ) ;
#46264 = CARTESIAN_POINT ( 'NONE',  ( -72.02372285203398405, -271.1237833571632905, -198.2697987213421698 ) ) ;
#46265 = VERTEX_POINT ( 'NONE', #53010 ) ;
#46266 = CARTESIAN_POINT ( 'NONE',  ( -108.0629762411944768, -283.2179300521741538, -289.7146892801354170 ) ) ;
#46267 = CARTESIAN_POINT ( 'NONE',  ( -82.53729739451570424, -277.3177300720651033, -332.6756610617824208 ) ) ;
#46268 = CARTESIAN_POINT ( 'NONE',  ( 36.51702530783049383, -283.7072261746205299, -282.3992700271738272 ) ) ;
#46269 = CARTESIAN_POINT ( 'NONE',  ( -54.04194081808444139, -170.5257408106840558, -363.2615279374122679 ) ) ;
#46270 = CARTESIAN_POINT ( 'NONE',  ( -66.36934788348081327, -281.9995673580031053, -341.0575990416611489 ) ) ;
#46271 = CARTESIAN_POINT ( 'NONE',  ( 35.31704978269277007, -285.3508884591338983, -253.2016229601303792 ) ) ;
#46272 = CARTESIAN_POINT ( 'NONE',  ( -101.6827884767155012, -274.9444500212786124, -230.3544956636292511 ) ) ;
#46273 = CARTESIAN_POINT ( 'NONE',  ( -58.42000539663133907, -295.8244719080564664, -340.3160569684570191 ) ) ;
#46274 = ORIENTED_EDGE ( 'NONE', *, *, #67056, .F. ) ;
#46275 = CARTESIAN_POINT ( 'NONE',  ( -47.04309644520665756, -290.6111649840099176, -197.5110913060013331 ) ) ;
#46276 = CARTESIAN_POINT ( 'NONE',  ( -113.6640153480350932, -279.0806679341160361, -280.1747311104796268 ) ) ;
#46277 = CARTESIAN_POINT ( 'NONE',  ( 35.60193609077818877, -275.6042791801405087, -274.3126303681194713 ) ) ;
#46278 = CARTESIAN_POINT ( 'NONE',  ( 30.26405250746054421, -274.9436141718023805, -306.6803198339683831 ) ) ;
#46279 = DIRECTION ( 'NONE',  ( 0.000000000000000000, 0.000000000000000000, 1.000000000000000000 ) ) ;
#46280 = CARTESIAN_POINT ( 'NONE',  ( -33.50494521547745563, -272.1002650189423662, -195.4466888876256974 ) ) ;
#46281 = EDGE_CURVE ( 'NONE', #16269, #19500, #57276, .T. ) ;
#46282 = CARTESIAN_POINT ( 'NONE',  ( -11.24128429275440233, -296.1439987217785301, -342.2321231324961559 ) ) ;
#46283 = CARTESIAN_POINT ( 'NONE',  ( 152.4536156746142410, 129.7208004331680797, 12.50000000000000000 ) ) ;
#46284 = CARTESIAN_POINT ( 'NONE',  ( 198.7350614680083538, 66.75098366858709653, 10.35296668938518216 ) ) ;
#46285 = CARTESIAN_POINT ( 'NONE',  ( -110.6187084289727949, -285.6603267123361434, -268.1917569814370381 ) ) ;
#46286 = CARTESIAN_POINT ( 'NONE',  ( -24.68006851802043400, -284.6530082800641139, -345.3388667412988866 ) ) ;
#46287 = CARTESIAN_POINT ( 'NONE',  ( -78.44077709836832923, -282.9703452669656372, -330.8157169816710166 ) ) ;
#46288 = CARTESIAN_POINT ( 'NONE',  ( 10.16362670252486566, -274.7839992825527702, -326.8384084257006066 ) ) ;
#46289 = CARTESIAN_POINT ( 'NONE',  ( 26.63537936562969222, -283.9223222138413121, -308.1164186136542753 ) ) ;
#46290 = CARTESIAN_POINT ( 'NONE',  ( -67.10022423793390089, -275.9293967296944174, -337.7787565998945070 ) ) ;
#46291 = CARTESIAN_POINT ( 'NONE',  ( 20.27390275724414437, -277.2687251126907881, -315.7097886556133517 ) ) ;
#46292 = FACE_OUTER_BOUND ( 'NONE', #45579, .T. ) ;
#46293 = CARTESIAN_POINT ( 'NONE',  ( -94.84774534786933486, -280.0468785297908880, -219.3982532288467837 ) ) ;
#46294 = CARTESIAN_POINT ( 'NONE',  ( -62.03382016110933250, -280.2320118665113569, -197.4363751072278887 ) ) ;
#46295 = ORIENTED_EDGE ( 'NONE', *, *, #49739, .F. ) ;
#46296 = CARTESIAN_POINT ( 'NONE',  ( 197.3380612925967057, 18.22700036951244584, -11.15593255764697567 ) ) ;
#46297 = CARTESIAN_POINT ( 'NONE',  ( 38.37123740727610510, -289.4630672738114754, -274.3341554334433567 ) ) ;
#46298 = CARTESIAN_POINT ( 'NONE',  ( -108.1284044367303778, -295.5051595200919223, -288.8997070272046699 ) ) ;
#46299 = CARTESIAN_POINT ( 'NONE',  ( -71.86814614747392227, -288.8451493913223089, -339.0723784303086745 ) ) ;
#46300 = ADVANCED_FACE ( 'NONE', ( #38801 ), #24602, .T. ) ;
#46301 = CARTESIAN_POINT ( 'NONE',  ( 3.018101175348274268, -284.8421288870412127, -208.3203213164763667 ) ) ;
#46303 = CARTESIAN_POINT ( 'NONE',  ( -103.7645765641147051, -288.3556749469547071, -303.0103981713608619 ) ) ;
#46302 = CARTESIAN_POINT ( 'NONE',  ( -9.251810149712797582, -285.0014304847313724, -202.3303471054953206 ) ) ;
#46304 = CARTESIAN_POINT ( 'NONE',  ( -91.82623210097115418, -286.4583933362018229, -221.1074983045434976 ) ) ;
#46305 = CARTESIAN_POINT ( 'NONE',  ( -48.22949183385324545, -275.1904010738356874, -344.6191174926257759 ) ) ;
#46306 = CARTESIAN_POINT ( 'NONE',  ( 11.88335065627740761, -286.7811178905666907, -328.5275583819951635 ) ) ;
#46307 = CARTESIAN_POINT ( 'NONE',  ( 20.53024547613670237, -288.8942117152043352, -222.6553681751702243 ) ) ;
#46308 = CARTESIAN_POINT ( 'NONE',  ( 21.82814721845769412, -286.1869833289202347, -316.7386852402980821 ) ) ;
#46309 = CARTESIAN_POINT ( 'NONE',  ( 14.09845758317911013, -283.2496735033903974, -322.5604379622570264 ) ) ;
#46310 = CARTESIAN_POINT ( 'NONE',  ( 19.21079913231912073, -290.2386823653113197, -319.8966076060448245 ) ) ;
#46311 = DIRECTION ( 'NONE',  ( -1.000000000000000000, 0.000000000000000000, 0.000000000000000000 ) ) ;
#46312 = DIRECTION ( 'NONE',  ( 0.3024135303179589229, 0.9531768234071938961, 0.000000000000000000 ) ) ;
#46313 = CARTESIAN_POINT ( 'NONE',  ( -72.63029377766190464, -299.5091890795721383, -203.4899686540603057 ) ) ;
#46314 =( BOUNDED_CURVE ( )  B_SPLINE_CURVE ( 3, ( #93670, #28829, #57712, #21727 ),
 .UNSPECIFIED., .F., .F. ) 
 B_SPLINE_CURVE_WITH_KNOTS ( ( 4, 4 ),
 ( 1.570796326794896558, 3.141592653589793116 ),
 .UNSPECIFIED. ) 
 CURVE ( )  GEOMETRIC_REPRESENTATION_ITEM ( )  RATIONAL_B_SPLINE_CURVE ( ( 1.000000000000000000, 0.8047378541243649375, 0.8047378541243649375, 1.000000000000000000 ) ) 
 REPRESENTATION_ITEM ( '' )  );
#46315 = CARTESIAN_POINT ( 'NONE',  ( 37.70371272009514740, -279.5648804318485077, -271.3652785254038804 ) ) ;
#46316 = CARTESIAN_POINT ( 'NONE',  ( -11.19855715296629661, -291.5813785442620656, -198.0508182402863326 ) ) ;
#46317 = CARTESIAN_POINT ( 'NONE',  ( -111.1741663943203662, -294.9737602023050158, -268.6947196850270529 ) ) ;
#46318 = CARTESIAN_POINT ( 'NONE',  ( 32.45017119036801745, -279.9314194999859069, -247.1715353946632092 ) ) ;
#46319 = CARTESIAN_POINT ( 'NONE',  ( 12.52903630444056304, -272.8329343424976514, -215.0266566773978241 ) ) ;
#46320 = CARTESIAN_POINT ( 'NONE',  ( -95.98780272191407903, -297.2490271468528817, -314.6749368759372487 ) ) ;
#46321 = CARTESIAN_POINT ( 'NONE',  ( 205.7381008070598227, 0.000000000000000000, 7.000000000000000000 ) ) ;
#46322 = CARTESIAN_POINT ( 'NONE',  ( 7.501621120913360308, -297.0838201114648882, -194.0657894636586036 ) ) ;
#46323 = CARTESIAN_POINT ( 'NONE',  ( 20.58048956254331685, -292.4638758398115215, -319.5443870633923211 ) ) ;
#46324 = EDGE_CURVE ( 'NONE', #3893, #48610, #16375, .T. ) ;
#46325 = CARTESIAN_POINT ( 'NONE',  ( -70.50235700857385268, -293.0313014536339438, -204.6667821989525464 ) ) ;
#46326 = CARTESIAN_POINT ( 'NONE',  ( 129.9467878515196162, -299.5541904835127980, -195.3611179825600175 ) ) ;
#46327 = CARTESIAN_POINT ( 'NONE',  ( 34.48485135541626079, -294.5381067991047530, -284.2732791867372271 ) ) ;
#46328 = FACE_BOUND ( 'NONE', #79109, .T. ) ;
#46330 = CARTESIAN_POINT ( 'NONE',  ( -45.09073446984387346, -295.1528744107228022, -342.9991450440437575 ) ) ;
#46329 = CARTESIAN_POINT ( 'NONE',  ( -41.50405241988473648, -281.1243016670110819, -345.6524856356463715 ) ) ;
#46331 = CARTESIAN_POINT ( 'NONE',  ( -34.47897102602613728, -283.0170992835729749, -347.3078838800832386 ) ) ;
#46332 = CARTESIAN_POINT ( 'NONE',  ( 38.19992841572207709, -283.4306793522565613, -267.0947722615724729 ) ) ;
#46333 = CARTESIAN_POINT ( 'NONE',  ( 1.514672317913646982, -286.2233352209967165, -203.8933446736745339 ) ) ;
#46334 = CARTESIAN_POINT ( 'NONE',  ( -108.7434333408032501, -288.8421187522321247, -247.9166387788759494 ) ) ;
#46335 = CARTESIAN_POINT ( 'NONE',  ( 157.7374095173865385, -21.37379927922774314, 10.00000000000000000 ) ) ;
#46336 = CARTESIAN_POINT ( 'NONE',  ( 39.01674746887911738, -280.0268864339724360, -269.9534690223280222 ) ) ;
#46337 = CARTESIAN_POINT ( 'NONE',  ( 38.25450449644097972, -286.3093869475776501, -257.3723007814103312 ) ) ;
#46338 = DIRECTION ( 'NONE',  ( 0.09665007798479340051, -0.000000000000000000, 0.9953184226294283787 ) ) ;
#46339 = CARTESIAN_POINT ( 'NONE',  ( -41.05935858943956873, -296.6998137170402288, -344.0801283360063394 ) ) ;
#46340 = CARTESIAN_POINT ( 'NONE',  ( 35.93361755758476761, -277.2518259647716832, -292.0714397965968487 ) ) ;
#46342 = CARTESIAN_POINT ( 'NONE',  ( -38.34988255329290752, -279.7058919817886817, -197.3345298516230173 ) ) ;
#46341 = CARTESIAN_POINT ( 'NONE',  ( 37.59338493961973171, -291.4645839810127654, -261.9354214932698142 ) ) ;
#46343 = CARTESIAN_POINT ( 'NONE',  ( 39.71161926582044543, -293.7181655676005789, -270.3078399084605508 ) ) ;
#46344 = CARTESIAN_POINT ( 'NONE',  ( -107.6788896007015097, -282.9902236642016078, -242.6147070906043837 ) ) ;
#46345 = ADVANCED_FACE ( 'NONE', ( #54410 ), #18912, .T. ) ;
#46346 = CARTESIAN_POINT ( 'NONE',  ( -103.2067127041706698, -280.0757008774535848, -306.2331232843191628 ) ) ;
#46347 = CARTESIAN_POINT ( 'NONE',  ( 17.24798155832381852, -293.3072305702777953, -319.1998442266411189 ) ) ;
#46348 = CARTESIAN_POINT ( 'NONE',  ( -35.50665490957358372, -296.0749665335084728, -195.3617348925761235 ) ) ;
#46349 = ORIENTED_EDGE ( 'NONE', *, *, #23350, .F. ) ;
#46350 = DIRECTION ( 'NONE',  ( 0.000000000000000000, 0.000000000000000000, -1.000000000000000000 ) ) ;
#46351 = CARTESIAN_POINT ( 'NONE',  ( -57.58291125297170510, -281.7694366269533361, -198.5130827124814914 ) ) ;
#46352 = CARTESIAN_POINT ( 'NONE',  ( 34.27805597506248603, -292.8694372884131099, -255.9181619983269513 ) ) ;
#46353 = DIRECTION ( 'NONE',  ( -0.000000000000000000, -0.000000000000000000, 1.000000000000000000 ) ) ;
#46354 = CARTESIAN_POINT ( 'NONE',  ( -53.28691492658257545, -295.3380690714490129, -200.3538533559491555 ) ) ;
#46355 = CARTESIAN_POINT ( 'NONE',  ( -112.2835255618849999, -271.9619667686486650, -253.3940433356491440 ) ) ;
#46356 = CARTESIAN_POINT ( 'NONE',  ( 35.91804928170274991, -289.1464020034975420, -292.4590311703821044 ) ) ;
#46357 = CARTESIAN_POINT ( 'NONE',  ( 7.978283973949081620, -288.2458957510714299, -327.5895990516440861 ) ) ;
#46358 = CARTESIAN_POINT ( 'NONE',  ( -88.02135643986768798, -280.8481165182821542, -216.7902964030737394 ) ) ;
#46359 = CARTESIAN_POINT ( 'NONE',  ( -95.25809100411727570, -298.9541240556448543, -224.2778706503605690 ) ) ;
#46360 = CARTESIAN_POINT ( 'NONE',  ( -59.84083681738145799, -278.5491162600953317, -200.4439503244655612 ) ) ;
#46361 = ORIENTED_EDGE ( 'NONE', *, *, #31125, .T. ) ;
#46362 = CARTESIAN_POINT ( 'NONE',  ( 30.76934322675772293, -298.5497918239036039, -193.3859609996251265 ) ) ;
#46363 = CARTESIAN_POINT ( 'NONE',  ( -11.78841591291329749, -294.3074546909768401, -200.3894926422692606 ) ) ;
#46364 = CARTESIAN_POINT ( 'NONE',  ( 32.68947203243885724, -295.5403470442806224, -300.5290273544906654 ) ) ;
#46365 = DIRECTION ( 'NONE',  ( 0.000000000000000000, 0.000000000000000000, -1.000000000000000000 ) ) ;
#46366 = CARTESIAN_POINT ( 'NONE',  ( -110.4077740675563177, -291.1566586507199759, -273.9221826773558064 ) ) ;
#46367 = CARTESIAN_POINT ( 'NONE',  ( 157.3400606585842354, 276.0000000000001137, 16.90038786543334126 ) ) ;
#46368 = CARTESIAN_POINT ( 'NONE',  ( 31.08082618801976338, -291.2665010447502141, -237.7020057178556840 ) ) ;
#46369 = CARTESIAN_POINT ( 'NONE',  ( -99.91272315313989338, -296.7378393500935658, -232.6203390726961118 ) ) ;
#46370 = CARTESIAN_POINT ( 'NONE',  ( 196.3496553477289979, 250.0000000000000568, -12.41762739670150850 ) ) ;
#46371 = CARTESIAN_POINT ( 'NONE',  ( 196.0583257291930295, 24.84528228517684667, 13.82746528162204491 ) ) ;
#46372 = CARTESIAN_POINT ( 'NONE',  ( -110.1147047664034773, -291.7792450655117023, -293.4856677743620708 ) ) ;
#46373 = CARTESIAN_POINT ( 'NONE',  ( 40.65961533371913106, -296.2662352645559167, -288.1317622949166548 ) ) ;
#46374 = CARTESIAN_POINT ( 'NONE',  ( 20.05185306690983182, -288.8871543897271863, -222.3202461236955685 ) ) ;
#46375 = CARTESIAN_POINT ( 'NONE',  ( 16.79014183914382841, -272.8242979144181959, -218.6162415006879769 ) ) ;
#46376 = CARTESIAN_POINT ( 'NONE',  ( 35.30383162187533941, -277.6832253726983026, -286.6654224065933931 ) ) ;
#46377 = CARTESIAN_POINT ( 'NONE',  ( -44.41312411285835537, -290.0419883669500223, -196.2059303815636326 ) ) ;
#46378 = CARTESIAN_POINT ( 'NONE',  ( -35.39194776999691783, -281.9367581745924554, -194.6084798188588536 ) ) ;
#46379 = ORIENTED_EDGE ( 'NONE', *, *, #29058, .T. ) ;
#46380 = CARTESIAN_POINT ( 'NONE',  ( 3.440218207359738045, -281.8366552454165230, -331.0913462205418796 ) ) ;
#46381 = CARTESIAN_POINT ( 'NONE',  ( -109.3208575026317391, -279.9693989404456147, -243.7408889201573174 ) ) ;
#46382 = CARTESIAN_POINT ( 'NONE',  ( 37.15858708771732211, -280.5718154017666848, -288.2416088204408879 ) ) ;
#46383 = CARTESIAN_POINT ( 'NONE',  ( -32.29525589772949701, -123.9253558744183010, -361.4536083058858935 ) ) ;
#46384 = CARTESIAN_POINT ( 'NONE',  ( 13.79876679911920156, -275.6895075074633041, -213.0408770695811711 ) ) ;
#46385 = ADVANCED_FACE ( 'NONE', ( #46823 ), #68182, .T. ) ;
#46386 = PRODUCT_CONTEXT ( 'NONE', #31747, 'mechanical' ) ;
#46387 = CARTESIAN_POINT ( 'NONE',  ( 21.30545371755189876, -276.4096568132458174, -221.5428928950725833 ) ) ;
#46388 = CARTESIAN_POINT ( 'NONE',  ( -110.4542110544635705, -298.8376638359844719, -287.0812184334320705 ) ) ;
#46389 = EDGE_LOOP ( 'NONE', ( #67050, #57249, #40443, #93009 ) ) ;
#46390 = ORIENTED_EDGE ( 'NONE', *, *, #62476, .F. ) ;
#46391 = DIRECTION ( 'NONE',  ( -0.000000000000000000, -1.000000000000000000, -0.000000000000000000 ) ) ;
#46392 = CARTESIAN_POINT ( 'NONE',  ( -106.3187866098970176, -291.3025600349148476, -295.1882727475874049 ) ) ;
#46393 = CARTESIAN_POINT ( 'NONE',  ( -88.78872062443217317, -291.5230351917008420, -326.2822954904153789 ) ) ;
#46394 = CARTESIAN_POINT ( 'NONE',  ( -22.71213192228901079, -291.5929570822947312, -198.7380183432076990 ) ) ;
#46395 = CARTESIAN_POINT ( 'NONE',  ( 1.496033748994984425, -286.0642948689919649, -203.9292471266118696 ) ) ;
#46396 = CARTESIAN_POINT ( 'NONE',  ( 150.6539576904058606, 293.9636489450775230, 0.000000000000000000 ) ) ;
#46397 = CARTESIAN_POINT ( 'NONE',  ( -4.489142514825396724, -281.0116512783066014, -336.4455327542974601 ) ) ;
#46398 = CARTESIAN_POINT ( 'NONE',  ( 36.91527576519431619, -289.3852435326124350, -268.2541570470018542 ) ) ;
#46399 = CARTESIAN_POINT ( 'NONE',  ( 19.87824628872928656, -280.6831573958477861, -316.8200539764588370 ) ) ;
#46400 = CARTESIAN_POINT ( 'NONE',  ( 35.04998085649585704, -282.7012311139661165, -257.6848408079382580 ) ) ;
#46401 = CARTESIAN_POINT ( 'NONE',  ( 35.72747335436562111, -288.7902196797586498, -293.8922909122684359 ) ) ;
#46402 = CARTESIAN_POINT ( 'NONE',  ( -107.6792578609853877, -279.3060782671766447, -250.5507162075596455 ) ) ;
#46403 = CARTESIAN_POINT ( 'NONE',  ( -108.4356802373065420, -288.9832073504236973, -298.8857513700295385 ) ) ;
#46404 = CARTESIAN_POINT ( 'NONE',  ( -95.70063300322010491, -286.0315078299092875, -220.2973688517673168 ) ) ;
#46405 = CARTESIAN_POINT ( 'NONE',  ( 16.25182647336717068, -287.2810180583446140, -215.1591179323358460 ) ) ;
#46406 = CARTESIAN_POINT ( 'NONE',  ( -105.2131509675829903, -284.3576376503070264, -297.3774390006513499 ) ) ;
#46407 = ORIENTED_EDGE ( 'NONE', *, *, #17135, .F. ) ;
#46408 = DIRECTION ( 'NONE',  ( 0.000000000000000000, 0.000000000000000000, 1.000000000000000000 ) ) ;
#46409 = CARTESIAN_POINT ( 'NONE',  ( 32.18141296128852957, -295.0225519098081577, -240.2472968312838759 ) ) ;
#46410 = CARTESIAN_POINT ( 'NONE',  ( 38.95056213539505308, -292.1649048759869061, -264.6349508133022823 ) ) ;
#46411 = CARTESIAN_POINT ( 'NONE',  ( -3.770250696512623456, -275.6565233490712217, -335.4484918104378721 ) ) ;
#46412 = CARTESIAN_POINT ( 'NONE',  ( -41.94775898574346229, -294.4572157296943828, -347.1734380241659323 ) ) ;
#46413 = CARTESIAN_POINT ( 'NONE',  ( -70.51565781845140179, -290.0863837760697947, -204.5568910248455836 ) ) ;
#46414 = CARTESIAN_POINT ( 'NONE',  ( 8.843250423906901858, -292.6490410919157057, -328.2622899375991778 ) ) ;
#46415 = CARTESIAN_POINT ( 'NONE',  ( -102.7704557630788145, -292.2078339740842239, -236.9888535220450478 ) ) ;
#46416 = CARTESIAN_POINT ( 'NONE',  ( -3.505758968497529438, -293.5895482063708073, -205.3276253788006613 ) ) ;
#46417 = CARTESIAN_POINT ( 'NONE',  ( 209.2038787506929793, 35.78193936320073476, 14.26380413240767098 ) ) ;
#46418 = CARTESIAN_POINT ( 'NONE',  ( -41.86140837607259613, -293.1086862304427996, -345.4429281183137164 ) ) ;
#46419 = CARTESIAN_POINT ( 'NONE',  ( -44.00562195928616660, -299.9681931489901103, -195.6069440379329762 ) ) ;
#46420 = CARTESIAN_POINT ( 'NONE',  ( -3.246179430729769333, -289.5318387246890666, -335.2316691412055434 ) ) ;
#46421 = CARTESIAN_POINT ( 'NONE',  ( 24.72674802516062442, -278.1094940323442870, -313.1821945748203007 ) ) ;
#46422 = CARTESIAN_POINT ( 'NONE',  ( -109.3686879415191555, -277.0142365354618619, -296.5955206070291297 ) ) ;
#46423 = CARTESIAN_POINT ( 'NONE',  ( -87.96302347577335468, -272.7147809255042148, -212.4042825872313927 ) ) ;
#46424 = CARTESIAN_POINT ( 'NONE',  ( 30.29103816560489193, -279.2191305179655956, -239.1388334326545362 ) ) ;
#46425 = CARTESIAN_POINT ( 'NONE',  ( -77.41173809772131165, -275.9796151952839409, -335.2362731638159516 ) ) ;
#46426 = CARTESIAN_POINT ( 'NONE',  ( -93.46979529053184876, -294.5670767082834232, -317.8240637294426847 ) ) ;
#46427 = CARTESIAN_POINT ( 'NONE',  ( -68.51488237780591817, -275.6427384623713124, -202.1326231451482442 ) ) ;
#46428 = CARTESIAN_POINT ( 'NONE',  ( -37.83384158578008538, -298.8486663569955795, -197.2012961926343451 ) ) ;
#46429 = CARTESIAN_POINT ( 'NONE',  ( 196.7383257810085695, 24.47698789593438917, 11.00000000000000355 ) ) ;
#46431 = CARTESIAN_POINT ( 'NONE',  ( 17.28696614175932567, -274.6928676796962918, -221.8640199470314940 ) ) ;
#46430 = CARTESIAN_POINT ( 'NONE',  ( -86.33460885551939157, -287.7478770723640764, -327.6843844502901106 ) ) ;
#46432 = CARTESIAN_POINT ( 'NONE',  ( 18.64481637960401983, -288.2740710177165511, -323.2242428366080276 ) ) ;
#46433 = CARTESIAN_POINT ( 'NONE',  ( -59.68497609087143019, -299.7441908903262515, -198.3402217715505174 ) ) ;
#46434 = CARTESIAN_POINT ( 'NONE',  ( -112.0738212627230439, -294.5019180846687732, -274.2519398153865495 ) ) ;
#46435 = CARTESIAN_POINT ( 'NONE',  ( 9.103058559264185945, -281.6296965013964382, -331.5742147060465186 ) ) ;
#46436 = FACE_OUTER_BOUND ( 'NONE', #59367, .T. ) ;
#46437 = CARTESIAN_POINT ( 'NONE',  ( -8.292988324166739034, -280.6716752413627773, -339.5209101439962183 ) ) ;
#46438 = CARTESIAN_POINT ( 'NONE',  ( 200.5336405603944456, 288.1658739788085200, -5.513969000952395838 ) ) ;
#46439 = CARTESIAN_POINT ( 'NONE',  ( -93.73512308261878445, -290.0101967664827498, -223.3637169999577736 ) ) ;
#46440 = EDGE_CURVE ( 'NONE', #443, #28384, #87435, .T. ) ;
#46441 = CARTESIAN_POINT ( 'NONE',  ( -108.5838958349923757, -282.4197322264703303, -291.2731555933654590 ) ) ;
#46442 = DIRECTION ( 'NONE',  ( 0.000000000000000000, 0.000000000000000000, -1.000000000000000000 ) ) ;
#46443 = DIRECTION ( 'NONE',  ( 0.000000000000000000, 0.000000000000000000, 1.000000000000000000 ) ) ;
#46444 = CARTESIAN_POINT ( 'NONE',  ( -109.3073868082940123, -288.8244599757809965, -249.1982652254150423 ) ) ;
#46445 = CARTESIAN_POINT ( 'NONE',  ( -0.2135237236779599368, -276.0756970226396447, -206.6894484954567588 ) ) ;
#46446 = CARTESIAN_POINT ( 'NONE',  ( 11.13291786550620621, -283.8215966836567645, -329.4958146255698921 ) ) ;
#46448 = CARTESIAN_POINT ( 'NONE',  ( -37.54052282974512877, -283.0547449011847903, -343.3732765808597946 ) ) ;
#46447 = CARTESIAN_POINT ( 'NONE',  ( -93.99037616140643081, -271.3220131083025990, -220.3587010078310300 ) ) ;
#46449 = CARTESIAN_POINT ( 'NONE',  ( 35.42156444521238967, -276.8324453484163996, -259.2818236959449223 ) ) ;
#46450 = CARTESIAN_POINT ( 'NONE',  ( 35.80413762342946882, -276.3350792790271271, -268.8484560705453532 ) ) ;
#46451 = EDGE_CURVE ( 'NONE', #17445, #36646, #79889, .T. ) ;
#46452 = CARTESIAN_POINT ( 'NONE',  ( -64.50349158034769914, -285.4068306240286574, -340.2837322389356700 ) ) ;
#46453 = ORIENTED_EDGE ( 'NONE', *, *, #7541, .T. ) ;
#46454 = CARTESIAN_POINT ( 'NONE',  ( 204.7719119196574411, 293.0780843197346144, -54.00000000000338929 ) ) ;
#46455 = CARTESIAN_POINT ( 'NONE',  ( 1.767606473776451192, -294.3774121009295754, -336.6895594057350536 ) ) ;
#46456 = CARTESIAN_POINT ( 'NONE',  ( -41.43784094566748877, -287.9802400865987693, -195.8160067305347525 ) ) ;
#46457 = CARTESIAN_POINT ( 'NONE',  ( -23.68628624284178130, -43.55766379199612004, -21.50000000000000000 ) ) ;
#46458 = CARTESIAN_POINT ( 'NONE',  ( -19.05039376806006857, -283.7666405000204009, -190.3683826091709363 ) ) ;
#46459 = CARTESIAN_POINT ( 'NONE',  ( -67.65433532881492340, -276.6370755009165237, -340.9677959104295155 ) ) ;
#46460 = CARTESIAN_POINT ( 'NONE',  ( -64.08870748035188569, -290.1090029215429240, -198.9540250563174766 ) ) ;
#46461 = CARTESIAN_POINT ( 'NONE',  ( -54.94050206904025657, -287.3420280703763297, -198.7472279257920604 ) ) ;
#46462 = CARTESIAN_POINT ( 'NONE',  ( -76.87844364834829491, -279.3492813123046403, -332.9899053948845449 ) ) ;
#46463 = CARTESIAN_POINT ( 'NONE',  ( -70.82453441366230606, -287.0443459470996004, -201.6770142629244731 ) ) ;
#46464 = CARTESIAN_POINT ( 'NONE',  ( 6.788913995194937989, -284.4519230579898021, -331.0034261761716721 ) ) ;
#46465 = CARTESIAN_POINT ( 'NONE',  ( 39.63080533149643969, -275.6930996702062657, -268.3035933143937655 ) ) ;
#46466 = CARTESIAN_POINT ( 'NONE',  ( -34.29321983966458021, -276.8481353538730900, -347.3007486838610589 ) ) ;
#46467 = CARTESIAN_POINT ( 'NONE',  ( -103.8292990821091593, -298.9192201444915895, -236.7692148447806915 ) ) ;
#46468 = CARTESIAN_POINT ( 'NONE',  ( 185.8632872119974024, 215.0000000000001705, 23.14243616685787330 ) ) ;
#46469 = CYLINDRICAL_SURFACE ( 'NONE', #17843, 1.000000000000000888 ) ;
#46470 = CARTESIAN_POINT ( 'NONE',  ( -57.04528014716949258, -295.9403570344323953, -197.1488575668585952 ) ) ;
#46471 = DIRECTION ( 'NONE',  ( -1.000000000000000000, 0.000000000000000000, 0.000000000000000000 ) ) ;
#46472 = CARTESIAN_POINT ( 'NONE',  ( -110.3418825866378654, -278.0203441884185054, -273.3547449623461603 ) ) ;
#46473 = CARTESIAN_POINT ( 'NONE',  ( 4.632690563354548097, -275.8098827084253912, -206.2188701014767105 ) ) ;
#46474 = CARTESIAN_POINT ( 'NONE',  ( 37.75698957542275025, -280.4105768394371125, -254.3919926805629075 ) ) ;
#46475 = CARTESIAN_POINT ( 'NONE',  ( -6.616002688921249764, -288.2213426497713726, -203.0129209775155630 ) ) ;
#46476 = CARTESIAN_POINT ( 'NONE',  ( -113.6721291979071111, -298.0456576170525409, -272.4701219602595756 ) ) ;
#46477 = CARTESIAN_POINT ( 'NONE',  ( -64.11296887098848174, -296.5988460454856863, -342.1337303653332924 ) ) ;
#46478 = B_SPLINE_CURVE_WITH_KNOTS ( 'NONE', 3,
 ( #5872, #34741, #26230, #76435, #92480, #4450 ),
 .UNSPECIFIED., .F., .F.,
 ( 4, 2, 4 ),
 ( 0.000000000000000000, 0.0006327419528623999100, 0.001265483905724799820 ),
 .UNSPECIFIED. ) ;
#46479 = CARTESIAN_POINT ( 'NONE',  ( 24.07845450243603125, -294.9707634450836053, -227.5881933692811856 ) ) ;
#46480 = CARTESIAN_POINT ( 'NONE',  ( -41.11887304149887967, -278.0043305840779908, -195.6231664915185604 ) ) ;
#46481 = CARTESIAN_POINT ( 'NONE',  ( -2.496257393005111069, -282.4369078404466791, -204.5658955737301881 ) ) ;
#46482 = CARTESIAN_POINT ( 'NONE',  ( -108.8357003007970292, -294.9009456538357767, -249.6265541226763105 ) ) ;
#46483 = CARTESIAN_POINT ( 'NONE',  ( -102.2260972412861690, -285.6245452182780582, -310.3167862361407288 ) ) ;
#46484 = CARTESIAN_POINT ( 'NONE',  ( 19.76461015206173144, -285.8251067063666255, -224.3728071224861367 ) ) ;
#46485 = CARTESIAN_POINT ( 'NONE',  ( 1.329898937396618352, -279.9027848580465729, -203.8338049045802052 ) ) ;
#46486 = CARTESIAN_POINT ( 'NONE',  ( -61.77620294925019806, -183.7782069458722845, -361.8444782285974384 ) ) ;
#46487 = EDGE_LOOP ( 'NONE', ( #54772, #41262, #40833, #80201, #40914, #57131, #92186 ) ) ;
#46488 = CARTESIAN_POINT ( 'NONE',  ( -14.55537852441836044, -286.0223818072741437, -200.9332241126281815 ) ) ;
#46489 = VERTEX_POINT ( 'NONE', #83582 ) ;
#46490 = CARTESIAN_POINT ( 'NONE',  ( -34.47669755257052060, -284.0965961714980494, -346.9984735655148143 ) ) ;
#46491 = CARTESIAN_POINT ( 'NONE',  ( 34.72872807739076961, -276.0443542757327009, -282.4115702967845891 ) ) ;
#46492 = CARTESIAN_POINT ( 'NONE',  ( 26.03751117941197180, -285.7766374851220803, -227.3134500792251060 ) ) ;
#46493 = CARTESIAN_POINT ( 'NONE',  ( -81.74019806730593984, -290.3833181852807570, -207.8289991177871059 ) ) ;
#46494 = CARTESIAN_POINT ( 'NONE',  ( 35.94749142148326371, -282.2056294564739005, -247.5244234982417026 ) ) ;
#46495 = FACE_OUTER_BOUND ( 'NONE', #3300, .T. ) ;
#46496 = CARTESIAN_POINT ( 'NONE',  ( -14.45433086940533407, -281.8635802459497768, -197.5123465187869272 ) ) ;
#46497 = CARTESIAN_POINT ( 'NONE',  ( 34.30318578081588754, -281.5267522505560009, -242.0597524498827795 ) ) ;
#46498 = CARTESIAN_POINT ( 'NONE',  ( -105.5937364680635966, -281.8380690714489560, -285.9065529553535612 ) ) ;
#46499 = CARTESIAN_POINT ( 'NONE',  ( -47.47154897853537392, -155.3119904466320804, -365.2842717752373574 ) ) ;
#46500 = ORIENTED_EDGE ( 'NONE', *, *, #61310, .F. ) ;
#46501 = CARTESIAN_POINT ( 'NONE',  ( 35.02136117726902853, -277.7979341047210369, -289.4298302571585850 ) ) ;
#46502 = CARTESIAN_POINT ( 'NONE',  ( 188.7542133104363415, 271.4570962582653806, -139.3427320832213638 ) ) ;
#46503 = CARTESIAN_POINT ( 'NONE',  ( 37.20737500415631160, -279.6210096644622354, -274.1402973787165251 ) ) ;
#46504 = CARTESIAN_POINT ( 'NONE',  ( -81.99984057473265864, -296.7738103376374283, -212.4217306007535342 ) ) ;
#46505 = CARTESIAN_POINT ( 'NONE',  ( -79.55540984551448958, -291.0063263815785035, -205.9738042515697600 ) ) ;
#46506 = CARTESIAN_POINT ( 'NONE',  ( 159.6810783670777880, 8.542400036368780647, 9.000000000000001776 ) ) ;
#46507 = EDGE_CURVE ( 'NONE', #25512, #48026, #29489, .T. ) ;
#46509 = CARTESIAN_POINT ( 'NONE',  ( 20.15111980897052035, -285.3047340312012352, -224.0699744219512866 ) ) ;
#46508 = CARTESIAN_POINT ( 'NONE',  ( -80.27880545019738179, -296.0581093270862425, -207.0914089845376509 ) ) ;
#46510 = CARTESIAN_POINT ( 'NONE',  ( 34.31511994998453474, -295.6650723877946234, -289.8044982718808456 ) ) ;
#46511 = EDGE_CURVE ( 'NONE', #21957, #78913, #27248, .T. ) ;
#46512 = CARTESIAN_POINT ( 'NONE',  ( 9.330855014310634132, -288.0245267162670189, -213.5903854431656157 ) ) ;
#46513 = ORIENTED_EDGE ( 'NONE', *, *, #72006, .T. ) ;
#46514 = CARTESIAN_POINT ( 'NONE',  ( 37.23428988671186346, -294.7223839500972531, -288.6162091161399417 ) ) ;
#46515 = CARTESIAN_POINT ( 'NONE',  ( -106.5926498419017463, -285.3554628579443033, -246.9154461683848467 ) ) ;
#46516 = CARTESIAN_POINT ( 'NONE',  ( -103.4990952029686753, -295.8533586527062198, -231.6404577125566391 ) ) ;
#46517 = CARTESIAN_POINT ( 'NONE',  ( -8.581166271665804146, -293.2219674376185026, -199.1081144466369039 ) ) ;
#46518 = CARTESIAN_POINT ( 'NONE',  ( -34.96859767793201001, -292.5735202635398764, -193.4461234652441135 ) ) ;
#46519 = CARTESIAN_POINT ( 'NONE',  ( -13.28587243346614066, -288.8974840554821526, -339.2836626136479481 ) ) ;
#46520 = ORIENTED_EDGE ( 'NONE', *, *, #74502, .T. ) ;
#46521 = CARTESIAN_POINT ( 'NONE',  ( 140.0681712527789671, 131.0000000000000568, -11.49999999999999822 ) ) ;
#46522 = CARTESIAN_POINT ( 'NONE',  ( -9.696521646170193520, -300.2551450493016318, -194.5876580512280327 ) ) ;
#46523 = CARTESIAN_POINT ( 'NONE',  ( -106.4782272792930655, -271.7721689242761158, -237.3740094259029547 ) ) ;
#46524 = CARTESIAN_POINT ( 'NONE',  ( -32.14091564159048175, -282.0436832783194632, -343.4115135259049225 ) ) ;
#46525 = ORIENTED_EDGE ( 'NONE', *, *, #52600, .T. ) ;
#46526 = CARTESIAN_POINT ( 'NONE',  ( -34.29980923948419047, -276.5225208320015327, -347.2394231356013279 ) ) ;
#46527 = CARTESIAN_POINT ( 'NONE',  ( -91.69812366915154200, -271.6608971428851191, -220.4242877252961819 ) ) ;
#46528 = CARTESIAN_POINT ( 'NONE',  ( -107.6216710325976607, -280.7268517594920354, -246.2951353709926821 ) ) ;
#46529 = CARTESIAN_POINT ( 'NONE',  ( 32.41443528281216402, -274.0262437218823379, -295.9061690981015431 ) ) ;
#46530 = CARTESIAN_POINT ( 'NONE',  ( -69.44499153016444382, -298.8249977409690814, -204.3572606151357149 ) ) ;
#46531 = CARTESIAN_POINT ( 'NONE',  ( -39.18984574589416070, -299.1081261503075552, -197.0628434366063004 ) ) ;
#46532 = CARTESIAN_POINT ( 'NONE',  ( -112.1077475633819205, -298.3390650588717676, -255.5807153435105761 ) ) ;
#46533 = CARTESIAN_POINT ( 'NONE',  ( -29.97406864047778541, -272.1650794284279300, -195.3669528197211775 ) ) ;
#46534 = CARTESIAN_POINT ( 'NONE',  ( 1.631185191535880374, -295.1677828401715828, -332.2677131690297756 ) ) ;
#46535 = CARTESIAN_POINT ( 'NONE',  ( -60.42672580765761126, -290.3216947233413521, -200.4330781412546685 ) ) ;
#46536 = DIRECTION ( 'NONE',  ( -1.000000000000000000, -0.000000000000000000, -0.000000000000000000 ) ) ;
#46537 = CARTESIAN_POINT ( 'NONE',  ( 11.74160832447875613, -275.2047662835769870, -211.0436376925225090 ) ) ;
#46538 = CARTESIAN_POINT ( 'NONE',  ( -110.3417001280813707, -272.7188053858000671, -270.3632352445363267 ) ) ;
#46539 = CARTESIAN_POINT ( 'NONE',  ( 30.63128665182165022, -280.6925371517787084, -305.4748096095851793 ) ) ;
#46540 = FACE_OUTER_BOUND ( 'NONE', #49916, .T. ) ;
#46541 = CARTESIAN_POINT ( 'NONE',  ( -87.04602165081868748, -282.9625272965397471, -324.1154638808611708 ) ) ;
#46542 = CARTESIAN_POINT ( 'NONE',  ( -35.95908338051339825, -281.0347259743611517, -345.5278769504558909 ) ) ;
#46543 = CARTESIAN_POINT ( 'NONE',  ( -9.784421121998015280, -275.2597489329264135, -338.6094696337240180 ) ) ;
#46544 = CARTESIAN_POINT ( 'NONE',  ( 24.52240164543244560, -284.1277778642296425, -312.8511540795840347 ) ) ;
#46545 = EDGE_CURVE ( 'NONE', #3069, #25728, #56134, .T. ) ;
#46546 = FACE_OUTER_BOUND ( 'NONE', #57060, .T. ) ;
#46547 = CIRCLE ( 'NONE', #25399, 9.103929867429224387 ) ;
#46548 = FACE_OUTER_BOUND ( 'NONE', #93012, .T. ) ;
#46549 = CARTESIAN_POINT ( 'NONE',  ( -64.59472941738422946, -272.1021126672830519, -199.1873117509834685 ) ) ;
#46550 = CARTESIAN_POINT ( 'NONE',  ( -112.2497287703827169, -280.4648215103738380, -277.1904708549156453 ) ) ;
#46551 = DIRECTION ( 'NONE',  ( 1.000000000000000000, 0.000000000000000000, 0.000000000000000000 ) ) ;
#46552 = CARTESIAN_POINT ( 'NONE',  ( -98.60628917152341444, -285.8736722264678178, -314.6748056152290474 ) ) ;
#46553 = ORIENTED_EDGE ( 'NONE', *, *, #13732, .T. ) ;
#46554 = CARTESIAN_POINT ( 'NONE',  ( 202.6531192844960287, 63.25403289339011081, 9.673168394419587202 ) ) ;
#46555 = CARTESIAN_POINT ( 'NONE',  ( -90.35999277721030865, -287.8018218744213641, -323.4812491160253103 ) ) ;
#46556 = DIRECTION ( 'NONE',  ( -1.000000000000000000, 0.000000000000000000, 0.000000000000000000 ) ) ;
#46557 = CARTESIAN_POINT ( 'NONE',  ( -88.79107481039878280, -294.5888948618323866, -322.7784501479519008 ) ) ;
#46558 = CARTESIAN_POINT ( 'NONE',  ( -87.58248017972501032, -287.9015490681890697, -325.0818535784466121 ) ) ;
#46559 = CARTESIAN_POINT ( 'NONE',  ( -99.29329069375972949, -236.7418906163237580, -339.9611904871904358 ) ) ;
#46560 = CARTESIAN_POINT ( 'NONE',  ( -112.0948556754403427, -294.4660598399690343, -277.0534350092479485 ) ) ;
#46561 = CARTESIAN_POINT ( 'NONE',  ( 38.39989222181901596, -286.1543634083397478, -280.0544876338055360 ) ) ;
#46562 = CARTESIAN_POINT ( 'NONE',  ( 36.22828717972275570, -283.2363178523491456, -276.8008891564444411 ) ) ;
#46563 = CARTESIAN_POINT ( 'NONE',  ( -3.366303541904547725, -280.8496913973339133, -338.3435576598768080 ) ) ;
#46564 = CARTESIAN_POINT ( 'NONE',  ( 12.15580102355880854, -288.3406755816164377, -324.0860959863687185 ) ) ;
#46565 = CARTESIAN_POINT ( 'NONE',  ( 30.88757684273510407, -283.3436705467093475, -297.9317668663750851 ) ) ;
#46566 = CARTESIAN_POINT ( 'NONE',  ( 28.30045861956977404, -282.7931657773804091, -302.7826016632959067 ) ) ;
#46567 = CARTESIAN_POINT ( 'NONE',  ( 27.27488020807414415, -289.0142107210244831, -231.4906465224462124 ) ) ;
#46568 = EDGE_CURVE ( 'NONE', #47159, #67960, #77888, .T. ) ;
#46569 = CARTESIAN_POINT ( 'NONE',  ( -30.48671247894817427, -298.3024367115428959, -193.3609299358889473 ) ) ;
#46570 = EDGE_LOOP ( 'NONE', ( #90713, #31389, #31298, #72611, #34299, #85145 ) ) ;
#46571 = CARTESIAN_POINT ( 'NONE',  ( -99.56705243431393626, -273.1551104488721649, -224.9184825532749983 ) ) ;
#46572 = CARTESIAN_POINT ( 'NONE',  ( 7.647966158127728953, -294.6495862211684766, -210.7979017570939959 ) ) ;
#46573 = CARTESIAN_POINT ( 'NONE',  ( 160.5350683151633291, 250.0000000000000568, 20.22542485937379908 ) ) ;
#46574 = CARTESIAN_POINT ( 'NONE',  ( -106.6662871844225293, -281.4805209788417528, -237.0123917617630980 ) ) ;
#46575 = VERTEX_POINT ( 'NONE', #77435 ) ;
#46576 = CARTESIAN_POINT ( 'NONE',  ( -8.609558829170946836, -274.6768893165237273, -339.8336268800298967 ) ) ;
#46577 = CARTESIAN_POINT ( 'NONE',  ( 197.1577115253454338, 71.52895221111288038, 12.06965615694062244 ) ) ;
#46578 = CARTESIAN_POINT ( 'NONE',  ( -113.5378019297075554, -294.9617684197314702, -269.5900903333194378 ) ) ;
#46579 = CARTESIAN_POINT ( 'NONE',  ( -16.60381347833856225, -273.6757199202681363, -200.2095983897104645 ) ) ;
#46580 = CARTESIAN_POINT ( 'NONE',  ( -75.35367709335112352, -293.0559306613838544, -207.1683618300355079 ) ) ;
#46581 = CARTESIAN_POINT ( 'NONE',  ( -93.62834761314395848, -292.1561772618987902, -223.4883427569804724 ) ) ;
#46582 = CARTESIAN_POINT ( 'NONE',  ( 19.28391228345673625, -283.9802102709580254, -318.0412025849864790 ) ) ;
#46583 = CARTESIAN_POINT ( 'NONE',  ( -113.2261450943129262, -291.8590950070779400, -279.7500239434645550 ) ) ;
#46584 = CARTESIAN_POINT ( 'NONE',  ( -42.04051370237161933, -293.3092564129298694, -193.9986964379793051 ) ) ;
#46585 = CARTESIAN_POINT ( 'NONE',  ( -26.20950126106492561, -294.7397945242577180, -342.5073178330993073 ) ) ;
#46586 = CARTESIAN_POINT ( 'NONE',  ( 21.95394524892376609, -290.1820178921375941, -316.3060666026779018 ) ) ;
#46587 = CARTESIAN_POINT ( 'NONE',  ( 28.30611449797990886, -282.2457496656749640, -310.7034942541572491 ) ) ;
#46588 = CARTESIAN_POINT ( 'NONE',  ( -94.50836201296606021, -293.9518631375467521, -319.7704993705849574 ) ) ;
#46589 = CARTESIAN_POINT ( 'NONE',  ( -31.63840623613665315, -282.8153818476476431, -347.1628775364534363 ) ) ;
#46590 = CARTESIAN_POINT ( 'NONE',  ( 1.753912904981421050, -278.5068207043474899, -334.0094404234041576 ) ) ;
#46591 = CARTESIAN_POINT ( 'NONE',  ( -108.5835401312018291, -276.3590019111426273, -296.3004918719157104 ) ) ;
#46592 = DIRECTION ( 'NONE',  ( 0.9251343685759222391, -0.3490264795282477794, -0.1493550021517442705 ) ) ;
#46593 = CARTESIAN_POINT ( 'NONE',  ( 15.86637979916431362, -281.7807001949903452, -320.5029402491841779 ) ) ;
#46594 = CARTESIAN_POINT ( 'NONE',  ( -41.00483948908105702, -281.2121194942228044, -193.8326971583397835 ) ) ;
#46595 = CARTESIAN_POINT ( 'NONE',  ( 9.676121556389981393, -285.7402886695355733, -209.6804401985278616 ) ) ;
#46596 = CARTESIAN_POINT ( 'NONE',  ( -66.99030088293672236, -293.4182639793105523, -202.5456736602772310 ) ) ;
#46597 = CARTESIAN_POINT ( 'NONE',  ( 37.70066684158338433, -276.9841144675755231, -257.0547561907097815 ) ) ;
#46598 = CARTESIAN_POINT ( 'NONE',  ( 38.23780358342659724, -276.7167789953472834, -258.4008937734320739 ) ) ;
#46599 = CARTESIAN_POINT ( 'NONE',  ( -108.4867444995050931, -278.1690329238269896, -286.7683621450599389 ) ) ;
#46600 = CARTESIAN_POINT ( 'NONE',  ( -111.2142068344568173, -274.6747812398086808, -259.2972781682528876 ) ) ;
#46601 = CARTESIAN_POINT ( 'NONE',  ( 37.43845261011856707, -293.4480569937410905, -288.6829804417172340 ) ) ;
#46602 = CARTESIAN_POINT ( 'NONE',  ( -97.51519561589029195, -291.5213448295623380, -317.1114212866702928 ) ) ;
#46603 = CARTESIAN_POINT ( 'NONE',  ( -14.73808618523979774, -291.2723928470009582, -200.6237341069408728 ) ) ;
#46604 = ORIENTED_EDGE ( 'NONE', *, *, #30011, .T. ) ;
#46605 = CARTESIAN_POINT ( 'NONE',  ( -66.56864206318293498, -291.3251799890189773, -203.4442041867044111 ) ) ;
#46606 = EDGE_LOOP ( 'NONE', ( #9590, #57909, #59135, #56589 ) ) ;
#46607 = CARTESIAN_POINT ( 'NONE',  ( -36.07809076639345847, -290.1163566599614114, -347.0546541457024432 ) ) ;
#46608 = CARTESIAN_POINT ( 'NONE',  ( -39.71283842052467605, -280.6730390831329487, -197.2851126979471132 ) ) ;
#46609 = CARTESIAN_POINT ( 'NONE',  ( -104.9744953429309078, -295.9429009894870433, -234.0919320306861948 ) ) ;
#46610 = CARTESIAN_POINT ( 'NONE',  ( 2.680869986122784265, -287.2255899567784354, -204.6990538363054952 ) ) ;
#46611 = CARTESIAN_POINT ( 'NONE',  ( 33.83825483885439667, -287.5112753461085617, -240.9104792703699616 ) ) ;
#46613 = CARTESIAN_POINT ( 'NONE',  ( -95.93617238407178149, -284.2743898774062359, -313.9360569714524445 ) ) ;
#46612 = AXIS2_PLACEMENT_3D ( 'NONE', #44967, #59689, #3286 ) ;
#46614 = CARTESIAN_POINT ( 'NONE',  ( -56.47922461787481296, -169.2600705521303155, -364.3876518943077372 ) ) ;
#46615 = CARTESIAN_POINT ( 'NONE',  ( 43.60372932191738471, 12.79097968492800419, -330.4845513384636888 ) ) ;
#46616 = CARTESIAN_POINT ( 'NONE',  ( 160.0134857714809868, 218.2058721980534131, -202.3628264432244350 ) ) ;
#46617 = CARTESIAN_POINT ( 'NONE',  ( -89.20749389083766800, -277.0018624060468255, -322.0328857616854066 ) ) ;
#46618 = CARTESIAN_POINT ( 'NONE',  ( 35.89657587248282056, -274.4169574217511354, -266.1347974990356420 ) ) ;
#46619 = CARTESIAN_POINT ( 'NONE',  ( -114.1596139752474812, -272.2906471836773790, -264.6235902141106067 ) ) ;
#46620 = CARTESIAN_POINT ( 'NONE',  ( 104.1431745715192108, 114.1911308902789131, -280.0153630978813908 ) ) ;
#46621 = EDGE_CURVE ( 'NONE', #64177, #65891, #61781, .T. ) ;
#46622 = CARTESIAN_POINT ( 'NONE',  ( -110.2022031407864944, -276.9397264110240826, -293.8694482995268231 ) ) ;
#46623 = CARTESIAN_POINT ( 'NONE',  ( -105.3191693759786176, -274.7018240896084649, -240.9559402438141262 ) ) ;
#46624 = ORIENTED_EDGE ( 'NONE', *, *, #9108, .F. ) ;
#46625 = CARTESIAN_POINT ( 'NONE',  ( -106.0883560879463232, -290.7153304748176197, -295.0974422026754382 ) ) ;
#46626 = CARTESIAN_POINT ( 'NONE',  ( -23.40650237791145116, -299.0252869540051961, -193.5207482409714714 ) ) ;
#46627 = CARTESIAN_POINT ( 'NONE',  ( -75.75462430054365370, -298.0464484496349087, -203.6368322189051412 ) ) ;
#46628 = CARTESIAN_POINT ( 'NONE',  ( 17.08198505742569751, -294.4149836624684440, -319.0324314909709074 ) ) ;
#46629 = EDGE_LOOP ( 'NONE', ( #49456, #27064 ) ) ;
#46630 = CARTESIAN_POINT ( 'NONE',  ( -5.861986287342172197, -278.5616776875972391, -339.0513051859056191 ) ) ;
#46631 = CARTESIAN_POINT ( 'NONE',  ( -38.73772207297331960, -282.5768779335834324, -347.2869135665104068 ) ) ;
#46632 = CARTESIAN_POINT ( 'NONE',  ( -109.0643579511549603, -279.4325707987173359, -285.5297180951608311 ) ) ;
#46633 = CARTESIAN_POINT ( 'NONE',  ( 9.913641704785165487, -278.1719366065626673, -329.9338413607540588 ) ) ;
#46634 = CARTESIAN_POINT ( 'NONE',  ( -68.27882090709577767, -296.2123935670972514, -203.5770705003258172 ) ) ;
#46635 = CARTESIAN_POINT ( 'NONE',  ( 150.4957602436334412, 21.00000000000000000, -3.637614988394444637 ) ) ;
#46636 = CARTESIAN_POINT ( 'NONE',  ( -96.88446650811557959, -278.1288498162246015, -312.6162137463947488 ) ) ;
#46637 = CARTESIAN_POINT ( 'NONE',  ( -36.95084140150425611, -274.8597892339802229, -193.5105632280675536 ) ) ;
#46638 = CARTESIAN_POINT ( 'NONE',  ( -40.33633225810174849, -287.7738592789223162, -346.8223364624061560 ) ) ;
#46639 = CARTESIAN_POINT ( 'NONE',  ( -34.21280475890486628, -276.0916655243986497, -195.4264086363318995 ) ) ;
#46640 = CARTESIAN_POINT ( 'NONE',  ( 39.04232645707350713, -274.1014035657841532, -268.3395408849036698 ) ) ;
#46641 = DIRECTION ( 'NONE',  ( 0.000000000000000000, -1.000000000000000000, 0.000000000000000000 ) ) ;
#46642 = CARTESIAN_POINT ( 'NONE',  ( -71.25667532229101653, -288.7090670983927794, -335.2010096735273237 ) ) ;
#46643 = CARTESIAN_POINT ( 'NONE',  ( -114.1071690859248378, -283.8338513835529398, -275.7024244056433986 ) ) ;
#46644 = CARTESIAN_POINT ( 'NONE',  ( 34.92505048358838593, -279.9999797905764467, -286.3451967039497958 ) ) ;
#46646 = CARTESIAN_POINT ( 'NONE',  ( -106.9020194466564675, -282.9790879706035867, -243.8530782145600710 ) ) ;
#46645 = CARTESIAN_POINT ( 'NONE',  ( 31.90291973362528211, -280.4577649308583318, -295.4226713768119907 ) ) ;
#46647 = CARTESIAN_POINT ( 'NONE',  ( -104.7344854773557188, -292.1171017490884765, -303.3901034200227400 ) ) ;
#46648 = CARTESIAN_POINT ( 'NONE',  ( -106.6340168383098899, -279.4352169025285093, -294.7165126826161554 ) ) ;
#46649 = DIRECTION ( 'NONE',  ( -1.000000000000000000, 0.000000000000000000, 0.000000000000000000 ) ) ;
#46650 = CARTESIAN_POINT ( 'NONE',  ( -63.65507890920710565, -281.7894108878634825, -341.8736799001981126 ) ) ;
#46651 = CARTESIAN_POINT ( 'NONE',  ( 36.86904808483186713, -295.4085114551244828, -259.1614731028344636 ) ) ;
#46652 = CARTESIAN_POINT ( 'NONE',  ( -56.28211438996942206, -278.0513834950457976, -196.7185677521244145 ) ) ;
#46653 = CARTESIAN_POINT ( 'NONE',  ( -46.99507195992543274, -285.1746618724193922, -344.9053386650672337 ) ) ;
#46654 = CARTESIAN_POINT ( 'NONE',  ( 199.7657144415678658, 24.99747890858082044, 9.999999999999998224 ) ) ;
#46655 = CARTESIAN_POINT ( 'NONE',  ( -103.8761969678313477, -292.0004431222741914, -306.1727770573348835 ) ) ;
#46656 = CARTESIAN_POINT ( 'NONE',  ( 25.41913416240550916, -286.1612057914416596, -226.0074409139718057 ) ) ;
#46657 = CARTESIAN_POINT ( 'NONE',  ( -38.89420052928657157, -290.4322239426742840, -196.5774466202844053 ) ) ;
#46658 = CARTESIAN_POINT ( 'NONE',  ( -48.18343439339133027, -276.7382201398716006, -436.3198488720709634 ) ) ;
#46659 = CARTESIAN_POINT ( 'NONE',  ( 18.67349055953226866, -274.9089592096100318, -317.9378128175799247 ) ) ;
#46660 = CARTESIAN_POINT ( 'NONE',  ( -34.27346081750354045, -293.1527472614341150, -344.5328874755946345 ) ) ;
#46661 = DIRECTION ( 'NONE',  ( -0.000000000000000000, -0.000000000000000000, -1.000000000000000000 ) ) ;
#46662 = LINE ( 'NONE', #75566, #89723 ) ;
#46663 = CARTESIAN_POINT ( 'NONE',  ( 22.57580596936763229, -291.3941324423157084, -223.0898318017452198 ) ) ;
#46664 = CARTESIAN_POINT ( 'NONE',  ( -77.50130454998196683, -287.1039550906161253, -208.3840265463012145 ) ) ;
#46665 = CARTESIAN_POINT ( 'NONE',  ( -40.32175890250741190, -287.3289639892508376, -346.3022385609456251 ) ) ;
#46666 = CARTESIAN_POINT ( 'NONE',  ( 9.390807003501517869, -288.1346072790750554, -213.5152941022397783 ) ) ;
#46667 = CARTESIAN_POINT ( 'NONE',  ( 153.8109486292483439, 20.54314272855871337, -10.84972530314838579 ) ) ;
#46668 = CARTESIAN_POINT ( 'NONE',  ( 14.20438381706701314, -289.1077625939840345, -322.2803144007839364 ) ) ;
#46669 = CARTESIAN_POINT ( 'NONE',  ( 35.48630691864657649, -295.2838994834227719, -250.9597017114630830 ) ) ;
#46670 = CARTESIAN_POINT ( 'NONE',  ( 164.6329196456214277, 215.0000000000000568, 23.09031830825856346 ) ) ;
#46671 = CIRCLE ( 'NONE', #10387, 22.83127060016883192 ) ;
#46672 = CARTESIAN_POINT ( 'NONE',  ( 4.947616718786922441, -287.8146017465406885, -206.4260243713895306 ) ) ;
#46673 = CARTESIAN_POINT ( 'NONE',  ( -96.81099048729556955, -275.9970493877451077, -316.9735380710748132 ) ) ;
#46674 = CARTESIAN_POINT ( 'NONE',  ( -41.37909123622963392, -277.4349307691293234, -347.2472297835606128 ) ) ;
#46675 = CARTESIAN_POINT ( 'NONE',  ( -14.28220519702349023, -290.4285825203360787, -198.3508233262575402 ) ) ;
#46676 = CARTESIAN_POINT ( 'NONE',  ( -75.00793408253187522, -279.5646736540456914, -203.2026872408534359 ) ) ;
#46677 = CARTESIAN_POINT ( 'NONE',  ( -94.89760861249123991, -299.1911398577760792, -222.8105603503004204 ) ) ;
#46678 = CARTESIAN_POINT ( 'NONE',  ( -48.18343439337080980, -261.9263060112091921, -500.2732637504696527 ) ) ;
#46679 = CARTESIAN_POINT ( 'NONE',  ( -109.2658526243514672, -282.8278768411228725, -248.9228722796012505 ) ) ;
#46680 = CARTESIAN_POINT ( 'NONE',  ( -48.18343439339133738, -263.2803689379327921, -495.2320347593006886 ) ) ;
#46681 = CARTESIAN_POINT ( 'NONE',  ( -107.6063063982399086, -277.0066196533318248, -246.2503205628196383 ) ) ;
#46682 = CARTESIAN_POINT ( 'NONE',  ( 28.96584730303280963, -279.0860963705572999, -235.2030773423830396 ) ) ;
#46683 = DIRECTION ( 'NONE',  ( -0.000000000000000000, -1.000000000000000000, -0.000000000000000000 ) ) ;
#46684 = CARTESIAN_POINT ( 'NONE',  ( 20.28382865853616579, -274.7143387070482277, -320.4009455897826228 ) ) ;
#46685 = CARTESIAN_POINT ( 'NONE',  ( -111.0683352647907753, -298.0935084864881333, -268.7367482327626931 ) ) ;
#46686 = CARTESIAN_POINT ( 'NONE',  ( -8.169255774653347402, -281.5994052134367394, -341.3431679827423864 ) ) ;
#46687 = CARTESIAN_POINT ( 'NONE',  ( -110.2858228500285662, -297.5864049509891629, -263.2888161205055439 ) ) ;
#46688 = CARTESIAN_POINT ( 'NONE',  ( -112.6566200674386806, -298.0366440087377669, -256.9089394205408325 ) ) ;
#46689 = CARTESIAN_POINT ( 'NONE',  ( -46.17713153867786247, -273.6036958065105296, -197.8764807238676156 ) ) ;
#46690 = CARTESIAN_POINT ( 'NONE',  ( 22.57668471328187465, -294.9357139609228398, -225.2524956371835003 ) ) ;
#46691 = CARTESIAN_POINT ( 'NONE',  ( 39.70250112861683789, -287.7336901139755128, -271.5491702985265761 ) ) ;
#46692 = CARTESIAN_POINT ( 'NONE',  ( -112.6071379406231188, -276.7241942098969503, -263.1270051354865132 ) ) ;
#46693 = CARTESIAN_POINT ( 'NONE',  ( -95.65952686948801897, -291.0646077996743202, -220.0614357714437972 ) ) ;
#46694 = CARTESIAN_POINT ( 'NONE',  ( 16.15450826230483727, -285.8935200104600085, -220.3269695680680513 ) ) ;
#46695 = CARTESIAN_POINT ( 'NONE',  ( -55.67460081037683750, -289.8161491580938218, -197.5827413428565649 ) ) ;
#46696 = ORIENTED_EDGE ( 'NONE', *, *, #29388, .F. ) ;
#46697 = CARTESIAN_POINT ( 'NONE',  ( 24.80950920047307307, -22.49099280560490399, -345.4124233396505019 ) ) ;
#46698 = CARTESIAN_POINT ( 'NONE',  ( -58.71311437851345971, -288.8436439243002951, -340.2799190209283324 ) ) ;
#46699 = DIRECTION ( 'NONE',  ( 0.000000000000000000, 0.000000000000000000, 1.000000000000000000 ) ) ;
#46700 = CARTESIAN_POINT ( 'NONE',  ( -89.73443779016372446, -286.2760793483358839, -214.1833619613309168 ) ) ;
#46701 = CARTESIAN_POINT ( 'NONE',  ( 34.24775278838919945, -292.2571528448036702, -242.5054902150876615 ) ) ;
#46702 = CARTESIAN_POINT ( 'NONE',  ( 16.64182079220857347, -282.4041863108669759, -216.5077882062450385 ) ) ;
#46703 = CARTESIAN_POINT ( 'NONE',  ( -1.382128565355458694, -281.8340925258497691, -202.8318096285994159 ) ) ;
#46704 = CARTESIAN_POINT ( 'NONE',  ( -32.14781935606998786, -282.8181302018990664, -343.1761137391787315 ) ) ;
#46705 = CARTESIAN_POINT ( 'NONE',  ( -111.2153881658450416, -296.2792015064840712, -292.1257786404678995 ) ) ;
#46706 = CARTESIAN_POINT ( 'NONE',  ( -68.50683993270271799, -274.9490711843843087, -203.7892500557035760 ) ) ;
#46707 = CARTESIAN_POINT ( 'NONE',  ( 19.75054632130364496, -290.9041815193578486, -222.2745065287639079 ) ) ;
#46708 = CARTESIAN_POINT ( 'NONE',  ( -36.46502778714970816, -296.9837068221518166, -197.0521690192059054 ) ) ;
#46709 = VERTEX_POINT ( 'NONE', #62300 ) ;
#46710 = LINE ( 'NONE', #68048, #86421 ) ;
#46711 = CARTESIAN_POINT ( 'NONE',  ( -93.63231911263713414, -285.7914550963929514, -319.0906752722166857 ) ) ;
#46712 = CARTESIAN_POINT ( 'NONE',  ( 4.071992744360424687, -295.5882287311251844, -334.9712940604021014 ) ) ;
#46713 = CARTESIAN_POINT ( 'NONE',  ( -94.20656074971103067, -285.8525113270188740, -224.4034884059300623 ) ) ;
#46714 = EDGE_CURVE ( 'NONE', #58673, #76475, #31563, .T. ) ;
#46715 = CARTESIAN_POINT ( 'NONE',  ( 23.32470423266149240, -275.2411354751882300, -317.4186696975211817 ) ) ;
#46716 = CARTESIAN_POINT ( 'NONE',  ( 30.80474116737842749, -293.7419871243301372, -234.6182148998019557 ) ) ;
#46717 = CARTESIAN_POINT ( 'NONE',  ( 0.9187094753207517561, -284.6964468662071113, -204.9514780428838208 ) ) ;
#46718 = CARTESIAN_POINT ( 'NONE',  ( -4.616987851408536514, -292.8048746146095596, -200.6844540407172133 ) ) ;
#46719 = CARTESIAN_POINT ( 'NONE',  ( -108.9586352519391852, -290.6966462182868440, -284.6764448294320005 ) ) ;
#46720 = CARTESIAN_POINT ( 'NONE',  ( -54.94434090351493438, -232.1443419142230766, 22.50000000000000000 ) ) ;
#46721 = CYLINDRICAL_SURFACE ( 'NONE', #5508, 6.286090667950827715 ) ;
#46722 = CARTESIAN_POINT ( 'NONE',  ( -101.8397201137918273, -254.3509017731851429, -324.1331500758875563 ) ) ;
#46723 = CARTESIAN_POINT ( 'NONE',  ( -106.3701399115108615, -285.6518744641234093, -302.8846825465999473 ) ) ;
#46724 = CARTESIAN_POINT ( 'NONE',  ( 31.09738932201053885, -296.4086741954486115, -195.3901485728259502 ) ) ;
#46725 = ORIENTED_EDGE ( 'NONE', *, *, #33278, .T. ) ;
#46726 = CARTESIAN_POINT ( 'NONE',  ( -21.33405164084337713, -281.7624509208380914, -341.9534166131051052 ) ) ;
#46727 = CARTESIAN_POINT ( 'NONE',  ( -111.3157526888499831, -278.4859703168679061, -249.0636101637744559 ) ) ;
#46728 = CARTESIAN_POINT ( 'NONE',  ( -84.61512365627537235, -281.3998237904342545, -212.2832385099890189 ) ) ;
#46729 = CARTESIAN_POINT ( 'NONE',  ( -101.3712253486714729, -256.2545489327123391, -325.4733069935736012 ) ) ;
#46730 = CARTESIAN_POINT ( 'NONE',  ( -63.72572039728786564, -281.9642387780498325, -342.0722730902862168 ) ) ;
#46731 = CARTESIAN_POINT ( 'NONE',  ( 5.693782458913366540, -284.6580936043405359, -209.3077381165867905 ) ) ;
#46732 = CARTESIAN_POINT ( 'NONE',  ( -46.03646689318789242, -299.7034568587974377, -194.8735359340652735 ) ) ;
#46733 = CARTESIAN_POINT ( 'NONE',  ( -102.8205296441016259, -296.6041395492026140, -302.8870183449707838 ) ) ;
#46734 = ORIENTED_EDGE ( 'NONE', *, *, #45734, .T. ) ;
#46735 = CARTESIAN_POINT ( 'NONE',  ( 30.31625490522999655, -291.8527042035598242, -241.5316400211297605 ) ) ;
#46736 = CARTESIAN_POINT ( 'NONE',  ( -6.607810289531760972, -277.3105137605671189, -340.8646517337873547 ) ) ;
#46737 = CARTESIAN_POINT ( 'NONE',  ( 27.86128662085983976, -275.1066291771242618, -237.5347487191553739 ) ) ;
#46738 = CARTESIAN_POINT ( 'NONE',  ( 38.61990525563883381, -274.3399952410734386, -259.8099560949489728 ) ) ;
#46739 = FACE_OUTER_BOUND ( 'NONE', #10313, .T. ) ;
#46740 = CARTESIAN_POINT ( 'NONE',  ( -95.56402688411247937, -271.2033622209871169, -223.0637146685942866 ) ) ;
#46741 = ADVANCED_FACE ( 'NONE', ( #19205 ), #11162, .T. ) ;
#46742 = CARTESIAN_POINT ( 'NONE',  ( -2.222015681115426133, -296.0217567322440573, -338.2228454791646186 ) ) ;
#46743 = CARTESIAN_POINT ( 'NONE',  ( 138.6539576904058606, 250.5000000000000568, 10.50000000000000000 ) ) ;
#46744 = VECTOR ( 'NONE', #74411, 1000.000000000000000 ) ;
#46745 = CARTESIAN_POINT ( 'NONE',  ( -43.52944128795684264, -249.3926482227765860, -482.3108334129058790 ) ) ;
#46746 = CARTESIAN_POINT ( 'NONE',  ( -107.2766376429477901, -285.3416583648190112, -292.3458988216260650 ) ) ;
#46747 = CARTESIAN_POINT ( 'NONE',  ( 23.76334358981527473, -282.7039803391659234, -225.1931243597964283 ) ) ;
#46748 = CARTESIAN_POINT ( 'NONE',  ( -94.36973702319804147, -283.2551381691380357, -316.1160935256242510 ) ) ;
#46749 = CARTESIAN_POINT ( 'NONE',  ( -8.443999797408698882, -275.0673268475259761, -338.2818266226420292 ) ) ;
#46750 = CARTESIAN_POINT ( 'NONE',  ( -5.481685914308793706, -284.4890048819452204, -337.4258668135261132 ) ) ;
#46751 = CARTESIAN_POINT ( 'NONE',  ( -81.24783278021497779, -276.1412367623302657, -329.5469208930792888 ) ) ;
#46752 = CARTESIAN_POINT ( 'NONE',  ( -6.411012262670094941, -275.5479530525081486, -203.8967017676368698 ) ) ;
#46753 = DIRECTION ( 'NONE',  ( -0.000000000000000000, -1.000000000000000000, -0.000000000000000000 ) ) ;
#46754 = CARTESIAN_POINT ( 'NONE',  ( -107.2764065286123127, -279.7641522453856169, -238.4006703163460941 ) ) ;
#46755 = EDGE_LOOP ( 'NONE', ( #50378, #38375, #93335, #62209 ) ) ;
#46756 = EDGE_CURVE ( 'NONE', #69769, #38673, #23981, .T. ) ;
#46757 = CARTESIAN_POINT ( 'NONE',  ( 200.2454457599218927, 15.96501597606886769, 10.07064028581559256 ) ) ;
#46758 = CARTESIAN_POINT ( 'NONE',  ( -94.89405966539744952, -287.0889195726613821, -221.0073457029371298 ) ) ;
#46759 = CARTESIAN_POINT ( 'NONE',  ( 14.42332061702167501, -293.4986289255981546, -322.1332514729375589 ) ) ;
#46760 = CARTESIAN_POINT ( 'NONE',  ( -113.5639656404338353, -290.0330084121748655, -259.7991293808597675 ) ) ;
#46762 = CARTESIAN_POINT ( 'NONE',  ( -108.7233414855515008, -289.0469154973205832, -250.8000522592148229 ) ) ;
#46761 = CARTESIAN_POINT ( 'NONE',  ( 35.54144204940245544, -286.2611539220728218, -280.6223890411409911 ) ) ;
#46763 = CARTESIAN_POINT ( 'NONE',  ( -109.1050753979022545, -285.5544002912084238, -285.8203797214163160 ) ) ;
#46764 = CARTESIAN_POINT ( 'NONE',  ( -110.7544795691030117, -276.7498517916012588, -254.9511784583348799 ) ) ;
#46765 = CARTESIAN_POINT ( 'NONE',  ( 19.95773687891198378, -286.6389751872345641, -320.6123815290641232 ) ) ;
#46766 = CARTESIAN_POINT ( 'NONE',  ( 36.80438653099493962, -289.4063156119605651, -258.9904778047576883 ) ) ;
#46767 = CARTESIAN_POINT ( 'NONE',  ( 30.03257463744635558, -285.9920934755145367, -303.8061236370199367 ) ) ;
#46768 = CARTESIAN_POINT ( 'NONE',  ( -33.47184316135159321, -283.9435351554913041, -343.5067102684656106 ) ) ;
#46769 = CARTESIAN_POINT ( 'NONE',  ( -18.16683304624904594, -290.8057285031925403, -343.0409150103961906 ) ) ;
#46770 = CARTESIAN_POINT ( 'NONE',  ( 208.4306832106270804, -198.2391364535880598, 0.000000000000000000 ) ) ;
#46771 = CARTESIAN_POINT ( 'NONE',  ( 195.9944643786954259, 40.77738931532193334, 13.32058305467766957 ) ) ;
#46772 = CARTESIAN_POINT ( 'NONE',  ( -110.8982473963231712, -298.2513033762172654, -287.7013503410714179 ) ) ;
#46773 = CARTESIAN_POINT ( 'NONE',  ( 36.44873747522782281, -279.7251665673247771, -283.8483111841259756 ) ) ;
#46774 = CARTESIAN_POINT ( 'NONE',  ( 24.69015057209802677, -292.1460437121533573, -225.0156847003438827 ) ) ;
#46775 = CARTESIAN_POINT ( 'NONE',  ( -94.21720025602796511, -295.6116996783073319, -223.3136229615314789 ) ) ;
#46776 = CARTESIAN_POINT ( 'NONE',  ( 30.48300365769452114, -279.8598692033370980, -242.0582376842496899 ) ) ;
#46777 = CARTESIAN_POINT ( 'NONE',  ( 35.24324344331149916, -273.4176901811385960, -253.7891960201028496 ) ) ;
#46778 = CARTESIAN_POINT ( 'NONE',  ( -78.21016175967831430, -296.9293425162473454, -331.5045904921583997 ) ) ;
#46779 = CYLINDRICAL_SURFACE ( 'NONE', #36822, 2.000000000000000000 ) ;
#46780 = CARTESIAN_POINT ( 'NONE',  ( -43.21688256451417232, -296.4592596781590714, -194.2282321944719001 ) ) ;
#46781 = CARTESIAN_POINT ( 'NONE',  ( -41.90738058935478705, -293.3486667304447906, -346.2622022036466092 ) ) ;
#46782 = CARTESIAN_POINT ( 'NONE',  ( 32.35327366383609160, -294.6642029286959996, -246.5808908674738689 ) ) ;
#46783 = DIRECTION ( 'NONE',  ( -0.000000000000000000, -1.000000000000000000, -0.000000000000000000 ) ) ;
#46784 = CARTESIAN_POINT ( 'NONE',  ( -3.570790652506796281, -293.3127541505124327, -205.4602135159243517 ) ) ;
#46785 = DIRECTION ( 'NONE',  ( 0.000000000000000000, 0.000000000000000000, 1.000000000000000000 ) ) ;
#46787 = CARTESIAN_POINT ( 'NONE',  ( -7.988308176006066574, -294.6565936969429913, -337.2131452401724232 ) ) ;
#46786 = CARTESIAN_POINT ( 'NONE',  ( -92.25068126354996423, -281.8523750196478090, -321.9882835814649980 ) ) ;
#46788 = CARTESIAN_POINT ( 'NONE',  ( -16.14183752788294512, -282.7855381839688107, -344.4404932703343434 ) ) ;
#46789 = CARTESIAN_POINT ( 'NONE',  ( -4.309626302289554900, -282.4042502825120096, -202.3895616829989876 ) ) ;
#46790 = CARTESIAN_POINT ( 'NONE',  ( -113.4658671525149316, -284.3663702048252730, -258.5705399046373714 ) ) ;
#46791 = CARTESIAN_POINT ( 'NONE',  ( -109.8794375153375427, -288.7894100610452597, -251.9160026082831791 ) ) ;
#46792 = CARTESIAN_POINT ( 'NONE',  ( 201.2104617360081704, 41.21457449016152452, 10.49999999999999822 ) ) ;
#46793 = CARTESIAN_POINT ( 'NONE',  ( -1.972848693455385272, -281.0722269068924106, -337.9758508630173424 ) ) ;
#46794 = CARTESIAN_POINT ( 'NONE',  ( -29.02442258126227514, -287.8695485624459138, -346.6529711315224063 ) ) ;
#46795 = FACE_OUTER_BOUND ( 'NONE', #7246, .T. ) ;
#46796 = CARTESIAN_POINT ( 'NONE',  ( 6.554967427744428754, -296.0447774294781880, -329.7503844756199101 ) ) ;
#46797 = CARTESIAN_POINT ( 'NONE',  ( -51.18789780538250511, -278.6510966314526172, -345.5069036346620805 ) ) ;
#46798 = CARTESIAN_POINT ( 'NONE',  ( -34.30820238962408553, -279.7580201447307786, -197.3904638657029693 ) ) ;
#46799 = CARTESIAN_POINT ( 'NONE',  ( -25.02353168793252536, -292.3717848219060897, -194.3528109972795619 ) ) ;
#46800 = CARTESIAN_POINT ( 'NONE',  ( -112.0596581951970450, -282.7797534199804090, -258.7677926004978417 ) ) ;
#46801 = CARTESIAN_POINT ( 'NONE',  ( -94.60523539357275524, -279.8821134007427531, -318.8153014472902100 ) ) ;
#46803 = CARTESIAN_POINT ( 'NONE',  ( -2.316393565318947356, -291.5864189557678401, -206.0301879968598087 ) ) ;
#46802 = VECTOR ( 'NONE', #35071, 1000.000000000000000 ) ;
#46804 = CARTESIAN_POINT ( 'NONE',  ( -111.6174256862581586, -294.6866888243472999, -259.8704963559827661 ) ) ;
#46805 = ORIENTED_EDGE ( 'NONE', *, *, #87350, .T. ) ;
#46806 = DIRECTION ( 'NONE',  ( 0.6056179655966479336, -0.7957555401921982963, 0.000000000000000000 ) ) ;
#46807 = CARTESIAN_POINT ( 'NONE',  ( -5.520368767034310231, -294.1295451126133003, -336.1426467329376351 ) ) ;
#46808 = CARTESIAN_POINT ( 'NONE',  ( 184.7149167944524493, -12.49482340714361506, 9.974999999999996092 ) ) ;
#46809 = VECTOR ( 'NONE', #22924, 1000.000000000000000 ) ;
#46810 = CARTESIAN_POINT ( 'NONE',  ( -6.998514795304330072, -292.1237833571632336, -333.4427485647536855 ) ) ;
#46811 = CARTESIAN_POINT ( 'NONE',  ( -112.9075915997575663, -271.9274202390725463, -256.1504789243317646 ) ) ;
#46812 = CARTESIAN_POINT ( 'NONE',  ( 26.71564516297948089, -288.3141868991640990, -228.5286570616940764 ) ) ;
#46813 = CARTESIAN_POINT ( 'NONE',  ( 19.51214923481084895, -288.0328525565698783, -316.1501976540363898 ) ) ;
#46814 = CARTESIAN_POINT ( 'NONE',  ( -70.74998003744313735, -279.0212814498722764, -336.0466916479080624 ) ) ;
#46815 = CARTESIAN_POINT ( 'NONE',  ( -35.81142357793161324, -299.8317057372617569, -196.3473114662746184 ) ) ;
#46816 = CARTESIAN_POINT ( 'NONE',  ( -87.37737015061139800, -276.5639099852722893, -324.0599282993237011 ) ) ;
#46817 = ORIENTED_EDGE ( 'NONE', *, *, #18018, .T. ) ;
#46818 = CARTESIAN_POINT ( 'NONE',  ( -113.0678965813541197, -272.5634699782864914, -256.1286169489388271 ) ) ;
#46819 = CARTESIAN_POINT ( 'NONE',  ( -109.5104580981725206, -292.7090905254490849, -252.0613424212702114 ) ) ;
#46820 = CARTESIAN_POINT ( 'NONE',  ( 24.15662711807824081, -294.5486163513410816, -225.3678277859163472 ) ) ;
#46821 = CARTESIAN_POINT ( 'NONE',  ( 196.3886764727502054, 69.83403101108301314, -15.08154681515735085 ) ) ;
#46822 = CARTESIAN_POINT ( 'NONE',  ( -88.72683398023475831, -290.4486016215405471, -322.3559320226291902 ) ) ;
#46823 = FACE_OUTER_BOUND ( 'NONE', #21989, .T. ) ;
#46824 = EDGE_CURVE ( 'NONE', #27803, #12480, #66318, .T. ) ;
#46825 = CARTESIAN_POINT ( 'NONE',  ( 1.094246314520575192, -290.6986517721620089, -205.0096254285737700 ) ) ;
#46826 = CARTESIAN_POINT ( 'NONE',  ( -33.34011082396492753, -298.4342490044799092, -193.3820424796144266 ) ) ;
#46827 = CARTESIAN_POINT ( 'NONE',  ( -40.51464284768410096, -297.6779089888000840, -197.3963899822251449 ) ) ;
#46828 = CARTESIAN_POINT ( 'NONE',  ( 73.43068321062709458, -134.2391364535880598, -5.025000000000002132 ) ) ;
#46829 = CARTESIAN_POINT ( 'NONE',  ( 189.4188515237862589, 293.9636489450775798, 9.103929867429222611 ) ) ;
#46830 = CARTESIAN_POINT ( 'NONE',  ( -82.42726890285256047, -291.1755718613267732, -331.9240876904858624 ) ) ;
#46831 = CARTESIAN_POINT ( 'NONE',  ( -115.3288506153726871, -286.8376638359844719, -288.1938231032136741 ) ) ;
#46832 = CARTESIAN_POINT ( 'NONE',  ( -65.81377399587834987, -287.6791493850333836, -201.1006789375407777 ) ) ;
#46833 = CARTESIAN_POINT ( 'NONE',  ( -36.69527521088521382, -272.0601337886153601, -195.5178449881298377 ) ) ;
#46834 = CARTESIAN_POINT ( 'NONE',  ( 36.53832420928921465, -277.5955393794843076, -279.8868183234383196 ) ) ;
#46835 = CARTESIAN_POINT ( 'NONE',  ( -64.57611798041747875, -289.7736945246065261, -201.0681696380719927 ) ) ;
#46836 = CARTESIAN_POINT ( 'NONE',  ( -45.49279707765411729, -279.0146684454041974, -345.7383876816082307 ) ) ;
#46837 = VERTEX_POINT ( 'NONE', #12097 ) ;
#46838 = CARTESIAN_POINT ( 'NONE',  ( -34.85136655472116018, -282.3686655291266447, -343.4330745383493877 ) ) ;
#46839 = CARTESIAN_POINT ( 'NONE',  ( -107.1435071399293406, -280.0409465176456365, -238.4652964810486822 ) ) ;
#46840 = CARTESIAN_POINT ( 'NONE',  ( 35.80115906322091490, -280.0596480845708811, -247.5986298077007746 ) ) ;
#46841 = CARTESIAN_POINT ( 'NONE',  ( 197.4573848121495416, 287.6755661058302849, -96.60709594317813753 ) ) ;
#46842 = CARTESIAN_POINT ( 'NONE',  ( 21.55782282952521101, -277.1579230107995500, -319.5918645658061337 ) ) ;
#46843 = ADVANCED_FACE ( 'NONE', ( #55202 ), #76920, .F. ) ;
#46844 = APPLICATION_PROTOCOL_DEFINITION ( 'draft international standard', 'automotive_design', 1998, #929 ) ;
#46846 = CARTESIAN_POINT ( 'NONE',  ( 2.043418945047154711, -276.0894731127471573, -205.0042503412220753 ) ) ;
#46845 = B_SPLINE_CURVE_WITH_KNOTS ( 'NONE', 3,
 ( #20345, #92760, #13252, #49677, #29314, #56817, #72406, #85659, #86578, #63454, #19862, #41628, #48733, #35946, #64405, #57277, #27440, #14190, #70548, #42561, #71478, #5671, #86119, #34546, #57732, #79038, #21747, #79514 ),
 .UNSPECIFIED., .F., .F.,
 ( 4, 2, 2, 2, 2, 2, 2, 2, 2, 2, 2, 2, 2, 4 ),
 ( 0.007868691692155720466, 0.008845612455071254210, 0.009334072836528988990, 0.009822533217986722034, 0.01031099359944445681, 0.01079945398090218986, 0.01128791436235992290, 0.01177637474381765595, 0.01226483512527539073, 0.01275329550673312551, 0.01324175588819085855, 0.01373021626964859160, 0.01470713703256412014, 0.01568405779547964868 ),
 .UNSPECIFIED. ) ;
#46847 = CARTESIAN_POINT ( 'NONE',  ( 21.31550574532285580, -296.6948066931273615, -317.0979686699210447 ) ) ;
#46848 = ORIENTED_EDGE ( 'NONE', *, *, #65933, .T. ) ;
#46849 = ORIENTED_EDGE ( 'NONE', *, *, #52243, .T. ) ;
#46850 = CARTESIAN_POINT ( 'NONE',  ( 60.83730532400070246, -250.0090898647485176, 21.50000000000000000 ) ) ;
#46851 = CARTESIAN_POINT ( 'NONE',  ( -42.67272446439136502, -290.2005196228595310, -343.5269567670270021 ) ) ;
#46852 = CARTESIAN_POINT ( 'NONE',  ( 31.78079137556968092, -288.9019993375378021, -238.6741920333060420 ) ) ;
#46853 = CARTESIAN_POINT ( 'NONE',  ( -107.0963991988017767, -290.1906483991432424, -248.4517607941682513 ) ) ;
#46854 = CARTESIAN_POINT ( 'NONE',  ( -57.73358334943154091, -285.3034630765065458, -196.1188992306328203 ) ) ;
#46855 = CARTESIAN_POINT ( 'NONE',  ( 196.1963538710216994, 282.2246705312485915, -40.00000000000000711 ) ) ;
#46856 = CARTESIAN_POINT ( 'NONE',  ( 36.48818723402094832, -279.9288325332478280, -268.5844290499083513 ) ) ;
#46857 = CARTESIAN_POINT ( 'NONE',  ( 14.97032150275138562, -290.1651754952927718, -323.0329118777052599 ) ) ;
#46858 = CARTESIAN_POINT ( 'NONE',  ( -37.56185159518126682, -281.5348691761150235, -344.0666728013138709 ) ) ;
#46859 = CARTESIAN_POINT ( 'NONE',  ( -81.59810958637109479, -280.7509618162966945, -211.6234148026327944 ) ) ;
#46860 = CARTESIAN_POINT ( 'NONE',  ( 37.14560079645574575, -288.2604895310776101, -251.8014246977716084 ) ) ;
#46861 = CARTESIAN_POINT ( 'NONE',  ( -103.1837504123561615, -278.6150238893242772, -302.1453812113981030 ) ) ;
#46862 = CARTESIAN_POINT ( 'NONE',  ( -98.87641883833006773, -289.9570058609152738, -224.7158321821602271 ) ) ;
#46863 = CARTESIAN_POINT ( 'NONE',  ( -54.93758100951860968, -286.6342948651698066, -195.5644349277536946 ) ) ;
#46864 = CARTESIAN_POINT ( 'NONE',  ( -73.58957004187121242, -286.0769947834070877, -202.4373991479402832 ) ) ;
#46865 = CARTESIAN_POINT ( 'NONE',  ( -65.31373319830633761, -283.5948945566061070, -337.8029401839038997 ) ) ;
#46866 = VERTEX_POINT ( 'NONE', #33885 ) ;
#46867 = LINE ( 'NONE', #76709, #20134 ) ;
#46868 = CARTESIAN_POINT ( 'NONE',  ( -69.12693003084130794, -293.4989792609995334, -201.5719757696961096 ) ) ;
#46869 = CARTESIAN_POINT ( 'NONE',  ( 30.46963714374363263, -291.7757163938274516, -234.8221605571063435 ) ) ;
#46870 = CARTESIAN_POINT ( 'NONE',  ( 35.33806040673717064, -274.7345947034932578, -279.7684096025811868 ) ) ;
#46871 = CARTESIAN_POINT ( 'NONE',  ( -109.3450226567610883, -295.5571032897107102, -297.5083259787439260 ) ) ;
#46872 = CIRCLE ( 'NONE', #69609, 2.999999999999997780 ) ;
#46873 = CARTESIAN_POINT ( 'NONE',  ( -66.82384580459678602, -290.1385310595077272, -202.8221600386912939 ) ) ;
#46874 = CARTESIAN_POINT ( 'NONE',  ( -47.96027363389119813, -293.4287651625002695, -343.6607731370596639 ) ) ;
#46875 = CARTESIAN_POINT ( 'NONE',  ( -81.98264858339445027, -292.6335779687863123, -212.0360335224583821 ) ) ;
#46876 = CARTESIAN_POINT ( 'NONE',  ( 207.6662022560303171, 36.29800326561214519, 14.90057469441918947 ) ) ;
#46877 = CARTESIAN_POINT ( 'NONE',  ( 14.20003917586191555, -290.7735027746303444, -215.5769466340024678 ) ) ;
#46878 = AXIS2_PLACEMENT_3D ( 'NONE', #79096, #78625, #13302 ) ;
#46879 = CARTESIAN_POINT ( 'NONE',  ( 33.08241283956743217, -295.2159507105831153, -244.4172390993785768 ) ) ;
#46880 = CARTESIAN_POINT ( 'NONE',  ( 19.70428784401630651, -289.1406051773078616, -316.2867503160322258 ) ) ;
#46881 = CARTESIAN_POINT ( 'NONE',  ( -39.88170544273447859, -279.0637725825090456, -345.6862893238195511 ) ) ;
#46882 = CARTESIAN_POINT ( 'NONE',  ( -104.6341327016061484, -276.8709806574642585, -306.9635391579996053 ) ) ;
#46883 = CARTESIAN_POINT ( 'NONE',  ( -75.69042796910599691, -296.7514776721768612, -203.7152706514069109 ) ) ;
#46884 = CARTESIAN_POINT ( 'NONE',  ( -7.114024572189377338, -274.8898898864312059, -337.9204374448056001 ) ) ;
#46885 = CARTESIAN_POINT ( 'NONE',  ( -95.90894070865891763, -277.2675540450228482, -224.3928957015725132 ) ) ;
#46886 = CARTESIAN_POINT ( 'NONE',  ( -59.45254646894837691, -275.7336684753215650, -343.2826572415415285 ) ) ;
#46887 = CARTESIAN_POINT ( 'NONE',  ( -110.7035680661494297, -295.2945055766592191, -265.9702399943167848 ) ) ;
#46888 = DIRECTION ( 'NONE',  ( -0.000000000000000000, -1.000000000000000000, -0.000000000000000000 ) ) ;
#46889 = CARTESIAN_POINT ( 'NONE',  ( -83.26104478151587784, -274.0549525008167393, -213.4813636368857317 ) ) ;
#46890 = CARTESIAN_POINT ( 'NONE',  ( 209.5769276792742346, 0.02860196560701893168, 7.415405905516098350 ) ) ;
#46892 = CARTESIAN_POINT ( 'NONE',  ( 34.84197555492129084, -275.2407499413783967, -259.3904458100947750 ) ) ;
#46891 = CARTESIAN_POINT ( 'NONE',  ( -54.15959457129459764, -287.2870430271519240, -343.8691761463691705 ) ) ;
#46893 = CARTESIAN_POINT ( 'NONE',  ( 38.02350660930691362, -287.3539724695729092, -254.5148300327509503 ) ) ;
#46894 = CARTESIAN_POINT ( 'NONE',  ( -88.92373787837848909, -275.3300913450562462, -215.6153242181658527 ) ) ;
#46895 = CARTESIAN_POINT ( 'NONE',  ( -99.96823353129545353, -295.1069028351938073, -229.3046556303672503 ) ) ;
#46896 = CARTESIAN_POINT ( 'NONE',  ( -90.33419302872037804, -282.9760711694154338, -326.0753856950369709 ) ) ;
#46897 = DIRECTION ( 'NONE',  ( 0.000000000000000000, 1.000000000000000000, 0.000000000000000000 ) ) ;
#46898 = CARTESIAN_POINT ( 'NONE',  ( 21.47023816398901630, -278.9124881820549149, -223.7988820376661749 ) ) ;
#46899 = DIRECTION ( 'NONE',  ( 0.000000000000000000, 0.000000000000000000, 1.000000000000000000 ) ) ;
#46900 = CARTESIAN_POINT ( 'NONE',  ( -109.5723982504696750, -289.1760770719048423, -283.3940284143973258 ) ) ;
#46901 = CARTESIAN_POINT ( 'NONE',  ( 198.6462973140338875, 41.50354292539933709, 11.14960445194718019 ) ) ;
#46902 = CARTESIAN_POINT ( 'NONE',  ( 151.4851178187871312, 21.00000000000000000, 3.492110388858642889 ) ) ;
#46903 = CARTESIAN_POINT ( 'NONE',  ( -66.07012327224013859, -289.6760666312246144, -201.0675250192834937 ) ) ;
#46904 = CARTESIAN_POINT ( 'NONE',  ( -34.02869719533108395, -275.6147018488665594, -196.7422904642450305 ) ) ;
#46905 = CARTESIAN_POINT ( 'NONE',  ( 38.20931589831229047, -282.8290493070682601, -258.5882457565131176 ) ) ;
#46907 = CARTESIAN_POINT ( 'NONE',  ( -53.68966852611506368, -283.2676916330322001, -341.5591363401455283 ) ) ;
#46906 = CARTESIAN_POINT ( 'NONE',  ( -95.80601951000305405, -271.2871524245595083, -222.4740616317136528 ) ) ;
#46908 = CARTESIAN_POINT ( 'NONE',  ( -2.651801216718761456, -275.9456819964217402, -205.4613041789028216 ) ) ;
#46909 = CARTESIAN_POINT ( 'NONE',  ( 33.01247274742645033, -276.0880278155352698, -250.1080145665276575 ) ) ;
#46910 = EDGE_CURVE ( 'NONE', #25794, #13434, #67789, .T. ) ;
#46911 = CARTESIAN_POINT ( 'NONE',  ( -70.82245150820266133, -285.4939989542326089, -337.4732624858654049 ) ) ;
#46912 = CARTESIAN_POINT ( 'NONE',  ( -83.37405570498910379, -272.3241464575996247, -213.3063345488225764 ) ) ;
#46913 = ORIENTED_EDGE ( 'NONE', *, *, #68145, .F. ) ;
#46914 = CYLINDRICAL_SURFACE ( 'NONE', #9028, 4.999999999999990230 ) ;
#46915 = CARTESIAN_POINT ( 'NONE',  ( 35.48572158426885892, -293.7024345034074599, -295.5278303757756930 ) ) ;
#46916 = CARTESIAN_POINT ( 'NONE',  ( -109.3411367842514750, -286.2769992143743707, -290.1052003954233101 ) ) ;
#46917 = CARTESIAN_POINT ( 'NONE',  ( 208.4306832106271088, 20.44233620800389772, 0.000000000000000000 ) ) ;
#46918 = CARTESIAN_POINT ( 'NONE',  ( -99.86837403722181250, -276.6952119285918457, -220.4570493818173702 ) ) ;
#46919 = CARTESIAN_POINT ( 'NONE',  ( -34.30772645810454691, -276.2120856266992632, -347.1397206309391095 ) ) ;
#46920 = CARTESIAN_POINT ( 'NONE',  ( -94.86788344615027313, -288.2695244997815962, -320.3328965143486471 ) ) ;
#46921 = CARTESIAN_POINT ( 'NONE',  ( -68.05585817551738614, -284.9830711392421563, -337.3487903542435333 ) ) ;
#46922 = CARTESIAN_POINT ( 'NONE',  ( -51.45242795770836608, -278.9952236349207624, -343.0168911265149063 ) ) ;
#46923 = CARTESIAN_POINT ( 'NONE',  ( -85.15841457249160840, -286.8317358163424728, -210.7610499371244543 ) ) ;
#46924 = CARTESIAN_POINT ( 'NONE',  ( 33.86769820320593283, -283.2462194376556681, -246.6556805340865708 ) ) ;
#46925 = CARTESIAN_POINT ( 'NONE',  ( -55.33567763507367232, -273.9935013321080532, -195.4931222970732279 ) ) ;
#46926 = CARTESIAN_POINT ( 'NONE',  ( -113.0660165063659122, -278.2100017788474702, -284.3916475938056578 ) ) ;
#46927 = CARTESIAN_POINT ( 'NONE',  ( -78.73047227620422461, -297.5342251296269183, -332.2964913152691793 ) ) ;
#46928 = CARTESIAN_POINT ( 'NONE',  ( 123.4306832106270946, -178.2391364535880882, 0.000000000000000000 ) ) ;
#46929 = CARTESIAN_POINT ( 'NONE',  ( -110.4542110544635705, -280.8376638359844719, -287.0812184334320705 ) ) ;
#46930 = CARTESIAN_POINT ( 'NONE',  ( -62.41359801023755693, -295.8689833392643322, -198.8649263636822866 ) ) ;
#46931 = CARTESIAN_POINT ( 'NONE',  ( -43.21828445101425586, -276.6360115185968311, -343.1859365431740230 ) ) ;
#46932 = CARTESIAN_POINT ( 'NONE',  ( -35.54854423031162725, -275.2792216778477155, -193.7661167871499401 ) ) ;
#46933 = CIRCLE ( 'NONE', #3096, 1.000000000000000888 ) ;
#46934 = CARTESIAN_POINT ( 'NONE',  ( 29.71876917803477269, -288.8951686610731713, -239.0423142484046366 ) ) ;
#46935 = CARTESIAN_POINT ( 'NONE',  ( -64.00561790569661014, -296.9138414628872624, -341.8575741261659005 ) ) ;
#46936 = CARTESIAN_POINT ( 'NONE',  ( -41.90647906290507763, -296.3134049404910684, -346.8800417321108966 ) ) ;
#46937 = CARTESIAN_POINT ( 'NONE',  ( 32.53132825814162032, -295.2032517806943019, -243.5695460121583267 ) ) ;
#46938 = CARTESIAN_POINT ( 'NONE',  ( -39.73497317003972995, -278.0218940957681184, -195.5532257248924566 ) ) ;
#46939 = CARTESIAN_POINT ( 'NONE',  ( 36.12867188484763403, -283.6272326712789322, -282.3368699507942097 ) ) ;
#46940 = CARTESIAN_POINT ( 'NONE',  ( -67.37839407562766780, -295.7349918527977479, -202.2361494568315550 ) ) ;
#46941 = CARTESIAN_POINT ( 'NONE',  ( -49.86561904497637698, -285.0705581024865864, -345.1366598365087839 ) ) ;
#46942 = CARTESIAN_POINT ( 'NONE',  ( -9.362743454458945180, -285.3469755665719276, -202.5876515215307450 ) ) ;
#46943 = CARTESIAN_POINT ( 'NONE',  ( 169.6770662837093084, 231.1674941253104976, -192.2518117328845904 ) ) ;
#46944 = ORIENTED_EDGE ( 'NONE', *, *, #11778, .F. ) ;
#46945 = CARTESIAN_POINT ( 'NONE',  ( 16.90916867492576614, -286.5190481281735515, -221.4657607458265716 ) ) ;
#46946 = ORIENTED_EDGE ( 'NONE', *, *, #71569, .T. ) ;
#46947 = CARTESIAN_POINT ( 'NONE',  ( -106.7201388501397901, -285.2114947837844738, -303.0432958377926980 ) ) ;
#46948 = CARTESIAN_POINT ( 'NONE',  ( -107.2180051618227310, -273.1681140090341273, -248.9890690553962997 ) ) ;
#46949 = CARTESIAN_POINT ( 'NONE',  ( 28.36588968391163235, -285.8297558394187377, -230.8821231114277737 ) ) ;
#46950 = CARTESIAN_POINT ( 'NONE',  ( -102.9442683331660504, -289.9941773925558550, -230.5372848800695067 ) ) ;
#46951 = CARTESIAN_POINT ( 'NONE',  ( 17.04791332139559401, -281.7454161081065536, -216.1147364500776007 ) ) ;
#46952 = FACE_OUTER_BOUND ( 'NONE', #55962, .T. ) ;
#46953 = CARTESIAN_POINT ( 'NONE',  ( -112.0428259243559239, -280.2695635856457557, -254.7272348855554753 ) ) ;
#46954 = CARTESIAN_POINT ( 'NONE',  ( 38.77316867427907709, -281.7372344245923728, -258.5146077812706835 ) ) ;
#46955 = CARTESIAN_POINT ( 'NONE',  ( 7.399455738971487229, -285.9094976428776249, -326.5171145203363494 ) ) ;
#46956 = CARTESIAN_POINT ( 'NONE',  ( 194.8177507750399400, 278.8342080080603864, -125.9237472059935925 ) ) ;
#46957 = ORIENTED_EDGE ( 'NONE', *, *, #11727, .F. ) ;
#46958 = CARTESIAN_POINT ( 'NONE',  ( 19.72253917211401131, -278.2237576157742751, -318.7729039706862295 ) ) ;
#46959 = CARTESIAN_POINT ( 'NONE',  ( -40.44464271085224993, -139.2070877199659549, -364.2637007583950890 ) ) ;
#46960 = CARTESIAN_POINT ( 'NONE',  ( 3.627343256310792352, -278.6259450273276457, -207.9020939042410134 ) ) ;
#46961 = CARTESIAN_POINT ( 'NONE',  ( 20.60956065430444539, -295.9835890928820277, -319.5101300760515528 ) ) ;
#46962 = CARTESIAN_POINT ( 'NONE',  ( -84.55024615857061576, -295.0708339854741666, -326.2419744307011911 ) ) ;
#46963 = CARTESIAN_POINT ( 'NONE',  ( -105.9463953377612597, -290.5098734150645328, -235.4166268970972453 ) ) ;
#46964 = DIRECTION ( 'NONE',  ( 0.000000000000000000, 0.000000000000000000, 1.000000000000000000 ) ) ;
#46966 = CARTESIAN_POINT ( 'NONE',  ( 1.717907479817098571, -286.9201072494794857, -332.9773097230851135 ) ) ;
#46965 = CARTESIAN_POINT ( 'NONE',  ( -110.2454253371586503, -295.4186315915780483, -247.3023882779304756 ) ) ;
#46967 = CARTESIAN_POINT ( 'NONE',  ( 29.84655285367539435, -294.9917865583138337, -238.6708420628921488 ) ) ;
#46968 = CARTESIAN_POINT ( 'NONE',  ( 7.212683526540816459, -287.9886006751912646, -211.8489868194129997 ) ) ;
#46969 = VERTEX_POINT ( 'NONE', #47603 ) ;
#46970 = CARTESIAN_POINT ( 'NONE',  ( -8.610440935211915559, -293.3603645007340788, -199.1759021136741694 ) ) ;
#46971 = CARTESIAN_POINT ( 'NONE',  ( -105.2688351451556343, -284.6832523746464290, -297.4040598760556122 ) ) ;
#46972 = CARTESIAN_POINT ( 'NONE',  ( -96.21614267100038376, -294.6843027927102980, -319.3897710384776474 ) ) ;
#46973 = CARTESIAN_POINT ( 'NONE',  ( -107.5796045707633937, -290.9550515346834914, -301.6495358087673822 ) ) ;
#46974 = EDGE_CURVE ( 'NONE', #60602, #2535, #54766, .T. ) ;
#46975 = CARTESIAN_POINT ( 'NONE',  ( -92.77210578817116016, -291.7761981067884562, -216.9280578369938723 ) ) ;
#46976 = CARTESIAN_POINT ( 'NONE',  ( -100.3028759983042448, -290.2103514610667503, -307.4050967936290135 ) ) ;
#46977 = VERTEX_POINT ( 'NONE', #4070 ) ;
#46978 = DIRECTION ( 'NONE',  ( -0.000000000000000000, 1.000000000000000000, -0.000000000000000000 ) ) ;
#46979 = CARTESIAN_POINT ( 'NONE',  ( -90.78135383411671455, -299.1642829180493095, -216.6534938395993777 ) ) ;
#46980 = CARTESIAN_POINT ( 'NONE',  ( -113.4663574789698117, -271.4545208574642174, -261.8144659321022232 ) ) ;
#46981 = EDGE_CURVE ( 'NONE', #34296, #4490, #4525, .T. ) ;
#46982 = CARTESIAN_POINT ( 'NONE',  ( -24.03446288130383834, -281.9367339217170070, -342.3772681456105147 ) ) ;
#46983 = CARTESIAN_POINT ( 'NONE',  ( 13.92814348106507438, -274.2561390963737153, -212.9232892548436951 ) ) ;
#46984 = CARTESIAN_POINT ( 'NONE',  ( -107.5355677566599013, -294.7353018575846022, -292.9658994180929881 ) ) ;
#46985 = CARTESIAN_POINT ( 'NONE',  ( -41.90930862228105980, -278.9707065260643049, -344.4684782110286960 ) ) ;
#46986 = CARTESIAN_POINT ( 'NONE',  ( -33.96111872393461795, -272.2347102126651066, -196.2029279331675582 ) ) ;
#46987 = CARTESIAN_POINT ( 'NONE',  ( -52.73325169411006641, -299.0557440639112201, -198.5438408901347600 ) ) ;
#46988 = CARTESIAN_POINT ( 'NONE',  ( -108.7813540979411471, -297.8479139283605832, -253.9111357514047711 ) ) ;
#46989 = CARTESIAN_POINT ( 'NONE',  ( 165.2494399300530290, 8.542400036368780647, 25.74970488511327815 ) ) ;
#46990 = CARTESIAN_POINT ( 'NONE',  ( -70.40059192125617926, -299.2237437361544039, -201.7058188978544422 ) ) ;
#46991 = CARTESIAN_POINT ( 'NONE',  ( -106.5565295716641430, -270.9616159465771830, -240.4347256797260854 ) ) ;
#46992 = CARTESIAN_POINT ( 'NONE',  ( 8.298268712311218209, -295.0602075196611054, -327.5303473707286912 ) ) ;
#46993 = CARTESIAN_POINT ( 'NONE',  ( 0.2253321349396642526, -291.1377977693260277, -207.0832150137832741 ) ) ;
#46994 = FACE_OUTER_BOUND ( 'NONE', #10266, .T. ) ;
#46995 = CARTESIAN_POINT ( 'NONE',  ( 38.15715175967597617, -275.8590810657676684, -255.5472640931754711 ) ) ;
#46996 = CARTESIAN_POINT ( 'NONE',  ( -91.12397300751980822, -273.4274203740927760, -220.9820303778206494 ) ) ;
#46997 = CARTESIAN_POINT ( 'NONE',  ( 36.63506767828697974, -283.3486921252967932, -256.0138314624815621 ) ) ;
#46998 = CARTESIAN_POINT ( 'NONE',  ( -50.02833169424848592, -281.8954793530547818, -345.8622978835057893 ) ) ;
#46999 = CARTESIAN_POINT ( 'NONE',  ( -100.3866959098494505, -277.3179440326601366, -314.3911224516833158 ) ) ;
#47000 = LINE ( 'NONE', #63487, #68660 ) ;
#47001 = CARTESIAN_POINT ( 'NONE',  ( -107.5069076522069764, -284.0250114670508879, -249.4624343582494532 ) ) ;
#47002 = CARTESIAN_POINT ( 'NONE',  ( -93.97073002194308344, -281.8672429092375751, -319.7896664334157322 ) ) ;
#47003 = CARTESIAN_POINT ( 'NONE',  ( 21.29552399324870038, -274.7467529015071932, -314.8251581273250963 ) ) ;
#47004 = CARTESIAN_POINT ( 'NONE',  ( -67.15354586629744915, -281.6616284565767501, -201.4860309758704773 ) ) ;
#47005 = CARTESIAN_POINT ( 'NONE',  ( 175.2296996224750103, 275.0000000000000568, 0.000000000000000000 ) ) ;
#47006 = DIRECTION ( 'NONE',  ( 1.000000000000000000, 0.000000000000000000, 0.000000000000000000 ) ) ;
#47007 = CARTESIAN_POINT ( 'NONE',  ( -38.32642062593526333, -272.4398796970623380, -194.1674781969756509 ) ) ;
#47008 = CIRCLE ( 'NONE', #75753, 2.842139515347646750 ) ;
#47009 = CARTESIAN_POINT ( 'NONE',  ( -111.4337740989455057, -280.7145634918160226, -257.6964820701455210 ) ) ;
#47010 = CARTESIAN_POINT ( 'NONE',  ( 139.1539576904058606, 249.5000000000000568, -10.49999999999999822 ) ) ;
#47011 = CARTESIAN_POINT ( 'NONE',  ( -112.7173390553466419, -286.5484470036557241, -264.3869059452312058 ) ) ;
#47012 = CARTESIAN_POINT ( 'NONE',  ( 156.3938767642171115, 16.40718364543664620, -10.09124105457608245 ) ) ;
#47013 = CARTESIAN_POINT ( 'NONE',  ( 37.47891543908901468, -285.4765352301147914, -264.4846717265897382 ) ) ;
#47014 = DIRECTION ( 'NONE',  ( 0.000000000000000000, 1.000000000000000000, 0.000000000000000000 ) ) ;
#47015 = CARTESIAN_POINT ( 'NONE',  ( -100.5160206574300190, -294.8352570375583923, -307.8261266774889577 ) ) ;
#47016 = CARTESIAN_POINT ( 'NONE',  ( -61.68200203203052467, -287.5114067677779417, -340.4925316464137950 ) ) ;
#47017 = CARTESIAN_POINT ( 'NONE',  ( -90.78337343436103879, -230.3218577325732781, -348.1307343985224634 ) ) ;
#47018 = CARTESIAN_POINT ( 'NONE',  ( -83.14596724027933305, -295.4252801002794513, -210.9070174246385818 ) ) ;
#47019 = CARTESIAN_POINT ( 'NONE',  ( -46.40378332877921252, -284.4190197345153592, -194.5944604093216128 ) ) ;
#47020 = CARTESIAN_POINT ( 'NONE',  ( 19.43869558214458237, -282.4907071640962499, -223.1988870093859703 ) ) ;
#47021 = CARTESIAN_POINT ( 'NONE',  ( -19.18257339715441034, -281.0615910928992207, -344.2003073555125638 ) ) ;
#47022 = CARTESIAN_POINT ( 'NONE',  ( 1.311582375930386180, -288.5199776905834028, -332.2878791740275801 ) ) ;
#47023 = CARTESIAN_POINT ( 'NONE',  ( -71.22902915375870236, -281.0209491235688120, -205.0244547385905776 ) ) ;
#47024 = CARTESIAN_POINT ( 'NONE',  ( -46.48675635365798797, -280.7361043481161005, -197.7222332245394796 ) ) ;
#47025 = CARTESIAN_POINT ( 'NONE',  ( 37.15559972513672449, -289.3860505917339196, -258.9370011673490239 ) ) ;
#47026 = VERTEX_POINT ( 'NONE', #70358 ) ;
#47027 = CARTESIAN_POINT ( 'NONE',  ( -60.87111981962079454, -273.7551671876918249, -196.9885975298930418 ) ) ;
#47028 = CARTESIAN_POINT ( 'NONE',  ( -108.9808215216218059, -292.8038699917130430, -249.3470570570178495 ) ) ;
#47029 = DIRECTION ( 'NONE',  ( 0.000000000000000000, -1.000000000000000000, 0.000000000000000000 ) ) ;
#47030 = CARTESIAN_POINT ( 'NONE',  ( 39.58706461736021254, -290.0519495502703080, -270.3284710469133074 ) ) ;
#47031 = ORIENTED_EDGE ( 'NONE', *, *, #21095, .F. ) ;
#47032 = EDGE_CURVE ( 'NONE', #23241, #34073, #42088, .T. ) ;
#47033 = CARTESIAN_POINT ( 'NONE',  ( 18.49778037380008300, -274.2519160745908380, -320.6991646455864498 ) ) ;
#47034 = EDGE_CURVE ( 'NONE', #77282, #16610, #90665, .T. ) ;
#47035 = CARTESIAN_POINT ( 'NONE',  ( 175.2296996224750103, 276.0000000000000568, 0.000000000000000000 ) ) ;
#47036 = CARTESIAN_POINT ( 'NONE',  ( -85.90133934816454087, -294.1119703109618513, -329.0842126918170152 ) ) ;
#47037 = CARTESIAN_POINT ( 'NONE',  ( -81.12543524878962842, -272.7882670244369478, -211.7580701082218582 ) ) ;
#47038 = CARTESIAN_POINT ( 'NONE',  ( -108.3891023910953919, -291.8139158061215426, -290.1187138804352799 ) ) ;
#47039 = CARTESIAN_POINT ( 'NONE',  ( -45.73239137491702877, -284.9199658065680865, -343.9490024771080243 ) ) ;
#47040 = CARTESIAN_POINT ( 'NONE',  ( -111.6851506909061129, -291.7542241589767400, -288.0708758724734366 ) ) ;
#47041 = CARTESIAN_POINT ( 'NONE',  ( -109.0177512386438963, -292.2095821832967317, -243.4548305301497919 ) ) ;
#47042 = CARTESIAN_POINT ( 'NONE',  ( 17.07915138694823654, -294.0816774226379380, -319.0355997970497697 ) ) ;
#47043 = CARTESIAN_POINT ( 'NONE',  ( -30.37006322470126918, -288.1403637804345408, -195.6336520173842075 ) ) ;
#47044 = CARTESIAN_POINT ( 'NONE',  ( 4.547477976340775108, -282.6706721715551112, -335.0329348870571948 ) ) ;
#47045 = CARTESIAN_POINT ( 'NONE',  ( -108.4866263536419808, -294.9593919667693172, -244.9108985521590114 ) ) ;
#47046 = CARTESIAN_POINT ( 'NONE',  ( -61.23368828972838429, -283.1872046948417392, -343.6163446926947245 ) ) ;
#47047 = CARTESIAN_POINT ( 'NONE',  ( 20.47116220953870780, -278.1860270779059192, -317.5990592484021136 ) ) ;
#47048 = CARTESIAN_POINT ( 'NONE',  ( -92.08974858914540107, -293.6948066931273047, -226.7417163044926838 ) ) ;
#47049 = CARTESIAN_POINT ( 'NONE',  ( -112.9998279212854015, -276.6406517938480079, -274.3802194925361846 ) ) ;
#47050 = PLANE ( 'NONE',  #7621 ) ;
#47051 = CARTESIAN_POINT ( 'NONE',  ( -34.85071812533317370, -282.5277058291583216, -343.3926273606829227 ) ) ;
#47052 = CARTESIAN_POINT ( 'NONE',  ( -104.4531380688512030, -280.2380577036137765, -233.4278861294972103 ) ) ;
#47053 = CARTESIAN_POINT ( 'NONE',  ( 2.628757674676041933, -285.6331815795425655, -204.8234744806161700 ) ) ;
#47054 = CARTESIAN_POINT ( 'NONE',  ( -5.627472017059326426, -294.2352124802760045, -203.4727743469865118 ) ) ;
#47055 = CARTESIAN_POINT ( 'NONE',  ( 0.7773851988820995595, -276.1517640811136971, -204.3658774473878168 ) ) ;
#47056 = CARTESIAN_POINT ( 'NONE',  ( 17.72294824480497866, -276.1346321005822233, -217.1702791299086073 ) ) ;
#47057 = CARTESIAN_POINT ( 'NONE',  ( -37.81189010033128284, -276.8914866397913102, -343.3720566061695649 ) ) ;
#47058 = CARTESIAN_POINT ( 'NONE',  ( -68.84189627889301732, -299.6372711097631623, -202.4665806840606876 ) ) ;
#47059 = CARTESIAN_POINT ( 'NONE',  ( -101.1598074412561346, -283.0784820371161459, -231.1820421061018180 ) ) ;
#47060 = CARTESIAN_POINT ( 'NONE',  ( 33.30667356818824487, -292.8292079152202518, -239.7906815199799269 ) ) ;
#47061 = CARTESIAN_POINT ( 'NONE',  ( -105.7858829580553959, -291.7162770810338088, -303.9747858199236248 ) ) ;
#47062 = CARTESIAN_POINT ( 'NONE',  ( -3.481310526433006203, -291.4305545795600096, -205.3403513735555919 ) ) ;
#47063 = ORIENTED_EDGE ( 'NONE', *, *, #33369, .T. ) ;
#47064 = CARTESIAN_POINT ( 'NONE',  ( -37.77334838268598105, -290.6215795207753558, -193.9515637679012059 ) ) ;
#47065 = CARTESIAN_POINT ( 'NONE',  ( -6.028715400097473420, -292.1421290203160197, -204.3807910971478918 ) ) ;
#47066 = ORIENTED_EDGE ( 'NONE', *, *, #73502, .T. ) ;
#47067 = CARTESIAN_POINT ( 'NONE',  ( -73.01782587618470188, -290.5933111271570510, -338.2632691896680512 ) ) ;
#47068 = CARTESIAN_POINT ( 'NONE',  ( -108.0733132660293876, -279.4475922210236263, -251.8475943923816374 ) ) ;
#47069 = CARTESIAN_POINT ( 'NONE',  ( -57.29598324438435952, -296.7209759230235022, -196.2566271848827739 ) ) ;
#47070 = CARTESIAN_POINT ( 'NONE',  ( -68.46711259473553923, -286.3052545824558592, -200.0294683858754183 ) ) ;
#47071 = CARTESIAN_POINT ( 'NONE',  ( 34.83293126133888507, -287.5469013258806967, -243.5923511961041754 ) ) ;
#47072 = CARTESIAN_POINT ( 'NONE',  ( -108.6864749445183946, -285.0913634823190250, -254.7460366052251572 ) ) ;
#47073 = CARTESIAN_POINT ( 'NONE',  ( -114.0438498157189002, -273.6021558389782058, -270.3744870444270418 ) ) ;
#47074 = CARTESIAN_POINT ( 'NONE',  ( -64.84513123375332100, -181.9241928666178012, -360.8394250873944884 ) ) ;
#47075 = CARTESIAN_POINT ( 'NONE',  ( -48.11459895883137960, -154.8715929890281018, -361.3444938967305120 ) ) ;
#47076 = PRESENTATION_LAYER_ASSIGNMENT (  '', '', ( #18373 ) ) ;
#47077 = CARTESIAN_POINT ( 'NONE',  ( 35.54004119667265371, -274.6578938696477508, -263.4155625949403543 ) ) ;
#47078 = CARTESIAN_POINT ( 'NONE',  ( 24.23659503619849431, -275.0219747546571512, -310.2333248977112703 ) ) ;
#47079 = CARTESIAN_POINT ( 'NONE',  ( -102.2611045658888997, -296.6014632875123311, -229.0694986076424016 ) ) ;
#47080 = CARTESIAN_POINT ( 'NONE',  ( 194.3800462488992764, 275.6740546377429837, -124.2862691682898912 ) ) ;
#47081 = CARTESIAN_POINT ( 'NONE',  ( 15.69729037477889477, -273.4690764703283321, -215.2234379593620872 ) ) ;
#47082 = CARTESIAN_POINT ( 'NONE',  ( -62.39347726987958254, -275.4818730019001691, -200.7164306406782259 ) ) ;
#47083 = ORIENTED_EDGE ( 'NONE', *, *, #909, .F. ) ;
#47084 = CARTESIAN_POINT ( 'NONE',  ( -112.1448397258379259, -273.8441659360954645, -253.4500914685297630 ) ) ;
#47085 = AXIS2_PLACEMENT_3D ( 'NONE', #93161, #28314, #41554 ) ;
#47086 = CARTESIAN_POINT ( 'NONE',  ( -86.76639950507839671, -290.2539334107912623, -324.2366916710582814 ) ) ;
#47087 = CARTESIAN_POINT ( 'NONE',  ( -113.4911810375529058, -297.2214278826049281, -281.0176193153636746 ) ) ;
#47088 = CARTESIAN_POINT ( 'NONE',  ( -87.42695835512067504, -297.8678430461726521, -211.8871664294761956 ) ) ;
#47089 = CARTESIAN_POINT ( 'NONE',  ( -31.60023773765314914, -295.1444758661645551, -343.1850974472641838 ) ) ;
#47090 = ORIENTED_EDGE ( 'NONE', *, *, #50938, .F. ) ;
#47091 = CARTESIAN_POINT ( 'NONE',  ( 2.758408817152785630, -278.4392578322497229, -334.4640773364017150 ) ) ;
#47092 = CARTESIAN_POINT ( 'NONE',  ( -6.249483265708501101, -279.9574497234660839, -199.9707174285328506 ) ) ;
#47093 = CARTESIAN_POINT ( 'NONE',  ( -87.24714235409743424, -278.7098920521756895, -323.9601411440245329 ) ) ;
#47094 = CARTESIAN_POINT ( 'NONE',  ( 2.982998827523904772, -278.2792707822525813, -334.8272022141157436 ) ) ;
#47095 = CARTESIAN_POINT ( 'NONE',  ( -94.66489187455550791, -273.6831936119405668, -225.0616684287499254 ) ) ;
#47096 = CARTESIAN_POINT ( 'NONE',  ( -73.11759151502221243, -296.1426784653517075, -206.0535716657066416 ) ) ;
#47097 = CARTESIAN_POINT ( 'NONE',  ( 151.9826577741344522, 20.03748314401282471, -9.225496140113904175 ) ) ;
#47098 = CARTESIAN_POINT ( 'NONE',  ( -110.1587953022172712, -278.7869597853193682, -265.1967540440379025 ) ) ;
#47099 = CARTESIAN_POINT ( 'NONE',  ( 15.90775751242345670, -275.5867418297112295, -214.9656842252709623 ) ) ;
#47100 = CARTESIAN_POINT ( 'NONE',  ( 19.24812447804917781, -286.9414441284055215, -321.8674212866099538 ) ) ;
#47101 = CARTESIAN_POINT ( 'NONE',  ( -41.11822994884737170, -276.0049114319845103, -195.4053537863085808 ) ) ;
#47102 = CARTESIAN_POINT ( 'NONE',  ( 201.2104617360081704, 60.19600395700749829, -9.000000000000000000 ) ) ;
#47103 = CARTESIAN_POINT ( 'NONE',  ( -108.8226826575141928, -289.5433933827991950, -286.0101253852195669 ) ) ;
#47104 = CARTESIAN_POINT ( 'NONE',  ( -103.9480126313587647, -284.4022051548209902, -231.8246337239282013 ) ) ;
#47105 = CARTESIAN_POINT ( 'NONE',  ( 29.90259401685330332, -279.3791176051769298, -239.3160701446660994 ) ) ;
#47107 = CARTESIAN_POINT ( 'NONE',  ( -55.07615895754810253, -283.9023055931288013, -198.0111594346907395 ) ) ;
#47106 = CARTESIAN_POINT ( 'NONE',  ( 30.57220201244553337, -279.7497886464838643, -242.0225080704779828 ) ) ;
#47108 = CARTESIAN_POINT ( 'NONE',  ( -4.615593536979407219, -290.6212791180838053, -337.8584503209099807 ) ) ;
#47109 = CARTESIAN_POINT ( 'NONE',  ( -108.9977426909084528, -279.9664205971453157, -254.4119552648612625 ) ) ;
#47110 = CARTESIAN_POINT ( 'NONE',  ( 154.4002551233161000, 19.39818217137391443, -12.47984618067382634 ) ) ;
#47111 = CARTESIAN_POINT ( 'NONE',  ( -39.18865352187957996, -294.0291617488275051, -195.3711623932291559 ) ) ;
#47112 = CARTESIAN_POINT ( 'NONE',  ( -97.75686792767474742, -277.4148497394630795, -224.2532558495760497 ) ) ;
#47113 = CARTESIAN_POINT ( 'NONE',  ( 0.9318544525416424529, -277.1785558957761282, -332.7024417860861263 ) ) ;
#47114 = CARTESIAN_POINT ( 'NONE',  ( -37.28933217341737816, -285.0516177149982582, -345.5405253696986279 ) ) ;
#47115 = CARTESIAN_POINT ( 'NONE',  ( 199.4392256788250961, 65.82574266882504332, 7.741079165001063522 ) ) ;
#47116 = CARTESIAN_POINT ( 'NONE',  ( -112.2421295699888759, -292.6041609144544964, -260.0152238140716463 ) ) ;
#47117 = CARTESIAN_POINT ( 'NONE',  ( -102.8913616717953516, -294.0657646029418402, -306.9117459754523907 ) ) ;
#47118 = CARTESIAN_POINT ( 'NONE',  ( 39.41692945656124891, -286.6926358324863031, -265.8381145829597472 ) ) ;
#47119 = CARTESIAN_POINT ( 'NONE',  ( -57.85800909566775374, -290.1827263545806090, -199.4167535430180749 ) ) ;
#47120 = CARTESIAN_POINT ( 'NONE',  ( 208.6208076322478746, 32.98517505407394168, 13.99999999999999822 ) ) ;
#47121 = CARTESIAN_POINT ( 'NONE',  ( -24.25815183867002389, -275.5665616661739818, -342.7320977899362902 ) ) ;
#47122 = CARTESIAN_POINT ( 'NONE',  ( -10.05769737431661426, -292.8316759633332254, -339.4005898417319145 ) ) ;
#47123 = FILL_AREA_STYLE ('',( #68467 ) ) ;
#47124 = CARTESIAN_POINT ( 'NONE',  ( 197.5007179652673415, 41.86699982721680868, 12.19591313108007036 ) ) ;
#47125 = CARTESIAN_POINT ( 'NONE',  ( -69.31482710721708429, -290.1189892909160335, -201.0617937484004756 ) ) ;
#47126 = CARTESIAN_POINT ( 'NONE',  ( -27.75256220885212599, -287.7760919578826133, -197.1867450913030382 ) ) ;
#47127 = CARTESIAN_POINT ( 'NONE',  ( -34.72446953642129586, -287.2595518301836819, -346.3027015835333486 ) ) ;
#47128 = CARTESIAN_POINT ( 'NONE',  ( -88.11405299361572929, -286.7497372199761116, -217.0925240394139450 ) ) ;
#47129 = CARTESIAN_POINT ( 'NONE',  ( 153.5035891336125360, 20.65792664182377791, -10.22121553831927088 ) ) ;
#47130 = CARTESIAN_POINT ( 'NONE',  ( -35.94060436001419845, -286.8730058873092048, -197.2130581441678032 ) ) ;
#47131 = CARTESIAN_POINT ( 'NONE',  ( 20.92115485456609747, -294.8762410942761107, -222.5715109931754796 ) ) ;
#47132 = CARTESIAN_POINT ( 'NONE',  ( -111.8826778263785400, -276.4743791852865797, -282.7286902134890738 ) ) ;
#47133 = AXIS2_PLACEMENT_3D ( 'NONE', #8342, #73683, #794 ) ;
#47134 = CARTESIAN_POINT ( 'NONE',  ( -89.19474017715236869, -278.0916778851050708, -327.2558148278662884 ) ) ;
#47135 = AXIS2_PLACEMENT_3D ( 'NONE', #5834, #56506, #85364 ) ;
#47136 = CARTESIAN_POINT ( 'NONE',  ( -73.95923529058131862, -289.6494777270734176, -204.2667133945505782 ) ) ;
#47137 = CARTESIAN_POINT ( 'NONE',  ( -109.7367621446333175, -278.2191181191696501, -296.7459905918261143 ) ) ;
#47138 = CARTESIAN_POINT ( 'NONE',  ( -82.96900631644514590, -299.4046923507244173, -211.2194067983151342 ) ) ;
#47139 = CARTESIAN_POINT ( 'NONE',  ( -48.18343439341874301, -255.4808422879580121, -493.8826162444244119 ) ) ;
#47140 = CARTESIAN_POINT ( 'NONE',  ( -112.2234160870243755, -282.6168989381570213, -265.3056901342445144 ) ) ;
#47141 = CARTESIAN_POINT ( 'NONE',  ( -48.18343439339133738, -253.7029054207300476, -479.0169286797111567 ) ) ;
#47142 = CARTESIAN_POINT ( 'NONE',  ( -104.4769649845768242, -277.1141253953377941, -238.5588094975017839 ) ) ;
#47143 = ADVANCED_FACE ( 'NONE', ( #79326 ), #78380, .F. ) ;
#47144 = CARTESIAN_POINT ( 'NONE',  ( 36.17980464814537811, -279.7422620177828776, -285.1796532502651758 ) ) ;
#47145 = EDGE_CURVE ( 'NONE', #71226, #15778, #80231, .T. ) ;
#47146 = CARTESIAN_POINT ( 'NONE',  ( -35.74559636889907921, -275.5123879625615473, -346.6640981007853384 ) ) ;
#47147 = AXIS2_PLACEMENT_3D ( 'NONE', #53320, #61842, #40952 ) ;
#47148 = CARTESIAN_POINT ( 'NONE',  ( -107.5236829127419327, -297.7750554325476173, -293.0027641199662298 ) ) ;
#47149 = CARTESIAN_POINT ( 'NONE',  ( -74.13980196493383801, -282.4493524272839409, -337.7062748260351555 ) ) ;
#47150 = CARTESIAN_POINT ( 'NONE',  ( -60.60195323911070631, -298.6842837270797872, -200.8641937631643941 ) ) ;
#47151 = CARTESIAN_POINT ( 'NONE',  ( -113.1156854297965992, -298.0014884745592099, -259.7020454363106978 ) ) ;
#47152 = CARTESIAN_POINT ( 'NONE',  ( -40.77168706947929877, -273.6746789753167945, -197.3708606759422821 ) ) ;
#47153 = CARTESIAN_POINT ( 'NONE',  ( 14.26127856995982057, -294.7774907186017117, -215.9356346469230346 ) ) ;
#47154 = CARTESIAN_POINT ( 'NONE',  ( -2.224799869616333581, -286.6706045093060311, -201.8204337911280675 ) ) ;
#47155 = CARTESIAN_POINT ( 'NONE',  ( 23.36354274383952401, -274.3046820923499922, -315.6951997626322850 ) ) ;
#47156 = CARTESIAN_POINT ( 'NONE',  ( -9.565311140439558102, -288.5323722803806845, -342.1766610029550293 ) ) ;
#47157 = CARTESIAN_POINT ( 'NONE',  ( 35.35634138105455548, -286.7273266253073416, -279.2156766240199204 ) ) ;
#47158 = CARTESIAN_POINT ( 'NONE',  ( -112.2548800659922676, -288.5056641619256084, -273.9689036732924023 ) ) ;
#47159 = VERTEX_POINT ( 'NONE', #36674 ) ;
#47160 = CARTESIAN_POINT ( 'NONE',  ( -71.74250447947856912, -195.9422791308210492, -360.7315132586310824 ) ) ;
#47161 = CARTESIAN_POINT ( 'NONE',  ( 22.00802344034511648, -287.6549668630858037, -312.9709613772907346 ) ) ;
#47162 = DIRECTION ( 'NONE',  ( 0.000000000000000000, 0.000000000000000000, -1.000000000000000000 ) ) ;
#47163 = CARTESIAN_POINT ( 'NONE',  ( -102.3256864906119290, -286.0301347428381860, -229.4966868831272109 ) ) ;
#47164 = CARTESIAN_POINT ( 'NONE',  ( 22.03490634339488707, -291.9555696385959891, -221.7068394665944311 ) ) ;
#47165 = CARTESIAN_POINT ( 'NONE',  ( -11.79693778787579816, -281.9792547514335297, -198.5150174740892339 ) ) ;
#47166 = CARTESIAN_POINT ( 'NONE',  ( 30.27805885086473836, -282.4008973034112273, -234.4590241448295842 ) ) ;
#47167 = CARTESIAN_POINT ( 'NONE',  ( -78.37838197559871389, -283.4550003757768764, -330.7348767477325282 ) ) ;
#47168 = CARTESIAN_POINT ( 'NONE',  ( 4.264197598525720778, -278.4913503183393004, -332.7626397683217192 ) ) ;
#47169 = CARTESIAN_POINT ( 'NONE',  ( -109.8508619828462400, -296.8792365744756125, -244.4493166727415030 ) ) ;
#47170 = CARTESIAN_POINT ( 'NONE',  ( -34.03513793910386909, -275.4097870147164144, -196.9423865484524754 ) ) ;
#47171 = CARTESIAN_POINT ( 'NONE',  ( -73.39986577598109818, -289.5918865061569818, -204.9451402227256267 ) ) ;
#47172 = CARTESIAN_POINT ( 'NONE',  ( -86.29654150467598583, -296.2737638410041541, -215.7932741674931094 ) ) ;
#47173 = ORIENTED_EDGE ( 'NONE', *, *, #26543, .F. ) ;
#47174 = DIRECTION ( 'NONE',  ( 0.000000000000000000, 0.000000000000000000, 1.000000000000000000 ) ) ;
#47175 = CARTESIAN_POINT ( 'NONE',  ( -111.4301104290268825, -286.5723994601119102, -262.6242205531833633 ) ) ;
#47176 = CARTESIAN_POINT ( 'NONE',  ( 27.85044064430050526, -295.1633034322525191, -310.8524654708133426 ) ) ;
#47177 = CARTESIAN_POINT ( 'NONE',  ( -108.5226542122557305, -284.9836001232575313, -287.0640393276780742 ) ) ;
#47178 = CARTESIAN_POINT ( 'NONE',  ( 20.63464958603786314, -275.2931151349641823, -320.6956497394458552 ) ) ;
#47179 = CARTESIAN_POINT ( 'NONE',  ( -50.55700361745870453, -292.5390305648504068, -194.6071178242516169 ) ) ;
#47180 = CARTESIAN_POINT ( 'NONE',  ( -111.0235649003089264, -282.4667926742456530, -288.0594715057580970 ) ) ;
#47181 = CARTESIAN_POINT ( 'NONE',  ( -53.38905477198330374, -292.1851602701935917, -195.0190081488170506 ) ) ;
#47182 = CARTESIAN_POINT ( 'NONE',  ( -37.26373621707863037, -289.3844316427937429, -343.3822204702021850 ) ) ;
#47183 = LINE ( 'NONE', #48125, #68613 ) ;
#47184 = DIRECTION ( 'NONE',  ( -1.000000000000000000, 0.000000000000000000, 0.000000000000000000 ) ) ;
#47185 = CARTESIAN_POINT ( 'NONE',  ( -110.8432946575179585, -271.2105112503826376, -270.3440356799262645 ) ) ;
#47186 = CARTESIAN_POINT ( 'NONE',  ( -113.6475361307806935, -286.0767731276364430, -270.0045470763440107 ) ) ;
#47187 = CARTESIAN_POINT ( 'NONE',  ( -106.6662871844225293, -293.6237833571632336, -303.7098442033569086 ) ) ;
#47188 = CARTESIAN_POINT ( 'NONE',  ( 27.12035354289720956, -280.9468365232679048, -305.2734325618674802 ) ) ;
#47189 = CARTESIAN_POINT ( 'NONE',  ( 16.93730589883815085, -275.9714655962019947, -325.0206520257424359 ) ) ;
#47190 = CARTESIAN_POINT ( 'NONE',  ( -105.0389662326316227, -280.9740806421274897, -238.3470921048167952 ) ) ;
#47191 = CARTESIAN_POINT ( 'NONE',  ( -10.83832046195042942, -93.09808498907607088, -357.9296412820179398 ) ) ;
#47192 = CARTESIAN_POINT ( 'NONE',  ( -94.90291095533092403, -282.4420381907338538, -320.6136134625443788 ) ) ;
#47193 = CARTESIAN_POINT ( 'NONE',  ( -111.5099796081230181, -282.4578481200293822, -279.2292867579384961 ) ) ;
#47194 = CARTESIAN_POINT ( 'NONE',  ( -9.594216685023646107, -300.1551415047837850, -194.3662611768685906 ) ) ;
#47195 = CARTESIAN_POINT ( 'NONE',  ( -72.14837848031922363, -296.0180212675554117, -334.6131099744407607 ) ) ;
#47196 = VERTEX_POINT ( 'NONE', #29594 ) ;
#47197 = CARTESIAN_POINT ( 'NONE',  ( 2.521963754546275638, -291.2833017870509025, -208.5583619379495701 ) ) ;
#47198 = CARTESIAN_POINT ( 'NONE',  ( 36.78957282834523568, -276.4605359260473847, -290.8520351895751332 ) ) ;
#47199 = CARTESIAN_POINT ( 'NONE',  ( -24.59643370986773903, -274.2192078372899573, -198.4307552523208642 ) ) ;
#47200 = CARTESIAN_POINT ( 'NONE',  ( 22.39154968962667880, -275.1199348831720499, -318.4800282412595038 ) ) ;
#47201 = CARTESIAN_POINT ( 'NONE',  ( 194.5881128153457098, -26.00396092263537540, 10.00000000000000178 ) ) ;
#47202 = CARTESIAN_POINT ( 'NONE',  ( -89.03795467839073297, -271.3257309467421692, -215.9538867083872447 ) ) ;
#47203 = CARTESIAN_POINT ( 'NONE',  ( -41.89218676549776177, -296.5335659507661035, -346.6882666136403373 ) ) ;
#47204 = CARTESIAN_POINT ( 'NONE',  ( 222.8344101925596306, 0.000000000000000000, -7.000000000000000888 ) ) ;
#47205 = B_SPLINE_CURVE_WITH_KNOTS ( 'NONE', 3,
 ( #19878, #39754, #48749, #77653, #41646, #5688, #13727, #85211 ),
 .UNSPECIFIED., .F., .F.,
 ( 4, 2, 2, 4 ),
 ( 0.000000000000000000, 0.0008360664702759048076, 0.001672132940551809615, 0.003344265881103569357 ),
 .UNSPECIFIED. ) ;
#47206 = VECTOR ( 'NONE', #17684, 1000.000000000000000 ) ;
#47207 = CARTESIAN_POINT ( 'NONE',  ( 2.197429475817664013, -229.5268262511776527, -22.50000000000000000 ) ) ;
#47208 = VECTOR ( 'NONE', #51465, 999.9999999999998863 ) ;
#47209 = CARTESIAN_POINT ( 'NONE',  ( -13.41554291714954950, -283.8138374632072214, -339.7097227638931258 ) ) ;
#47210 = CARTESIAN_POINT ( 'NONE',  ( 37.43248178429178097, -283.4845499658496237, -283.9537036214402406 ) ) ;
#47211 = CARTESIAN_POINT ( 'NONE',  ( -107.0855911612821956, -283.6108530795273737, -292.2627693309453321 ) ) ;
#47212 = CARTESIAN_POINT ( 'NONE',  ( 1.272834650735972462, -274.9273772703353416, -333.3127936274298690 ) ) ;
#47213 = CARTESIAN_POINT ( 'NONE',  ( 6.337672445789625186, -284.3122010144008414, -330.3859285969235771 ) ) ;
#47214 = CARTESIAN_POINT ( 'NONE',  ( -62.04026454272535318, -275.8589174673692241, -339.8465540622723893 ) ) ;
#47215 = CIRCLE ( 'NONE', #35147, 0.4999999999999938938 ) ;
#47216 = CARTESIAN_POINT ( 'NONE',  ( 20.08911706048522561, -275.9911781487510893, -224.7786915983855351 ) ) ;
#47217 = FACE_OUTER_BOUND ( 'NONE', #27154, .T. ) ;
#47218 = VECTOR ( 'NONE', #68473, 999.9999999999998863 ) ;
#47219 = CARTESIAN_POINT ( 'NONE',  ( -112.8394405884124865, -279.5349754866853687, -255.9990956565135889 ) ) ;
#47220 = ORIENTED_EDGE ( 'NONE', *, *, #16696, .T. ) ;
#47221 = CARTESIAN_POINT ( 'NONE',  ( 199.4949018615358511, 17.05867184936851899, 10.28330198088169212 ) ) ;
#47222 = CARTESIAN_POINT ( 'NONE',  ( -110.6733569989350059, -286.1696982874262289, -289.4591053198163308 ) ) ;
#47223 = CARTESIAN_POINT ( 'NONE',  ( -71.01419933998907652, -294.7055366935867369, -335.3271511601451493 ) ) ;
#47224 = CARTESIAN_POINT ( 'NONE',  ( -112.8233061686552077, -290.0855815693317368, -255.6010678277281727 ) ) ;
#47225 = CARTESIAN_POINT ( 'NONE',  ( 29.73767984930548280, -285.3754527291678755, -239.0828380946817902 ) ) ;
#47227 = CARTESIAN_POINT ( 'NONE',  ( -109.0852771559119674, -289.0293905106826173, -252.1208167930734589 ) ) ;
#47226 = CARTESIAN_POINT ( 'NONE',  ( 19.98555534489466012, -285.4795617971160482, -224.2004850895096979 ) ) ;
#47228 = CARTESIAN_POINT ( 'NONE',  ( -108.8084297621258543, -285.5371730028592765, -287.1383326504704314 ) ) ;
#47229 = CARTESIAN_POINT ( 'NONE',  ( 37.38555868714419006, -273.6340407210270200, -276.7515355555096335 ) ) ;
#47230 = CARTESIAN_POINT ( 'NONE',  ( 38.84068377116534521, -285.9313171855880569, -268.7225830092211822 ) ) ;
#47231 = CARTESIAN_POINT ( 'NONE',  ( 37.53100599718245434, -285.4597184642306615, -263.1588784501709029 ) ) ;
#47232 = CARTESIAN_POINT ( 'NONE',  ( 27.98587816216208424, -282.0440598634750131, -237.1471077708655173 ) ) ;
#47233 = CARTESIAN_POINT ( 'NONE',  ( -43.01782751543093752, -291.1238205177603504, -345.3131693545683447 ) ) ;
#47234 = LINE ( 'NONE', #25937, #30773 ) ;
#47235 = CARTESIAN_POINT ( 'NONE',  ( 195.4781563537916043, 39.36132622696000283, 14.00000000000000000 ) ) ;
#47236 = CARTESIAN_POINT ( 'NONE',  ( -61.11486860875385219, -297.2784201850321324, -342.1385420411614291 ) ) ;
#47237 = CARTESIAN_POINT ( 'NONE',  ( -21.75454244161035433, -278.2516332032158175, -196.9454404879627418 ) ) ;
#47238 = CARTESIAN_POINT ( 'NONE',  ( 26.36476417200979583, -292.1810160919434907, -227.3065301838002767 ) ) ;
#47239 = CARTESIAN_POINT ( 'NONE',  ( -103.4942067497565148, -294.5120006437263100, -303.1918945326826815 ) ) ;
#47240 = CARTESIAN_POINT ( 'NONE',  ( 7.456095199235232229, -279.3622530651644524, -212.0352293784813185 ) ) ;
#47241 = CARTESIAN_POINT ( 'NONE',  ( 35.53605300513926579, -273.4349377660291225, -255.1281866929532782 ) ) ;
#47242 = CARTESIAN_POINT ( 'NONE',  ( 32.82257019504893947, -295.1551674660261710, -292.2293288893948215 ) ) ;
#47243 = CARTESIAN_POINT ( 'NONE',  ( -20.19161114001083490, -297.3376638359845288, -345.3538533559490702 ) ) ;
#47244 = CARTESIAN_POINT ( 'NONE',  ( -35.47338832949255050, -296.5550266624689471, -194.0549192838901718 ) ) ;
#47245 = CARTESIAN_POINT ( 'NONE',  ( -33.50867054411274637, -293.2444201040388521, -346.2639976651822167 ) ) ;
#47246 = CARTESIAN_POINT ( 'NONE',  ( 17.16247376825644366, -294.2739021256037972, -220.8427991493268507 ) ) ;
#47247 = EDGE_CURVE ( 'NONE', #27568, #26249, #43653, .T. ) ;
#47248 = DIRECTION ( 'NONE',  ( -0.000000000000000000, -0.000000000000000000, -1.000000000000000000 ) ) ;
#47249 = CARTESIAN_POINT ( 'NONE',  ( 24.98007436116651903, -293.8267322415183003, -231.9426701240216744 ) ) ;
#47251 = CARTESIAN_POINT ( 'NONE',  ( -67.29520944067623134, -295.4562114322068851, -336.9464943259771985 ) ) ;
#47250 = CARTESIAN_POINT ( 'NONE',  ( -6.159652433930307147, -280.6645610799988049, -338.9620415035131487 ) ) ;
#47252 = CARTESIAN_POINT ( 'NONE',  ( -37.31425204684190078, -283.0517811524608760, -347.3741783324445578 ) ) ;
#47253 = CARTESIAN_POINT ( 'NONE',  ( -114.3053226495254080, -284.2595292315277220, -267.1110651571665358 ) ) ;
#47254 = CARTESIAN_POINT ( 'NONE',  ( -93.81153541482309777, -287.8683913136264323, -319.5424193463255733 ) ) ;
#47255 = EDGE_CURVE ( 'NONE', #34296, #64853, #78416, .T. ) ;
#47256 = FACE_OUTER_BOUND ( 'NONE', #42742, .T. ) ;
#47257 = CARTESIAN_POINT ( 'NONE',  ( -19.10304683103889545, -281.3015717310748869, -344.5105118003510825 ) ) ;
#47258 = CARTESIAN_POINT ( 'NONE',  ( -8.362728976432034500, -287.6018775804433290, -341.3803378083374582 ) ) ;
#47259 = CARTESIAN_POINT ( 'NONE',  ( -46.11236658152585477, -296.0521521680024080, -430.6442049081568371 ) ) ;
#47260 = CARTESIAN_POINT ( 'NONE',  ( -84.97912683419076529, -297.3220132842349699, -326.7941103515584018 ) ) ;
#47261 = CARTESIAN_POINT ( 'NONE',  ( -14.74647924161341983, -278.1903711024790482, -343.4100976707210862 ) ) ;
#47262 = CARTESIAN_POINT ( 'NONE',  ( -6.756690381603299045, -280.1317573073408198, -204.0402689355569521 ) ) ;
#47263 = CARTESIAN_POINT ( 'NONE',  ( -34.96253972944582245, -292.2479057605982575, -193.3847325202386571 ) ) ;
#47264 = CARTESIAN_POINT ( 'NONE',  ( -16.56177522502391142, -280.8656932031627207, -343.0618293177664100 ) ) ;
#47265 = CARTESIAN_POINT ( 'NONE',  ( -9.627357516935083126, -291.4819615835115769, -202.5183384911460109 ) ) ;
#47266 = CARTESIAN_POINT ( 'NONE',  ( -112.3662713181513766, -294.5259416601297175, -272.3896070059856243 ) ) ;
#47267 = EDGE_LOOP ( 'NONE', ( #1895, #27823, #78812, #49798 ) ) ;
#47268 = CARTESIAN_POINT ( 'NONE',  ( 200.9103445561496244, 65.54396272403067769, -5.212391550061756362 ) ) ;
#47269 = VECTOR ( 'NONE', #47921, 1000.000000000000000 ) ;
#47270 = CARTESIAN_POINT ( 'NONE',  ( 21.37218548273926189, -293.6689582017637008, -313.8429311725598723 ) ) ;
#47271 = DIRECTION ( 'NONE',  ( 0.000000000000000000, -0.7353190267777791611, -0.6777211291221335587 ) ) ;
#47272 = CARTESIAN_POINT ( 'NONE',  ( -37.37352853689063181, -292.5523547857346784, -340.3611179825599606 ) ) ;
#47273 = CARTESIAN_POINT ( 'NONE',  ( -110.8795906677379151, -272.0316282877120102, -247.9006872612312691 ) ) ;
#47274 = CARTESIAN_POINT ( 'NONE',  ( 36.13918005954949564, -279.4569759122437063, -251.8985685792554250 ) ) ;
#47275 = CARTESIAN_POINT ( 'NONE',  ( -68.31654884858404841, -286.9689080755973691, -200.3907242899047105 ) ) ;
#47276 = CARTESIAN_POINT ( 'NONE',  ( -8.220444392594361105, -288.4933151116125600, -337.3550734263518507 ) ) ;
#47277 = CARTESIAN_POINT ( 'NONE',  ( -110.8516076071489209, -280.1401837666065830, -265.1648449456408798 ) ) ;
#47278 = CARTESIAN_POINT ( 'NONE',  ( -37.16945262842013875, -299.8144870652361078, -196.3448372581566730 ) ) ;
#47279 = CARTESIAN_POINT ( 'NONE',  ( -89.37810487790241609, -276.5996840815217297, -322.1956765249523187 ) ) ;
#47280 = ORIENTED_EDGE ( 'NONE', *, *, #68560, .F. ) ;
#47281 = CARTESIAN_POINT ( 'NONE',  ( -114.3416212705230350, -272.4213605645363145, -267.4915351304622391 ) ) ;
#47282 = CARTESIAN_POINT ( 'NONE',  ( -101.5335610857579240, -291.9635430976080670, -308.1550172619818682 ) ) ;
#47283 = CARTESIAN_POINT ( 'NONE',  ( 21.57758991090565814, -294.4965387587181453, -222.0397181733385992 ) ) ;
#47284 = FACE_OUTER_BOUND ( 'NONE', #47457, .T. ) ;
#47285 = CARTESIAN_POINT ( 'NONE',  ( -109.7227076263855849, -291.0674761955495455, -280.6920631529058028 ) ) ;
#47286 = DIRECTION ( 'NONE',  ( -0.000000000000000000, -0.000000000000000000, -1.000000000000000000 ) ) ;
#47287 = CARTESIAN_POINT ( 'NONE',  ( 33.31955561591752257, -291.3381369091403030, -242.8793666042133168 ) ) ;
#47288 = CARTESIAN_POINT ( 'NONE',  ( -57.38830422467615477, -298.1337010959110216, -195.9830581277876433 ) ) ;
#47289 = CARTESIAN_POINT ( 'NONE',  ( 169.2744399300530347, 8.542400036368780647, 25.74970488511327815 ) ) ;
#47290 = CARTESIAN_POINT ( 'NONE',  ( 195.2949575809873011, 26.08759934769877376, 14.91285779741154016 ) ) ;
#47291 = CARTESIAN_POINT ( 'NONE',  ( -107.7350601565815538, -292.4502854101468188, -240.9080601619868105 ) ) ;
#47292 = CARTESIAN_POINT ( 'NONE',  ( -72.08107566293803359, -294.1233781216987495, -198.2974183793908196 ) ) ;
#47293 = EDGE_CURVE ( 'NONE', #61775, #70030, #40584, .T. ) ;
#47294 = CARTESIAN_POINT ( 'NONE',  ( -111.6912696969639995, -286.4372592251715446, -279.3020659056818999 ) ) ;
#47295 = CARTESIAN_POINT ( 'NONE',  ( 8.472924297440355801, -272.6810440886767424, -211.1914584251230735 ) ) ;
#47296 = CARTESIAN_POINT ( 'NONE',  ( -18.93882080572176108, -276.2109099559589822, -198.1782757031507174 ) ) ;
#47297 = CARTESIAN_POINT ( 'NONE',  ( -5.402030447738578545, -290.5555130453395805, -203.1074028878531976 ) ) ;
#47298 = CARTESIAN_POINT ( 'NONE',  ( -96.94232405863537849, -279.7770074085086662, -317.1379403594822293 ) ) ;
#47299 = VECTOR ( 'NONE', #92948, 1000.000000000000000 ) ;
#47300 = ORIENTED_EDGE ( 'NONE', *, *, #26635, .T. ) ;
#47302 = CARTESIAN_POINT ( 'NONE',  ( 31.44770197111118648, -281.2314993360548669, -295.2475694520865090 ) ) ;
#47301 = CARTESIAN_POINT ( 'NONE',  ( -46.45645791131997271, -279.9334011040078849, -197.8812840090843963 ) ) ;
#47303 = CARTESIAN_POINT ( 'NONE',  ( -25.80285307207096679, -277.9881240492748589, -346.1789754943714001 ) ) ;
#47304 = CARTESIAN_POINT ( 'NONE',  ( 39.13170861255787258, -280.4135515326923951, -275.6488589930308990 ) ) ;
#47305 = CARTESIAN_POINT ( 'NONE',  ( 183.2382489426448444, 261.9115828407970525, -151.4279635117714804 ) ) ;
#47306 = CARTESIAN_POINT ( 'NONE',  ( 4.724172336070187939, -275.5461014643733506, -206.0852640459838767 ) ) ;
#47307 = PRODUCT_CONTEXT ( 'NONE', #2714, 'mechanical' ) ;
#47308 = CARTESIAN_POINT ( 'NONE',  ( -46.81429039673593451, -275.4540674548663901, -194.6446878945457968 ) ) ;
#47309 = CARTESIAN_POINT ( 'NONE',  ( -92.05005921254146983, -280.4090924074130839, -314.0302885647153062 ) ) ;
#47310 = ORIENTED_EDGE ( 'NONE', *, *, #77831, .T. ) ;
#47311 = FACE_OUTER_BOUND ( 'NONE', #57052, .T. ) ;
#47312 = CARTESIAN_POINT ( 'NONE',  ( -23.71428578425187084, -289.9537248085028409, -342.4444172017016399 ) ) ;
#47313 = CARTESIAN_POINT ( 'NONE',  ( 37.11984029285012809, -289.5042570858722115, -285.5088245613155209 ) ) ;
#47314 = CARTESIAN_POINT ( 'NONE',  ( -73.60272487931625562, -288.8955944053112148, -333.8501968845516217 ) ) ;
#47315 = CARTESIAN_POINT ( 'NONE',  ( -10.00995263068972996, -285.9071430336842354, -198.3842487652408977 ) ) ;
#47316 = CARTESIAN_POINT ( 'NONE',  ( 200.0272528223206052, 26.57456426123552617, 9.050802287977962379 ) ) ;
#47317 = CARTESIAN_POINT ( 'NONE',  ( 18.19357468365641495, -280.6380219744269766, -318.9643449126352834 ) ) ;
#47318 = CARTESIAN_POINT ( 'NONE',  ( 23.78014919883603895, -289.9897879115958403, -312.5141052227509135 ) ) ;
#47319 = CARTESIAN_POINT ( 'NONE',  ( -78.78235003413496429, -282.1017764170376836, -331.2986293077425444 ) ) ;
#47320 = CARTESIAN_POINT ( 'NONE',  ( -109.6201222492224758, -280.0416918402560214, -257.0542334995348597 ) ) ;
#47321 = CARTESIAN_POINT ( 'NONE',  ( -48.61115109039207738, -277.6917294630731590, -342.5997224945263042 ) ) ;
#47322 = EDGE_CURVE ( 'NONE', #45887, #21613, #86387, .T. ) ;
#47323 = CARTESIAN_POINT ( 'NONE',  ( -102.8681893677457424, -289.8687932627612440, -230.5815831281811086 ) ) ;
#47324 = CARTESIAN_POINT ( 'NONE',  ( -69.73410099337527868, -286.4392955085043013, -200.6697328347086113 ) ) ;
#47325 = CARTESIAN_POINT ( 'NONE',  ( -37.98822370681094185, -286.5365997589728977, -193.4253726438971626 ) ) ;
#47326 = CARTESIAN_POINT ( 'NONE',  ( -110.3093882375007553, -284.7474822887779169, -268.1893683537275592 ) ) ;
#47327 = VERTEX_POINT ( 'NONE', #50421 ) ;
#47328 = FACE_OUTER_BOUND ( 'NONE', #47512, .T. ) ;
#47329 = CARTESIAN_POINT ( 'NONE',  ( -94.51045356221453630, -291.7295095897889610, -320.0807229001769656 ) ) ;
#47330 = AXIS2_PLACEMENT_3D ( 'NONE', #40133, #39658, #68581 ) ;
#47331 = CARTESIAN_POINT ( 'NONE',  ( 30.45753330345767296, -292.6972775638323583, -305.8091393317166080 ) ) ;
#47332 = CARTESIAN_POINT ( 'NONE',  ( -2.792100925336592265, -273.5795401780071643, -205.7876432151709309 ) ) ;
#47333 = CARTESIAN_POINT ( 'NONE',  ( -58.83080049629687380, -294.6714826667498528, -344.2511044763451196 ) ) ;
#47334 = CARTESIAN_POINT ( 'NONE',  ( -65.57485277101740451, -290.1560276251775576, -202.2769488683008774 ) ) ;
#47335 = CARTESIAN_POINT ( 'NONE',  ( -39.74407791727685435, -293.3225587706272677, -344.3480581158621590 ) ) ;
#47336 = CIRCLE ( 'NONE', #24653, 24.00000000000001066 ) ;
#47337 = CARTESIAN_POINT ( 'NONE',  ( -80.62938103434809989, -290.8587372268113427, -329.6975100401652981 ) ) ;
#47338 = CARTESIAN_POINT ( 'NONE',  ( 128.9467878515196162, -299.5541904835127980, -195.3611179825600175 ) ) ;
#47339 = VECTOR ( 'NONE', #18014, 1000.000000000000114 ) ;
#47340 = CARTESIAN_POINT ( 'NONE',  ( 9.984731590192005513, -290.7018841867899823, -211.8968966108954248 ) ) ;
#47341 = CARTESIAN_POINT ( 'NONE',  ( -31.29466985583038863, -296.9760661300392144, -345.1681882278454623 ) ) ;
#47342 = CARTESIAN_POINT ( 'NONE',  ( 26.56687212397964259, -288.0045184762986423, -234.4928423007621063 ) ) ;
#47343 = CONICAL_SURFACE ( 'NONE', #66982, 6.249455242036738412, 0.09862129276975223346 ) ;
#47344 = CARTESIAN_POINT ( 'NONE',  ( 24.77415395929567055, -276.9564266500975691, -227.6764777438025931 ) ) ;
#47345 = CARTESIAN_POINT ( 'NONE',  ( -31.49596081180238016, -275.7749559887330406, -346.7930225799743766 ) ) ;
#47346 = CARTESIAN_POINT ( 'NONE',  ( -65.47334378413312095, -296.8908782242624511, -198.8006192232170122 ) ) ;
#47347 = CARTESIAN_POINT ( 'NONE',  ( 36.61327719983081863, -273.8444212658760648, -274.3898287576024586 ) ) ;
#47348 = CARTESIAN_POINT ( 'NONE',  ( -93.27458176858496586, -277.3197769015390008, -221.2212000298078465 ) ) ;
#47349 = CARTESIAN_POINT ( 'NONE',  ( -90.49468936121647289, -274.4833408100532779, -219.7276072861770615 ) ) ;
#47350 = CARTESIAN_POINT ( 'NONE',  ( -9.523053172182095238, -275.0944882167575543, -341.3016797020646322 ) ) ;
#47351 = AXIS2_PLACEMENT_3D ( 'NONE', #55074, #47949, #69745 ) ;
#47352 = EDGE_CURVE ( 'NONE', #33107, #34536, #36093, .T. ) ;
#47353 = CARTESIAN_POINT ( 'NONE',  ( 200.2296996224750103, 66.43830042153604154, 2.389358538587006198 ) ) ;
#47354 = CARTESIAN_POINT ( 'NONE',  ( -67.10659532917318870, -274.3027702877292882, -203.5795708894461882 ) ) ;
#47355 = DIRECTION ( 'NONE',  ( -0.000000000000000000, 1.000000000000000000, -0.000000000000000000 ) ) ;
#47357 = CARTESIAN_POINT ( 'NONE',  ( 32.86060664846892365, -275.1186717630363319, -250.1645787173510485 ) ) ;
#47356 = CARTESIAN_POINT ( 'NONE',  ( -12.78409989859064666, -286.7547538235076559, -341.6571463136292550 ) ) ;
#47358 = VECTOR ( 'NONE', #74173, 1000.000000000000000 ) ;
#47359 = CARTESIAN_POINT ( 'NONE',  ( 35.07247007989381160, -287.8844780226338003, -296.6923417897996842 ) ) ;
#47360 = CARTESIAN_POINT ( 'NONE',  ( -80.53226247933328352, -289.2866503103895184, -334.1461522656327361 ) ) ;
#47361 = CARTESIAN_POINT ( 'NONE',  ( 28.95563896395952597, -300.8580694568498757, -194.9836664655143181 ) ) ;
#47362 = CARTESIAN_POINT ( 'NONE',  ( -101.4546696032397364, -295.0712285559720840, -231.6656413759651798 ) ) ;
#47363 = CARTESIAN_POINT ( 'NONE',  ( 37.03293015940866439, -280.9914175798062956, -289.6632730590859524 ) ) ;
#47364 = CARTESIAN_POINT ( 'NONE',  ( -36.09237171215956863, 15.36528803885690664, 21.50000000000000000 ) ) ;
#47365 = CARTESIAN_POINT ( 'NONE',  ( -106.9091457518933197, -276.1851947626889228, -298.5227303991360372 ) ) ;
#47366 = AXIS2_PLACEMENT_3D ( 'NONE', #23666, #52075, #9436 ) ;
#47367 = CARTESIAN_POINT ( 'NONE',  ( 140.6539576904058606, 275.5000000000000568, 10.50000000000000000 ) ) ;
#47368 = CARTESIAN_POINT ( 'NONE',  ( -107.3353889128277245, -289.0538256479035226, -292.6203719295008341 ) ) ;
#47369 = LINE ( 'NONE', #83838, #9441 ) ;
#47370 = DIRECTION ( 'NONE',  ( 0.000000000000000000, 1.000000000000000000, 0.000000000000000000 ) ) ;
#47371 = CARTESIAN_POINT ( 'NONE',  ( -111.6790434902572571, -288.6846530815898859, -260.0290238052101586 ) ) ;
#47372 = CARTESIAN_POINT ( 'NONE',  ( -19.11871989594659738, -275.8109422362250029, -198.9034994426666287 ) ) ;
#47373 = CARTESIAN_POINT ( 'NONE',  ( 39.05077414529836943, -282.9358772276694367, -267.0645545634561699 ) ) ;
#47375 = CARTESIAN_POINT ( 'NONE',  ( -86.92883687992903674, -283.7652306175546073, -324.0037369043731132 ) ) ;
#47374 = CARTESIAN_POINT ( 'NONE',  ( -33.41547829631709732, -296.1211820599642124, -195.0072265337391002 ) ) ;
#47376 = CARTESIAN_POINT ( 'NONE',  ( -59.67157749833192071, -275.1826000562756462, -200.1882128524400741 ) ) ;
#47377 = CARTESIAN_POINT ( 'NONE',  ( 23.92314449272920740, -275.8020554696799422, -230.3708624129477585 ) ) ;
#47378 = CARTESIAN_POINT ( 'NONE',  ( 20.37299723747537428, -286.3015841687665670, -319.1292213796348847 ) ) ;
#47379 = EDGE_CURVE ( 'NONE', #33695, #89141, #7332, .T. ) ;
#47380 = CARTESIAN_POINT ( 'NONE',  ( -30.37464905788779390, -284.9641743501232440, -345.0368225177737713 ) ) ;
#47381 = CARTESIAN_POINT ( 'NONE',  ( -109.4311415970967829, -271.6509713783288475, -256.7729986090099601 ) ) ;
#47382 = ORIENTED_EDGE ( 'NONE', *, *, #14909, .T. ) ;
#47383 = CARTESIAN_POINT ( 'NONE',  ( 204.9610684336733186, 293.7029684379119772, -54.00000000001035971 ) ) ;
#47384 = CARTESIAN_POINT ( 'NONE',  ( 39.60680653321302458, -293.4206848386472188, -273.1766689201677423 ) ) ;
#47385 = CARTESIAN_POINT ( 'NONE',  ( -107.1110617080529863, -286.8785060076702393, -243.8265558891319529 ) ) ;
#47386 = CIRCLE ( 'NONE', #68577, 1.499999999999999556 ) ;
#47387 = ADVANCED_FACE ( 'NONE', ( #44229 ), #64672, .F. ) ;
#47388 = DIRECTION ( 'NONE',  ( 0.000000000000000000, 0.000000000000000000, 1.000000000000000000 ) ) ;
#47389 = CARTESIAN_POINT ( 'NONE',  ( -111.2586520408596868, -270.4809262143062369, -234.7283546768995564 ) ) ;
#47390 = CARTESIAN_POINT ( 'NONE',  ( -103.4720422245554801, -277.2373635576383890, -309.5926677842815593 ) ) ;
#47391 = CARTESIAN_POINT ( 'NONE',  ( -112.0873016528295523, -288.7639433271329494, -285.2440726262187809 ) ) ;
#47392 = CARTESIAN_POINT ( 'NONE',  ( -21.21783944934228217, -284.3618259955413237, -342.3214079021063867 ) ) ;
#47393 = CARTESIAN_POINT ( 'NONE',  ( -100.0214892336160233, -279.7750505408614003, -309.8169143988872065 ) ) ;
#47394 = CARTESIAN_POINT ( 'NONE',  ( -103.5391334409621464, -286.4785562596400723, -232.0916561192736935 ) ) ;
#47395 = CARTESIAN_POINT ( 'NONE',  ( -3.466408484041502813, -282.4994331433874777, -203.4329837190015269 ) ) ;
#47396 = CARTESIAN_POINT ( 'NONE',  ( -0.04730437892725614796, -274.7009416561237458, -202.9804953923291464 ) ) ;
#47397 = CARTESIAN_POINT ( 'NONE',  ( -113.7665136220991116, -278.2627065904239885, -280.1773941270806176 ) ) ;
#47399 = CARTESIAN_POINT ( 'NONE',  ( -80.97954547535800884, -297.5700992779682679, -330.6690996157812492 ) ) ;
#47398 = VECTOR ( 'NONE', #6883, 1000.000000000000000 ) ;
#47400 = DIRECTION ( 'NONE',  ( 1.000000000000000000, 0.000000000000000000, 0.000000000000000000 ) ) ;
#47401 = DIRECTION ( 'NONE',  ( 0.000000000000000000, -0.000000000000000000, 1.000000000000000000 ) ) ;
#47402 = CARTESIAN_POINT ( 'NONE',  ( -20.82146376237103880, -296.3964595977623162, -194.6014795725925524 ) ) ;
#47403 = CARTESIAN_POINT ( 'NONE',  ( 29.14464829593334017, -274.6502850783444956, -239.9475571715804563 ) ) ;
#47404 = VECTOR ( 'NONE', #11265, 1000.000000000000000 ) ;
#47405 = CARTESIAN_POINT ( 'NONE',  ( 7.749300273335740563, -299.6839338148757292, -193.6621707208877012 ) ) ;
#47406 = CARTESIAN_POINT ( 'NONE',  ( -42.77051783036284860, -287.7428939757972444, -196.5343485453171297 ) ) ;
#47407 = CARTESIAN_POINT ( 'NONE',  ( -55.88291227595162525, -296.8068188998313417, -344.3809207585816239 ) ) ;
#47408 = CARTESIAN_POINT ( 'NONE',  ( -109.0603444146798324, -297.4132932125892808, -297.4262036220541745 ) ) ;
#47409 = CARTESIAN_POINT ( 'NONE',  ( -110.5083084155153443, -292.7544217070788477, -254.6551999153137160 ) ) ;
#47410 = CARTESIAN_POINT ( 'NONE',  ( 3.730982949472132493, -278.6056800005169407, -207.7444452180383792 ) ) ;
#47411 = CIRCLE ( 'NONE', #88249, 2.397123461337413719 ) ;
#47412 = CARTESIAN_POINT ( 'NONE',  ( -99.20366507609693940, -281.0373173936168314, -228.8640943438021793 ) ) ;
#47413 = CARTESIAN_POINT ( 'NONE',  ( -35.75314610685270367, -296.1520347558109734, -195.9216345540877739 ) ) ;
#47414 = CARTESIAN_POINT ( 'NONE',  ( -66.08534010418512139, -285.2847250274622297, -340.4757777030929446 ) ) ;
#47415 = CARTESIAN_POINT ( 'NONE',  ( 31.68585556289645666, -286.7997918608118653, -295.0476047435032569 ) ) ;
#47416 = CARTESIAN_POINT ( 'NONE',  ( 26.96909223665486621, -23.88996772622144249, -344.7745201028783413 ) ) ;
#47417 = ORIENTED_EDGE ( 'NONE', *, *, #2712, .T. ) ;
#47418 = CARTESIAN_POINT ( 'NONE',  ( -38.62102233416989350, -285.7024252220199401, -197.3386961749848183 ) ) ;
#47419 = EDGE_LOOP ( 'NONE', ( #2846, #51891, #36509, #75598 ) ) ;
#47420 = CARTESIAN_POINT ( 'NONE',  ( -35.89119930362267752, -284.1140596053600120, -347.0513531479867311 ) ) ;
#47421 = CARTESIAN_POINT ( 'NONE',  ( -106.3277506709990092, -273.2036926250512465, -246.4234422967631986 ) ) ;
#47422 = CARTESIAN_POINT ( 'NONE',  ( -18.26599194427078032, -285.0874671611159101, -196.1164992782853176 ) ) ;
#47423 = CARTESIAN_POINT ( 'NONE',  ( -17.06571014245249529, -281.2489917871808416, -196.3225844852802311 ) ) ;
#47424 = CARTESIAN_POINT ( 'NONE',  ( 199.0872936271226479, 69.92583464099142532, -8.677435037599659395 ) ) ;
#47425 = CARTESIAN_POINT ( 'NONE',  ( -110.6763272792857435, -280.3390741257584295, -249.2722532903270292 ) ) ;
#47426 = CARTESIAN_POINT ( 'NONE',  ( 3.807081742047634609, -280.9228225300652184, -205.2403197321870607 ) ) ;
#47427 = CARTESIAN_POINT ( 'NONE',  ( -53.28691492658257545, -289.3380690714490129, -200.3538533559491555 ) ) ;
#47428 = CARTESIAN_POINT ( 'NONE',  ( -99.18224766838898177, -248.6449173048312105, -334.3546491526849991 ) ) ;
#47429 = EDGE_LOOP ( 'NONE', ( #81577, #86213, #42274, #69360, #23831, #78715, #89116, #77380 ) ) ;
#47430 = CARTESIAN_POINT ( 'NONE',  ( -29.83056001419215519, -276.1476309348029758, -195.9056870182791386 ) ) ;
#47431 = CARTESIAN_POINT ( 'NONE',  ( -13.44854438592516743, -91.33897161315739766, -359.8347524150512413 ) ) ;
#47432 = CIRCLE ( 'NONE', #21725, 0.5000000000000004441 ) ;
#47433 = CARTESIAN_POINT ( 'NONE',  ( 33.79121296540559882, -279.8676103630207308, -293.1557082655626800 ) ) ;
#47434 = CARTESIAN_POINT ( 'NONE',  ( -27.99624598022954913, -293.9292366935629843, -194.8983609080697192 ) ) ;
#47435 = CARTESIAN_POINT ( 'NONE',  ( -37.00339734540678904, -294.3963586086436521, -343.4747099381384601 ) ) ;
#47436 = CARTESIAN_POINT ( 'NONE',  ( -107.2019207893588231, -290.4739283764644142, -237.9994977240889114 ) ) ;
#47437 = CARTESIAN_POINT ( 'NONE',  ( -107.1748277085148118, -264.8307257489140625, -305.4825756969800068 ) ) ;
#47439 = CARTESIAN_POINT ( 'NONE',  ( 33.07081732972576305, -286.2437860648411743, -292.6334883398951661 ) ) ;
#47438 = CARTESIAN_POINT ( 'NONE',  ( -112.5558899282725491, -295.2966404529260558, -256.8914503373235334 ) ) ;
#47440 = CARTESIAN_POINT ( 'NONE',  ( 13.21311059842174451, -296.1972275886332682, -324.7922102373204893 ) ) ;
#47441 = CARTESIAN_POINT ( 'NONE',  ( 33.50911789645265770, -285.9806498269613257, -250.8315234100532791 ) ) ;
#47442 = CARTESIAN_POINT ( 'NONE',  ( -109.9831983042996058, -285.7168804234313484, -281.8431347602841583 ) ) ;
#47443 = EDGE_LOOP ( 'NONE', ( #32780, #6459, #57515, #56997, #51538, #28941 ) ) ;
#47444 = CARTESIAN_POINT ( 'NONE',  ( 39.42026268742862527, -294.4566775741820948, -267.4335819055772276 ) ) ;
#47445 = CARTESIAN_POINT ( 'NONE',  ( -6.000861196347877069, -283.1211577672743829, -336.3729125533952811 ) ) ;
#47446 = CARTESIAN_POINT ( 'NONE',  ( -64.14171714688964698, -294.1890833164350738, -342.1230006651120448 ) ) ;
#47447 = AXIS2_PLACEMENT_3D ( 'NONE', #12245, #83739, #61065 ) ;
#47448 = CARTESIAN_POINT ( 'NONE',  ( -112.4054015943029583, -291.1492005077801082, -286.7806046825298267 ) ) ;
#47449 = CARTESIAN_POINT ( 'NONE',  ( -56.17979313988788448, -292.3082557503146859, -195.7096097580475771 ) ) ;
#47450 = CARTESIAN_POINT ( 'NONE',  ( -105.1122525118403104, -290.3540714552113400, -297.6289009731979718 ) ) ;
#47451 = ORIENTED_EDGE ( 'NONE', *, *, #12262, .T. ) ;
#47452 = DIRECTION ( 'NONE',  ( 0.000000000000000000, 1.000000000000000000, 0.000000000000000000 ) ) ;
#47453 = CARTESIAN_POINT ( 'NONE',  ( -107.2263898719252069, -298.0327134352918392, -299.7617222634390828 ) ) ;
#47454 = CARTESIAN_POINT ( 'NONE',  ( -24.21248841555564013, -273.0110100372268107, -194.8378147414888133 ) ) ;
#47455 = EDGE_CURVE ( 'NONE', #25970, #77341, #11883, .T. ) ;
#47456 = CARTESIAN_POINT ( 'NONE',  ( -68.61291896196424034, -278.6894964789363485, -204.1378643508918458 ) ) ;
#47457 = EDGE_LOOP ( 'NONE', ( #13709, #4031, #2634, #32390 ) ) ;
#47458 = CARTESIAN_POINT ( 'NONE',  ( 39.49327698980793144, -274.9983360849891483, -265.4499592058275539 ) ) ;
#47459 = CARTESIAN_POINT ( 'NONE',  ( -108.1199337881546398, -295.3009131489678225, -249.8391932867297385 ) ) ;
#47460 = CARTESIAN_POINT ( 'NONE',  ( -87.92008665302070369, -279.6289079625661884, -324.6997993695976561 ) ) ;
#47461 = CARTESIAN_POINT ( 'NONE',  ( -11.03063068004470004, -272.5382379393943211, -200.8900630760448962 ) ) ;
#47462 = CARTESIAN_POINT ( 'NONE',  ( -5.354663166924825468, -295.8266930832711523, -336.4352807222431352 ) ) ;
#47463 = CARTESIAN_POINT ( 'NONE',  ( -101.4916713185849488, -298.1147185321518123, -234.8786255520706732 ) ) ;
#47464 = LINE ( 'NONE', #5353, #70190 ) ;
#47465 = CARTESIAN_POINT ( 'NONE',  ( -75.39822371242237864, -299.1540508785749353, -204.2843317397194198 ) ) ;
#47466 = CARTESIAN_POINT ( 'NONE',  ( -29.27895349601016406, -296.1527012719359391, -195.1971838205473375 ) ) ;
#47467 = CARTESIAN_POINT ( 'NONE',  ( 26.31924943952492768, -293.7111588374173721, -234.3248415415681336 ) ) ;
#47468 = CARTESIAN_POINT ( 'NONE',  ( -105.2397746907739986, -289.5060556926109712, -241.8520794767093776 ) ) ;
#47469 = CARTESIAN_POINT ( 'NONE',  ( 6.501289990623595472, -300.6011461931510667, -195.3461625447490917 ) ) ;
#47470 = CARTESIAN_POINT ( 'NONE',  ( 4.824189293165201953, -275.0972689818939330, -205.9429204830475157 ) ) ;
#47471 = CARTESIAN_POINT ( 'NONE',  ( -93.77973342082707120, -273.3749006517828661, -224.0409410538604504 ) ) ;
#47472 = CARTESIAN_POINT ( 'NONE',  ( -2.374504463421271083, -284.5716752170822588, -337.1121631646437891 ) ) ;
#47473 = CARTESIAN_POINT ( 'NONE',  ( -66.40452724787992622, -282.1096478607734639, -341.1470334836013762 ) ) ;
#47474 = CARTESIAN_POINT ( 'NONE',  ( -45.64686461744222612, -276.5032441622067836, -346.8623701648375004 ) ) ;
#47475 = CARTESIAN_POINT ( 'NONE',  ( 208.2002831509629175, 1.063508326896295486, -7.500000000000015099 ) ) ;
#47476 = CARTESIAN_POINT ( 'NONE',  ( -108.2522530744371210, -283.5121569656338920, -288.3693163455671424 ) ) ;
#47477 = CARTESIAN_POINT ( 'NONE',  ( 35.89710774520484193, -279.3346401882822647, -253.3898294352219125 ) ) ;
#47478 = ADVANCED_FACE ( 'NONE', ( #85925 ), #48168, .T. ) ;
#47479 = CARTESIAN_POINT ( 'NONE',  ( 36.18973025653325948, -274.1792362902468199, -274.3626201796190571 ) ) ;
#47480 = CARTESIAN_POINT ( 'NONE',  ( -21.29540734494232268, -278.8466385558581919, -343.6769882151688194 ) ) ;
#47481 = CARTESIAN_POINT ( 'NONE',  ( 209.1374487190023501, 30.94653725228601715, 12.09245862095555601 ) ) ;
#47482 = CARTESIAN_POINT ( 'NONE',  ( 196.8803347170859865, 20.19615242270662847, 12.49999999999999289 ) ) ;
#47483 = CARTESIAN_POINT ( 'NONE',  ( -111.6584955308033216, -271.1648000688354614, -253.5250157027853959 ) ) ;
#47484 = AXIS2_PLACEMENT_3D ( 'NONE', #19187, #48047, #76952 ) ;
#47485 = CARTESIAN_POINT ( 'NONE',  ( -61.78514788984986694, -279.3691083284649608, -341.4973439075864121 ) ) ;
#47486 = CARTESIAN_POINT ( 'NONE',  ( -74.94434090351494149, -277.8906705383787994, 30.50000000000000000 ) ) ;
#47487 = CARTESIAN_POINT ( 'NONE',  ( -66.00687912452282546, -285.3444535061283318, -340.2865640699754408 ) ) ;
#47488 = ORIENTED_EDGE ( 'NONE', *, *, #80317, .T. ) ;
#47489 = AXIS2_PLACEMENT_3D ( 'NONE', #52968, #66275, #44928 ) ;
#47490 = CARTESIAN_POINT ( 'NONE',  ( 159.4851178187871312, 15.00000000000000178, -10.00000000000000178 ) ) ;
#47491 = CARTESIAN_POINT ( 'NONE',  ( 35.60531716339978203, -285.7764613812878451, -287.8429838378509658 ) ) ;
#47492 = PLANE ( 'NONE',  #52767 ) ;
#47493 = CARTESIAN_POINT ( 'NONE',  ( -110.6389998346100185, -295.2968748261232008, -274.1868675226101573 ) ) ;
#47494 = CARTESIAN_POINT ( 'NONE',  ( 4.288016781803740685, -286.6242855029354928, -331.8871624122991193 ) ) ;
#47495 = CARTESIAN_POINT ( 'NONE',  ( 197.0349383350915105, 285.8449894349855640, -111.9383547020201064 ) ) ;
#47496 = CARTESIAN_POINT ( 'NONE',  ( -109.3733055791940956, -294.8209521514482958, -249.4697689045983680 ) ) ;
#47497 = CARTESIAN_POINT ( 'NONE',  ( -18.33583071450935620, -284.7724716257929458, -196.4046497857824818 ) ) ;
#47498 = CARTESIAN_POINT ( 'NONE',  ( 20.28809305134553753, -282.5080102124807127, -224.2607128227005830 ) ) ;
#47499 = CARTESIAN_POINT ( 'NONE',  ( -95.50927080877582398, -282.1247238825616819, -319.2740768333006827 ) ) ;
#47500 = CARTESIAN_POINT ( 'NONE',  ( -104.0477169485465652, -290.1514632624219416, -300.1390707392179138 ) ) ;
#47501 = AXIS2_PLACEMENT_3D ( 'NONE', #58135, #85123, #86046 ) ;
#47502 = CIRCLE ( 'NONE', #91365, 4.999999999999990230 ) ;
#47503 = CARTESIAN_POINT ( 'NONE',  ( -103.9105531645786584, -280.3992849684564135, -238.8731022798182835 ) ) ;
#47504 = CARTESIAN_POINT ( 'NONE',  ( 2.784022759097974919, -281.4082215602958286, -209.1241289755912760 ) ) ;
#47505 = EDGE_CURVE ( 'NONE', #81416, #25769, #11842, .T. ) ;
#47506 = CARTESIAN_POINT ( 'NONE',  ( 36.66986701849825181, -289.3510003499635559, -256.1944410992196595 ) ) ;
#47507 = ORIENTED_EDGE ( 'NONE', *, *, #29881, .F. ) ;
#47508 = CARTESIAN_POINT ( 'NONE',  ( -105.6089422716172948, -273.0129119305963172, -234.6286964650097957 ) ) ;
#47509 = CARTESIAN_POINT ( 'NONE',  ( -95.58990173591513440, -293.1773796353858188, -223.6611051430612065 ) ) ;
#47510 = FACE_OUTER_BOUND ( 'NONE', #46755, .T. ) ;
#47511 = CARTESIAN_POINT ( 'NONE',  ( -115.3288506153726871, -292.8376638359844719, -288.1938231032136741 ) ) ;
#47512 = EDGE_LOOP ( 'NONE', ( #71018, #40777, #26829, #78095 ) ) ;
#47513 = CARTESIAN_POINT ( 'NONE',  ( -28.83444490674152760, -274.9445047091547849, -345.0971162895368707 ) ) ;
#47514 = CARTESIAN_POINT ( 'NONE',  ( 139.1539576904058606, 276.0000000000000568, -10.49999999999999822 ) ) ;
#47515 = CARTESIAN_POINT ( 'NONE',  ( -16.74293211478747878, -293.1904063318108911, -343.7787817393394221 ) ) ;
#47516 = CARTESIAN_POINT ( 'NONE',  ( -75.23720573856124361, -297.0402515931730818, -207.8371213331801073 ) ) ;
#47517 = CARTESIAN_POINT ( 'NONE',  ( -82.96044504382304297, -291.2096642047586101, -328.2371740230512387 ) ) ;
#47518 = AXIS2_PLACEMENT_3D ( 'NONE', #76071, #68037, #3163 ) ;
#47519 = CARTESIAN_POINT ( 'NONE',  ( -68.18651957364731686, -285.2230515667905024, -337.6409153176431346 ) ) ;
#47520 = CARTESIAN_POINT ( 'NONE',  ( -79.28625121524561337, -292.9236369733330321, -206.4287680954979578 ) ) ;
#47521 = CARTESIAN_POINT ( 'NONE',  ( -50.49812231399131690, -293.2026845073552295, -194.9939711158508544 ) ) ;
#47522 = CARTESIAN_POINT ( 'NONE',  ( -65.32499675398028671, -291.5092509534115948, -202.9240539062371056 ) ) ;
#47523 = CARTESIAN_POINT ( 'NONE',  ( -27.60135774694489541, -288.1760595989682656, -195.9962984954004810 ) ) ;
#47524 = CARTESIAN_POINT ( 'NONE',  ( 15.15978232629504241, -280.9352679105275570, -213.9624445336816336 ) ) ;
#47525 = CARTESIAN_POINT ( 'NONE',  ( -104.6855990875592397, -294.1810387019559130, -304.7417875851074314 ) ) ;
#47526 = CARTESIAN_POINT ( 'NONE',  ( -0.3773029460514870648, -282.4080053068450979, -337.9233243674437972 ) ) ;
#47527 = CARTESIAN_POINT ( 'NONE',  ( 27.70765615082352440, -276.9308217806917014, -234.4846887558680351 ) ) ;
#47528 = ADVANCED_FACE ( 'NONE', ( #66957 ), #24802, .T. ) ;
#47529 = CARTESIAN_POINT ( 'NONE',  ( -105.5937364680635966, -281.2662352645559167, -254.8156830097664738 ) ) ;
#47530 = CARTESIAN_POINT ( 'NONE',  ( -99.46647925246774946, -276.1091365146644421, -313.7295085455024832 ) ) ;
#47531 = FACE_OUTER_BOUND ( 'NONE', #82604, .T. ) ;
#47532 = CARTESIAN_POINT ( 'NONE',  ( -8.475693163766912619, -282.1714385259087408, -337.4784934059893544 ) ) ;
#47533 = CARTESIAN_POINT ( 'NONE',  ( -25.47232795450291221, -281.4052851904296517, -194.6833357616488343 ) ) ;
#47534 = CARTESIAN_POINT ( 'NONE',  ( -89.71692275410507023, -284.3938785119666477, -214.1670333773750770 ) ) ;
#47535 = CARTESIAN_POINT ( 'NONE',  ( -6.873294218886489837, -294.2177812038362958, -202.9100226822693571 ) ) ;
#47536 = CARTESIAN_POINT ( 'NONE',  ( 26.25157757958301374, -276.5944132812682597, -228.3809387848266397 ) ) ;
#47537 = CARTESIAN_POINT ( 'NONE',  ( 11.45817441120040314, -276.0274606959614516, -211.3697081764578911 ) ) ;
#47538 = CARTESIAN_POINT ( 'NONE',  ( 7.578722814606958735, -276.2531303639588032, -327.9681698734675024 ) ) ;
#47539 = CARTESIAN_POINT ( 'NONE',  ( -85.64246906516477509, -297.7219809988185375, -327.5873719487264566 ) ) ;
#47540 = CARTESIAN_POINT ( 'NONE',  ( -73.23143963290321778, -283.5750233033973586, -204.6810684702057017 ) ) ;
#47541 = CARTESIAN_POINT ( 'NONE',  ( 36.68499868472477488, -292.9535894915959489, -249.1992875222266832 ) ) ;
#47542 = CARTESIAN_POINT ( 'NONE',  ( 37.32847133688010643, -289.3442701305405649, -285.5534157374442543 ) ) ;
#47543 = CARTESIAN_POINT ( 'NONE',  ( 21.24910357455268795, -291.8563801456648434, -226.3004348748939094 ) ) ;
#47544 = ORIENTED_EDGE ( 'NONE', *, *, #78765, .T. ) ;
#47545 = CARTESIAN_POINT ( 'NONE',  ( 1.416997135172548106, -291.1337252148142625, -204.4495259250804509 ) ) ;
#47546 = CARTESIAN_POINT ( 'NONE',  ( 26.25505679491628186, -292.7266229670518101, -234.3755570041977876 ) ) ;
#47547 = EDGE_LOOP ( 'NONE', ( #34323, #84351, #85168, #17192 ) ) ;
#47548 = CARTESIAN_POINT ( 'NONE',  ( -57.19755612380235732, -290.3820500497033663, -344.4918889757568081 ) ) ;
#47549 = CARTESIAN_POINT ( 'NONE',  ( -108.6283233598747699, -279.0947672837481264, -254.4828375281031470 ) ) ;
#47550 = CARTESIAN_POINT ( 'NONE',  ( -109.1529620085846943, -295.1289140791500358, -297.4300669584623051 ) ) ;
#47551 = CARTESIAN_POINT ( 'NONE',  ( -71.02906988141430134, -286.2706121519483986, -201.2346114436066387 ) ) ;
#47552 = CARTESIAN_POINT ( 'NONE',  ( -29.46932064590940215, -286.4825686396810625, -193.7858613210267151 ) ) ;
#47553 = CARTESIAN_POINT ( 'NONE',  ( -99.04663183502438528, -284.3448762203460092, -309.5017538438171982 ) ) ;
#47554 = CARTESIAN_POINT ( 'NONE',  ( 203.1405228849236551, 295.9636489450776367, -54.00000000004142464 ) ) ;
#47555 = CARTESIAN_POINT ( 'NONE',  ( -91.06148389132593479, -229.3667599500281256, -346.6633138930380937 ) ) ;
#47556 = CARTESIAN_POINT ( 'NONE',  ( 178.6937129019192412, 251.6256410920926214, -164.2356949225344067 ) ) ;
#47557 = CARTESIAN_POINT ( 'NONE',  ( 32.21852534477521601, -274.4472130652386568, -247.5270200052369489 ) ) ;
#47558 = CARTESIAN_POINT ( 'NONE',  ( 25.63411541957023587, -274.9862526052712610, -307.8880780139328408 ) ) ;
#47559 = CARTESIAN_POINT ( 'NONE',  ( -113.5399384530185500, -296.1942588607597600, -259.6190226704199517 ) ) ;
#47560 = CARTESIAN_POINT ( 'NONE',  ( 85.70268185674719064, 81.17150233424827377, -299.2961519048424179 ) ) ;
#47561 = CARTESIAN_POINT ( 'NONE',  ( 0.7866359285302773063, -275.2399191282585207, -336.7501424353915809 ) ) ;
#47562 = CARTESIAN_POINT ( 'NONE',  ( -108.1727679605407815, -274.5947437918048308, -248.7160093815739117 ) ) ;
#47563 = VERTEX_POINT ( 'NONE', #58928 ) ;
#47564 = CARTESIAN_POINT ( 'NONE',  ( -87.84319746015545149, -274.4455869132079329, -212.5748954210873478 ) ) ;
#47565 = CARTESIAN_POINT ( 'NONE',  ( -108.7720538813131697, -291.2468524401055561, -255.0088215890920935 ) ) ;
#47566 = CARTESIAN_POINT ( 'NONE',  ( -90.59278332608258211, -296.5861977347719858, -325.8282333287130541 ) ) ;
#47567 = CARTESIAN_POINT ( 'NONE',  ( -112.8295280142959598, -297.2314629928028467, -255.4234104085188903 ) ) ;
#47568 = CARTESIAN_POINT ( 'NONE',  ( -42.38760562295917111, -295.2842404874551789, -343.1865176879359751 ) ) ;
#47569 = VERTEX_POINT ( 'NONE', #39439 ) ;
#47570 = VECTOR ( 'NONE', #65848, 1000.000000000000000 ) ;
#47571 = CARTESIAN_POINT ( 'NONE',  ( -25.96224266893775479, -278.8284713593610604, -345.0593250816299360 ) ) ;
#47572 = ORIENTED_EDGE ( 'NONE', *, *, #47032, .T. ) ;
#47573 = CARTESIAN_POINT ( 'NONE',  ( -45.26079598530847647, -279.4621824805769847, -193.7783404584913001 ) ) ;
#47574 = CARTESIAN_POINT ( 'NONE',  ( 19.37139351922690267, -277.1475549607477546, -316.7169759195553524 ) ) ;
#47575 = CARTESIAN_POINT ( 'NONE',  ( -34.30880400572465305, -278.7746452029656439, -346.2872370499692352 ) ) ;
#47576 = CARTESIAN_POINT ( 'NONE',  ( -64.52576852215828751, -275.4252178164295515, -340.6973120444997676 ) ) ;
#47577 = CARTESIAN_POINT ( 'NONE',  ( -51.57958507967996553, -274.3575882932390186, -198.6484781452173252 ) ) ;
#47578 = CARTESIAN_POINT ( 'NONE',  ( -94.90093830430885191, -295.7692264448830315, -224.5101744834705642 ) ) ;
#47579 = LINE ( 'NONE', #56599, #79010 ) ;
#47580 = CARTESIAN_POINT ( 'NONE',  ( -107.9731207818836936, -278.9629374276731824, -251.8674347539733844 ) ) ;
#47581 = VECTOR ( 'NONE', #64745, 1000.000000000000114 ) ;
#47582 = CARTESIAN_POINT ( 'NONE',  ( -59.89796240640044545, -288.0233021212309268, -343.4672962697396201 ) ) ;
#47583 = CARTESIAN_POINT ( 'NONE',  ( 18.52851441622891215, -276.8548607413847549, -220.2496433184762168 ) ) ;
#47584 = FACE_OUTER_BOUND ( 'NONE', #48964, .T. ) ;
#47585 = CARTESIAN_POINT ( 'NONE',  ( -95.08430858530101659, -289.1175331037509864, -315.3078900554295956 ) ) ;
#47586 = CARTESIAN_POINT ( 'NONE',  ( -104.3322976382552980, -283.4089440004628386, -308.2257436787626261 ) ) ;
#47587 = CARTESIAN_POINT ( 'NONE',  ( 30.23057755494690824, -280.1945898762396041, -300.6855665464400431 ) ) ;
#47589 = CARTESIAN_POINT ( 'NONE',  ( -90.67787887103109767, -283.3691259256360695, -218.3587014142066778 ) ) ;
#47588 = CARTESIAN_POINT ( 'NONE',  ( 11.71198929502814501, -279.3240363667945871, -215.5057584475467252 ) ) ;
#47590 = CARTESIAN_POINT ( 'NONE',  ( -22.29675490276056848, -288.2448550826783276, -196.8331817600846705 ) ) ;
#47591 = CARTESIAN_POINT ( 'NONE',  ( -110.5632759572167885, -279.6816070372574359, -276.1252648904854823 ) ) ;
#47592 = FACE_OUTER_BOUND ( 'NONE', #54104, .T. ) ;
#47593 = CARTESIAN_POINT ( 'NONE',  ( -63.71014044453618652, -293.7087111566733029, -200.0945302020680856 ) ) ;
#47594 = B_SPLINE_CURVE_WITH_KNOTS ( 'NONE', 3,
 ( #68239, #62069, #89993, #68712, #69638, #18988, #47840, #18045 ),
 .UNSPECIFIED., .F., .F.,
 ( 4, 2, 2, 4 ),
 ( -8.944277078438763205E-06, 0.001321608365870415719, 0.001986884687344899272, 0.002652161008819382826 ),
 .UNSPECIFIED. ) ;
#47595 = CARTESIAN_POINT ( 'NONE',  ( -111.4089096642188679, -277.0070971581349681, -253.3898926433860197 ) ) ;
#47596 = CARTESIAN_POINT ( 'NONE',  ( -51.29222526829494910, -277.8866740735675762, -342.1195705589668137 ) ) ;
#47597 = CARTESIAN_POINT ( 'NONE',  ( -91.10423642050577087, -285.8140612890744592, -322.8931854967257777 ) ) ;
#47598 = CARTESIAN_POINT ( 'NONE',  ( 196.9307570179617244, 70.66253453039786336, 10.51418682698406748 ) ) ;
#47599 = CARTESIAN_POINT ( 'NONE',  ( -111.7581457573550523, -292.6392090248023123, -257.2650567603678269 ) ) ;
#47600 = CARTESIAN_POINT ( 'NONE',  ( -85.33481484035438314, -293.7147043058071176, -328.0617980502964883 ) ) ;
#47601 = CARTESIAN_POINT ( 'NONE',  ( 37.94801681810128002, -286.9416978265425655, -285.7109500091943914 ) ) ;
#47602 = CARTESIAN_POINT ( 'NONE',  ( -109.4883952195729648, -289.1547155414114627, -254.8274511637614808 ) ) ;
#47603 = CARTESIAN_POINT ( 'NONE',  ( 82.68073018288104947, -297.0543924324409204, -195.4120394483015559 ) ) ;
#47604 = CARTESIAN_POINT ( 'NONE',  ( 1.115301559305689416, -275.2122857020949596, -333.0491960670415210 ) ) ;
#47605 = CARTESIAN_POINT ( 'NONE',  ( 26.84905820180849645, -292.1948161928117429, -307.6493470018145899 ) ) ;
#47606 = CARTESIAN_POINT ( 'NONE',  ( 196.4610981682406532, 41.67863480118781183, 13.65708146052827843 ) ) ;
#47607 = CARTESIAN_POINT ( 'NONE',  ( 197.4836817735085219, 42.27872732282707346, 11.66666666666667673 ) ) ;
#47608 = CARTESIAN_POINT ( 'NONE',  ( -19.52965614330108224, -290.7569505352001329, -196.1081412905921297 ) ) ;
#47609 = CARTESIAN_POINT ( 'NONE',  ( -96.41845246222676735, -286.7663842029486432, -226.1301587960186623 ) ) ;
#47610 = CARTESIAN_POINT ( 'NONE',  ( -37.52198627677552878, -287.2942095360349413, -346.3604735338157639 ) ) ;
#47611 = CARTESIAN_POINT ( 'NONE',  ( -86.13026583795144120, -286.7854615180390283, -215.2016999400666180 ) ) ;
#47612 = LINE ( 'NONE', #68005, #85014 ) ;
#47613 = CARTESIAN_POINT ( 'NONE',  ( 4.810073576419219954, -287.4403704319697113, -210.5008873459819938 ) ) ;
#47614 = CARTESIAN_POINT ( 'NONE',  ( 36.70423329606516205, -295.3533101847598346, -256.3751768772215200 ) ) ;
#47615 = CARTESIAN_POINT ( 'NONE',  ( -108.3912483775651907, -276.2992734078989088, -296.2296007827430344 ) ) ;
#47616 = CARTESIAN_POINT ( 'NONE',  ( 39.53294640657126990, -275.8238315351299548, -265.4368990987728125 ) ) ;
#47617 = CARTESIAN_POINT ( 'NONE',  ( -1.465605998608614291, -290.6039150269379547, -203.8613430214066966 ) ) ;
#47618 = CARTESIAN_POINT ( 'NONE',  ( -98.57635774909127235, -279.1747062544077949, -223.6564873353267160 ) ) ;
#47619 = CARTESIAN_POINT ( 'NONE',  ( -97.72442964321508896, -297.9311378339749581, -314.2665527876299052 ) ) ;
#47620 = CARTESIAN_POINT ( 'NONE',  ( -48.18343439339132317, -253.0206516614774728, -474.6280563232480745 ) ) ;
#47621 = CARTESIAN_POINT ( 'NONE',  ( 82.61707336526248469, -302.0539871969763226, -195.3101965168185075 ) ) ;
#47622 = CARTESIAN_POINT ( 'NONE',  ( -9.289759988345592134, -285.1115109857813081, -202.4186417087223333 ) ) ;
#47623 = CARTESIAN_POINT ( 'NONE',  ( -110.3425317100750505, -276.8666151121439611, -256.8798691341774543 ) ) ;
#47624 = CARTESIAN_POINT ( 'NONE',  ( 35.39792894632608977, -279.3172539828678964, -252.0869007789418106 ) ) ;
#47625 = DIRECTION ( 'NONE',  ( 0.000000000000000000, -1.000000000000000000, 0.000000000000000000 ) ) ;
#47626 = CARTESIAN_POINT ( 'NONE',  ( 15.56042246569386123, -273.2641615382976852, -215.3695442951176062 ) ) ;
#47627 = CARTESIAN_POINT ( 'NONE',  ( 35.00873177644231760, -295.2552802114641963, -284.3655014811394608 ) ) ;
#47628 = CARTESIAN_POINT ( 'NONE',  ( 20.84060621698269955, -279.7952161945113971, -220.3780411768001102 ) ) ;
#47629 = CARTESIAN_POINT ( 'NONE',  ( -41.03914793408155504, -296.0410437592004769, -343.5156244233089637 ) ) ;
#47630 = CARTESIAN_POINT ( 'NONE',  ( -113.1615712570140317, -297.7336866771927930, -280.9781290011997612 ) ) ;
#47631 = CARTESIAN_POINT ( 'NONE',  ( -37.82038706130927608, -297.8793107173324870, -197.3626874284838095 ) ) ;
#47632 = CARTESIAN_POINT ( 'NONE',  ( -93.17872728426682727, -293.2499372518411747, -220.2696827246394378 ) ) ;
#47633 = CARTESIAN_POINT ( 'NONE',  ( -110.9266604951672832, -285.0056532324294949, -247.5044796652495052 ) ) ;
#47634 = CARTESIAN_POINT ( 'NONE',  ( 37.70401613017851616, -273.5593766588340259, -259.9473793853367738 ) ) ;
#47635 = CARTESIAN_POINT ( 'NONE',  ( -54.50368079889251050, -289.0999634222840200, -345.4789130982442771 ) ) ;
#47636 = EDGE_CURVE ( 'NONE', #74793, #66186, #22928, .T. ) ;
#47637 = CARTESIAN_POINT ( 'NONE',  ( 31.61693705707779145, -286.9381889639606129, -295.0211018719610365 ) ) ;
#47638 = CARTESIAN_POINT ( 'NONE',  ( -94.12946154819205447, -289.2314237030576578, -221.3501623968813874 ) ) ;
#47639 = ORIENTED_EDGE ( 'NONE', *, *, #89695, .T. ) ;
#47640 = CARTESIAN_POINT ( 'NONE',  ( 172.7732574597264659, 233.5132621949535121, -195.2123807395911399 ) ) ;
#47641 = CARTESIAN_POINT ( 'NONE',  ( -13.27351186111235570, -288.2385630439052306, -339.3445272571921691 ) ) ;
#47642 = CARTESIAN_POINT ( 'NONE',  ( 29.33919985515026596, -282.8906705383787994, 30.50000000000000000 ) ) ;
#47643 = CARTESIAN_POINT ( 'NONE',  ( -107.7152394915555789, -285.8870332966218371, -239.5624597823806141 ) ) ;
#47644 =( GEOMETRIC_REPRESENTATION_CONTEXT ( 3 ) GLOBAL_UNCERTAINTY_ASSIGNED_CONTEXT ( ( #69364 ) ) GLOBAL_UNIT_ASSIGNED_CONTEXT ( ( #13813, #28029, #42191 ) ) REPRESENTATION_CONTEXT ( 'NONE', 'WORKASPACE' ) );
#47645 = CARTESIAN_POINT ( 'NONE',  ( 19.25032963359218385, -291.9031308432815877, -218.4943426778026776 ) ) ;
#47646 = CARTESIAN_POINT ( 'NONE',  ( 36.55044709686200122, -282.9169604685616264, -251.7495356683943157 ) ) ;
#47647 = CARTESIAN_POINT ( 'NONE',  ( 23.34582961793901390, -282.2416224719971183, -223.7530071189453622 ) ) ;
#47648 = CARTESIAN_POINT ( 'NONE',  ( -45.64157639274407785, -282.9934550536116262, -342.9387422208430962 ) ) ;
#47649 = CARTESIAN_POINT ( 'NONE',  ( -35.03118515858106008, -279.0232862465290395, -345.3255240185489470 ) ) ;
#47650 = CARTESIAN_POINT ( 'NONE',  ( -114.3097146207065578, -296.5974982793034087, -266.7352797015803390 ) ) ;
#47651 = CARTESIAN_POINT ( 'NONE',  ( -92.88046569008872666, -289.2705273134654362, -220.4692463708019829 ) ) ;
#47652 = AXIS2_PLACEMENT_3D ( 'NONE', #49197, #84694, #70528 ) ;
#47653 = CARTESIAN_POINT ( 'NONE',  ( -68.16500847693738763, -296.5579384447445364, -203.8331143420233218 ) ) ;
#47654 = ORIENTED_EDGE ( 'NONE', *, *, #83488, .F. ) ;
#47655 = ORIENTED_EDGE ( 'NONE', *, *, #34577, .T. ) ;
#47656 = CARTESIAN_POINT ( 'NONE',  ( 150.8012326218627948, 131.0000000000000568, -11.50000000000000000 ) ) ;
#47657 = CARTESIAN_POINT ( 'NONE',  ( -95.25752081037309438, -287.1210467887561890, -223.5747658964220363 ) ) ;
#47658 = CARTESIAN_POINT ( 'NONE',  ( 8.731465330671609237, -295.5166386557660871, -331.6698117666222743 ) ) ;
#47659 = CARTESIAN_POINT ( 'NONE',  ( 9.980988713669042056, -283.0315010312393156, -326.1453366281459125 ) ) ;
#47660 = CARTESIAN_POINT ( 'NONE',  ( -2.841629983217734967, -275.6661519946530916, -338.9510035292726684 ) ) ;
#47661 = CARTESIAN_POINT ( 'NONE',  ( -47.73783457298037547, -292.5748200191452497, -194.1153131082313337 ) ) ;
#47662 = CARTESIAN_POINT ( 'NONE',  ( -108.8042121782666669, -283.0144182493546055, -245.1933836623553589 ) ) ;
#47663 = CARTESIAN_POINT ( 'NONE',  ( -81.92159288018133623, -291.7960432747566983, -207.6046246638865114 ) ) ;
#47664 = CARTESIAN_POINT ( 'NONE',  ( -109.4393033478242074, -290.7317245770276486, -282.0165711778835771 ) ) ;
#47665 = CARTESIAN_POINT ( 'NONE',  ( 10.19742947581765691, -229.5268262511776527, -22.50000000000000000 ) ) ;
#47666 = DIRECTION ( 'NONE',  ( 0.000000000000000000, 0.000000000000000000, 1.000000000000000000 ) ) ;
#47667 = CARTESIAN_POINT ( 'NONE',  ( -109.6358133930788341, -268.7236802452458164, -295.3006767381334612 ) ) ;
#47668 = CARTESIAN_POINT ( 'NONE',  ( -19.06552280945043876, -284.3413264348214398, -344.5012716072055241 ) ) ;
#47669 = CARTESIAN_POINT ( 'NONE',  ( -110.4683760289727132, -281.8380690714489560, -287.0191576251351080 ) ) ;
#47670 = ORIENTED_EDGE ( 'NONE', *, *, #86916, .F. ) ;
#47671 = CARTESIAN_POINT ( 'NONE',  ( 28.06336765206942729, -280.0234616424397132, -237.1365389942568527 ) ) ;
#47672 = CARTESIAN_POINT ( 'NONE',  ( 37.21720677263221688, -275.4585890701054609, -289.5108880434040657 ) ) ;
#47673 = CARTESIAN_POINT ( 'NONE',  ( -37.02551789679036176, -282.0562785194675826, -195.5284482456149533 ) ) ;
#47674 = CARTESIAN_POINT ( 'NONE',  ( -61.30215766228251084, -183.8136707010272062, -360.3189382787912791 ) ) ;
#47675 = CARTESIAN_POINT ( 'NONE',  ( 28.78580410112975230, -279.6251867241250011, -232.0758796252319769 ) ) ;
#47676 = CARTESIAN_POINT ( 'NONE',  ( -110.2665141793495991, -282.7785645576452112, -254.3698580139528929 ) ) ;
#47677 = CARTESIAN_POINT ( 'NONE',  ( 29.65232855243818832, -300.6400987876805857, -194.3546781410696269 ) ) ;
#47678 = CARTESIAN_POINT ( 'NONE',  ( -12.98181965744049826, -295.2193703978383041, -339.2953684515639452 ) ) ;
#47679 = VERTEX_POINT ( 'NONE', #68355 ) ;
#47680 = CARTESIAN_POINT ( 'NONE',  ( 36.20138064381440302, -292.2424506577810348, -270.7793319094438402 ) ) ;
#47681 = CARTESIAN_POINT ( 'NONE',  ( 5.820931290189878204, -277.1350206301834760, -334.0030855463894000 ) ) ;
#47682 = CARTESIAN_POINT ( 'NONE',  ( -16.64066289968322465, -274.3270282708923560, -200.3050735678479555 ) ) ;
#47683 = CARTESIAN_POINT ( 'NONE',  ( 25.80451277027892232, -275.0504242463206310, -313.9736759531064081 ) ) ;
#47684 = CARTESIAN_POINT ( 'NONE',  ( 175.2296996224750103, 21.00000000000000000, 0.000000000000000000 ) ) ;
#47685 = CARTESIAN_POINT ( 'NONE',  ( -1.804745578269042694, -272.5227405973731152, -204.3004272533835888 ) ) ;
#47686 = CARTESIAN_POINT ( 'NONE',  ( 219.8344101925596021, 3.000000000000000000, -10.00000000000000000 ) ) ;
#47687 = CARTESIAN_POINT ( 'NONE',  ( -43.41716441663519532, -261.3309580482948036, -500.0881477262567500 ) ) ;
#47688 = CARTESIAN_POINT ( 'NONE',  ( 17.84659108932734028, -283.3173887270186810, -318.6154295693416998 ) ) ;
#47689 = CARTESIAN_POINT ( 'NONE',  ( 37.67115646527371808, -283.4669993684191240, -282.5687693303100900 ) ) ;
#47690 = CARTESIAN_POINT ( 'NONE',  ( -100.4933566793570634, -283.3961040028550542, -307.1817771672111235 ) ) ;
#47691 = CARTESIAN_POINT ( 'NONE',  ( 20.63845728254089806, -274.5893592052297549, -316.0404354382346241 ) ) ;
#47692 = CARTESIAN_POINT ( 'NONE',  ( 20.32632437346097376, -284.0631475246072455, -317.1279740642792717 ) ) ;
#47693 = CARTESIAN_POINT ( 'NONE',  ( -73.19611201322258864, -276.0165163483718516, -334.7586242900611637 ) ) ;
#47694 = EDGE_CURVE ( 'NONE', #69489, #65034, #93593, .T. ) ;
#47695 = DIRECTION ( 'NONE',  ( 0.000000000000000000, 0.000000000000000000, 1.000000000000000000 ) ) ;
#47696 = CARTESIAN_POINT ( 'NONE',  ( 34.42112294574901199, -276.4342778598795007, -255.3224628244218479 ) ) ;
#47697 = EDGE_CURVE ( 'NONE', #67402, #31059, #90525, .T. ) ;
#47698 = CARTESIAN_POINT ( 'NONE',  ( 195.8123035524153295, 42.33305793707737053, 12.34482224977402609 ) ) ;
#47699 = CARTESIAN_POINT ( 'NONE',  ( -68.61618267290103290, -280.4543429325115085, -200.1608257721644861 ) ) ;
#47700 = ORIENTED_EDGE ( 'NONE', *, *, #14640, .T. ) ;
#47701 = VERTEX_POINT ( 'NONE', #59398 ) ;
#47702 = CARTESIAN_POINT ( 'NONE',  ( 200.7741138073381819, 15.52361751442932025, 10.00000000000000178 ) ) ;
#47703 = CARTESIAN_POINT ( 'NONE',  ( -54.70491745366501846, -287.6917080216013574, -196.6127338519378043 ) ) ;
#47704 = CARTESIAN_POINT ( 'NONE',  ( 6.150742960839347795, -293.6422031563332666, -329.2545890534848354 ) ) ;
#47705 = CARTESIAN_POINT ( 'NONE',  ( -97.21594565599330906, -289.2528314534004039, -318.6352542560511552 ) ) ;
#47706 = CARTESIAN_POINT ( 'NONE',  ( 34.68207832655853906, -286.0138037230846066, -287.4066262950659052 ) ) ;
#47708 = CARTESIAN_POINT ( 'NONE',  ( -110.2714042347649297, -288.9599911570866198, -257.4502746748822233 ) ) ;
#47707 = CARTESIAN_POINT ( 'NONE',  ( -22.32197938764292999, -284.8228513987478436, -198.2686678903622806 ) ) ;
#47709 = CARTESIAN_POINT ( 'NONE',  ( -110.4902457411891703, -285.6780536511303126, -276.3960810136822488 ) ) ;
#47710 = CARTESIAN_POINT ( 'NONE',  ( -3.647065475366475074, -274.6074148424914370, -337.3804293146052373 ) ) ;
#47711 = CARTESIAN_POINT ( 'NONE',  ( -60.24979907409539237, -284.1600202365473251, -197.6310987883229586 ) ) ;
#47712 = CARTESIAN_POINT ( 'NONE',  ( -23.83641044767545836, -300.2213687122415422, -195.3565049566856828 ) ) ;
#47713 = CARTESIAN_POINT ( 'NONE',  ( 34.11436224735621892, -285.2494619235554296, -246.8693992218734365 ) ) ;
#47714 = CARTESIAN_POINT ( 'NONE',  ( 33.98684027382742556, -282.2750893985226526, -253.7584744255732687 ) ) ;
#47715 = CARTESIAN_POINT ( 'NONE',  ( -64.75411163116002911, -291.4093006804125139, -340.4060248311345163 ) ) ;
#47716 = DIRECTION ( 'NONE',  ( 0.000000000000000000, 1.000000000000000000, 0.000000000000000000 ) ) ;
#47717 = CARTESIAN_POINT ( 'NONE',  ( 196.1627136253405581, 40.86402454320599986, 13.15072824800578388 ) ) ;
#47718 = CARTESIAN_POINT ( 'NONE',  ( -68.90371440078584442, -297.3840149352756725, -339.0276890524650639 ) ) ;
#47719 = CARTESIAN_POINT ( 'NONE',  ( -96.34901561848397478, -277.1875605739548973, -224.0464252348748744 ) ) ;
#47720 = CARTESIAN_POINT ( 'NONE',  ( -25.03720412211271906, -291.4024283152998578, -194.5141787027797307 ) ) ;
#47721 = CARTESIAN_POINT ( 'NONE',  ( -111.0096578522765896, -295.0095970857670409, -265.9483616804477606 ) ) ;
#47722 = CARTESIAN_POINT ( 'NONE',  ( 33.42984690800979308, -280.4971180891677704, -290.1760519707942763 ) ) ;
#47723 = CARTESIAN_POINT ( 'NONE',  ( -0.9986393045823697134, -272.6183191392937033, -205.3811743587416174 ) ) ;
#47724 = CARTESIAN_POINT ( 'NONE',  ( 11.24436098399135098, -294.0568811471003414, -215.1512425903901544 ) ) ;
#47725 = CARTESIAN_POINT ( 'NONE',  ( -106.6662871844225293, -293.4805209788415823, -237.0123917617630696 ) ) ;
#47726 = CARTESIAN_POINT ( 'NONE',  ( -113.6157599027163627, -295.0776209862428914, -266.7486222704873171 ) ) ;
#47727 = CARTESIAN_POINT ( 'NONE',  ( 38.64354924975474148, -291.7557191225909605, -267.4974502809838555 ) ) ;
#47728 = CARTESIAN_POINT ( 'NONE',  ( -95.59184054737738734, -292.6054652558211160, -225.3911717963164278 ) ) ;
#47729 = DIRECTION ( 'NONE',  ( 0.000000000000000000, 0.000000000000000000, -1.000000000000000000 ) ) ;
#47730 = CARTESIAN_POINT ( 'NONE',  ( -75.07162759039111677, -292.3387569462754527, -207.6197985925956857 ) ) ;
#47731 = DIRECTION ( 'NONE',  ( 1.000000000000000000, 0.000000000000000000, 0.000000000000000000 ) ) ;
#47733 = CARTESIAN_POINT ( 'NONE',  ( -20.07216374514698742, -292.2801834026947745, -199.3809759998275410 ) ) ;
#47732 = CARTESIAN_POINT ( 'NONE',  ( -104.3337067412666812, -282.1165640111130415, -304.9783448220904916 ) ) ;
#47734 = CARTESIAN_POINT ( 'NONE',  ( 36.98501116077425621, -281.2997050018714731, -250.1979371213774925 ) ) ;
#47735 = CARTESIAN_POINT ( 'NONE',  ( -109.2847105019817349, -283.8704616686964641, -297.8948449141982451 ) ) ;
#47736 = CARTESIAN_POINT ( 'NONE',  ( -64.50965489499087369, -287.4072960804297168, -340.1442181516828782 ) ) ;
#47737 = DIRECTION ( 'NONE',  ( 0.000000000000000000, 0.000000000000000000, -1.000000000000000000 ) ) ;
#47738 = CARTESIAN_POINT ( 'NONE',  ( -39.54764277663036864, -278.5048414751907444, -194.0734077914263764 ) ) ;
#47739 = CARTESIAN_POINT ( 'NONE',  ( 39.39296711314005250, -286.4875392341477891, -271.5602332263627545 ) ) ;
#47740 = CARTESIAN_POINT ( 'NONE',  ( 195.4997886693276712, 41.25212764115887865, 14.63349899658207498 ) ) ;
#47741 = CARTESIAN_POINT ( 'NONE',  ( 34.07730842769990431, -294.9094495733689882, -251.7663436137316353 ) ) ;
#47742 = CARTESIAN_POINT ( 'NONE',  ( 10.17395498617785599, -277.8371215589682492, -330.2690562992742684 ) ) ;
#47743 = CARTESIAN_POINT ( 'NONE',  ( -93.95423220729134073, -278.8715256370971360, -224.2405293213952291 ) ) ;
#47744 = CARTESIAN_POINT ( 'NONE',  ( 28.05123619982690997, -293.1858820149072358, -229.6061752685889985 ) ) ;
#47745 = CARTESIAN_POINT ( 'NONE',  ( -38.73105522070399331, -281.1493020782292547, -345.9083475415899329 ) ) ;
#47746 = CARTESIAN_POINT ( 'NONE',  ( 33.67128884787867804, -292.8464354397736997, -288.2654148269921848 ) ) ;
#47747 = CARTESIAN_POINT ( 'NONE',  ( -112.1244148901376150, -294.6334884768492657, -264.0136916087113264 ) ) ;
#47748 = EDGE_LOOP ( 'NONE', ( #33662, #88661, #75770, #91704 ) ) ;
#47749 = DIRECTION ( 'NONE',  ( 0.7957555401921946325, 0.6056179655966527076, 0.000000000000000000 ) ) ;
#47750 = CARTESIAN_POINT ( 'NONE',  ( 34.89785664870981918, -293.2081829504113557, -281.6186346569671173 ) ) ;
#47751 = DIRECTION ( 'NONE',  ( 0.000000000000000000, 0.000000000000000000, 1.000000000000000000 ) ) ;
#47752 = CARTESIAN_POINT ( 'NONE',  ( 7.399455738971487229, -285.9094976428776249, -326.5171145203363494 ) ) ;
#47753 = CARTESIAN_POINT ( 'NONE',  ( -26.23994229802980271, -297.2467105780751240, -193.5981341315722659 ) ) ;
#47754 = CARTESIAN_POINT ( 'NONE',  ( 3.181661219328753454, -278.7294789342200261, -206.2822416791846081 ) ) ;
#47755 = CARTESIAN_POINT ( 'NONE',  ( -4.997753247498134321, -287.7843169035766664, -201.0273789015625425 ) ) ;
#47756 = CARTESIAN_POINT ( 'NONE',  ( 29.42419740904362158, -287.7842185941754565, -300.0045690794859752 ) ) ;
#47757 = CARTESIAN_POINT ( 'NONE',  ( -29.62172352023252486, -278.4728987251283456, -343.7003633859345655 ) ) ;
#47758 = CARTESIAN_POINT ( 'NONE',  ( -104.2535083699871450, -294.1322979533326247, -303.5635983049475044 ) ) ;
#47759 = CARTESIAN_POINT ( 'NONE',  ( -50.15102219760230184, -299.6465829423858054, -197.4646483878504455 ) ) ;
#47760 = CARTESIAN_POINT ( 'NONE',  ( -109.1564520441392148, -277.1481934026274416, -285.5193472089760007 ) ) ;
#47761 = ORIENTED_EDGE ( 'NONE', *, *, #44041, .T. ) ;
#47762 = CARTESIAN_POINT ( 'NONE',  ( -30.48266029254661547, -297.8025502153051889, -193.3826370686200846 ) ) ;
#47763 = CARTESIAN_POINT ( 'NONE',  ( -50.99199153367960946, -291.1479538660603339, -343.5915674354181419 ) ) ;
#47764 = CARTESIAN_POINT ( 'NONE',  ( 25.07123255647881876, -295.7366338377801185, -314.0996418343348182 ) ) ;
#47765 = CARTESIAN_POINT ( 'NONE',  ( 202.0868887437326009, 292.1662959946771139, -53.99999999997601918 ) ) ;
#47766 = CARTESIAN_POINT ( 'NONE',  ( -102.5041869584556196, -291.6542605405141444, -237.1168346312996391 ) ) ;
#47767 = CARTESIAN_POINT ( 'NONE',  ( -43.54160339317392214, -248.0334966641272558, -465.6442049081569508 ) ) ;
#47768 = CARTESIAN_POINT ( 'NONE',  ( -98.15846494899039953, -297.8328633425223870, -223.2799665494169687 ) ) ;
#47769 = CARTESIAN_POINT ( 'NONE',  ( -91.90580513875376312, -289.4238143662906850, -217.7216511321033181 ) ) ;
#47770 = CARTESIAN_POINT ( 'NONE',  ( -14.82206327796470013, -298.6601616315489878, -193.3810252821741074 ) ) ;
#47771 = DIRECTION ( 'NONE',  ( 0.000000000000000000, 1.000000000000000000, 0.000000000000000000 ) ) ;
#47772 = CARTESIAN_POINT ( 'NONE',  ( -36.07872676323889749, -290.5567359591474883, -346.6703265333196669 ) ) ;
#47773 = CARTESIAN_POINT ( 'NONE',  ( -55.56934967048406548, -279.7662352645559736, -350.3683826091709648 ) ) ;
#47774 = CARTESIAN_POINT ( 'NONE',  ( -88.97748520626691970, -287.3245327908676359, -216.1967927859187455 ) ) ;
#47775 = CARTESIAN_POINT ( 'NONE',  ( 13.86557104076155689, -285.3281008006022716, -213.5766099432649980 ) ) ;
#47776 = CARTESIAN_POINT ( 'NONE',  ( 35.29469311191165559, -273.3202936069629345, -252.3615955638833839 ) ) ;
#47777 = CARTESIAN_POINT ( 'NONE',  ( -49.12706271512227119, -275.8211213865592981, -196.8077806674050976 ) ) ;
#47778 = CARTESIAN_POINT ( 'NONE',  ( -111.0522243948232557, -288.4963238075204117, -280.8485848479246556 ) ) ;
#47779 = CARTESIAN_POINT ( 'NONE',  ( -35.71390687493809679, -278.8923790394271691, -346.1213460299987332 ) ) ;
#47780 = VECTOR ( 'NONE', #90276, 1000.000000000000000 ) ;
#47781 = ORIENTED_EDGE ( 'NONE', *, *, #12669, .F. ) ;
#47783 = CARTESIAN_POINT ( 'NONE',  ( -9.200451133116812841, -279.7786682168504626, -202.8928826909244378 ) ) ;
#47782 = CARTESIAN_POINT ( 'NONE',  ( -11.74314832479123893, -280.3948230826503050, -201.9430927547477950 ) ) ;
#47784 = CARTESIAN_POINT ( 'NONE',  ( -14.66790997642876704, -277.8448258570442135, -343.6792079792042500 ) ) ;
#47785 = CARTESIAN_POINT ( 'NONE',  ( 28.95067408403298970, -279.8453478236557430, -231.9771390454549476 ) ) ;
#47786 = CARTESIAN_POINT ( 'NONE',  ( -14.03755197167841295, -91.47614451431806515, -356.9296174414798770 ) ) ;
#47787 = CARTESIAN_POINT ( 'NONE',  ( 25.12842388375779734, -275.9003647540504858, -225.7258142996655295 ) ) ;
#47788 = CARTESIAN_POINT ( 'NONE',  ( -99.01819550539553916, -274.6749868029116328, -225.3433311945190667 ) ) ;
#47789 = CARTESIAN_POINT ( 'NONE',  ( -20.19161114001083490, -297.3376638359846424, -345.3538533559490702 ) ) ;
#47790 = EDGE_LOOP ( 'NONE', ( #45199, #72420, #42535, #87736, #79193, #26271 ) ) ;
#47791 = DIRECTION ( 'NONE',  ( 0.000000000000000000, 1.000000000000000000, 0.000000000000000000 ) ) ;
#47792 = CARTESIAN_POINT ( 'NONE',  ( 27.92711316866997251, -288.1788801405559752, -236.8694787884889479 ) ) ;
#47793 = CARTESIAN_POINT ( 'NONE',  ( 18.88966181576476799, -290.0162628869611581, -321.4883127545409707 ) ) ;
#47794 = CARTESIAN_POINT ( 'NONE',  ( -97.43742830510288400, -289.3213908267341026, -312.0051761180399694 ) ) ;
#47795 = CARTESIAN_POINT ( 'NONE',  ( 23.81633760228273289, -286.4366923169906158, -223.6573842876974254 ) ) ;
#47796 = CARTESIAN_POINT ( 'NONE',  ( 197.9084906637196468, 26.03761768678752730, 11.52973355077852524 ) ) ;
#47797 = CARTESIAN_POINT ( 'NONE',  ( 14.47199614912897836, -280.7087026063785515, -322.9857025533169121 ) ) ;
#47798 = CARTESIAN_POINT ( 'NONE',  ( 18.77455666692207714, -290.0942689705481712, -319.0367886127818338 ) ) ;
#47799 = CARTESIAN_POINT ( 'NONE',  ( -8.238070374407035601, -281.1438298552202468, -338.0640461972238882 ) ) ;
#47800 = EDGE_CURVE ( 'NONE', #63636, #9221, #19526, .T. ) ;
#47801 = CARTESIAN_POINT ( 'NONE',  ( -108.9631019788419479, -279.6506469371350363, -286.8976813401220056 ) ) ;
#47802 = CARTESIAN_POINT ( 'NONE',  ( 19.23322490027285525, -276.6987228228639424, -316.6114121402917476 ) ) ;
#47803 = CARTESIAN_POINT ( 'NONE',  ( -101.3437162637597027, -289.9043805502423652, -228.1737897792467322 ) ) ;
#47804 = CARTESIAN_POINT ( 'NONE',  ( -112.2047216655330857, -285.5719406928964759, -253.0496527733878622 ) ) ;
#47805 = CARTESIAN_POINT ( 'NONE',  ( -52.16757244290418072, -286.3597199234480968, -194.8102777431788297 ) ) ;
#47806 = CARTESIAN_POINT ( 'NONE',  ( 33.11302353964201473, -281.4658421557255110, -251.2048732497125343 ) ) ;
#47807 = VERTEX_POINT ( 'NONE', #87778 ) ;
#47808 = DIRECTION ( 'NONE',  ( 0.000000000000000000, 0.000000000000000000, 1.000000000000000000 ) ) ;
#47809 = CARTESIAN_POINT ( 'NONE',  ( -99.65106335666747839, -291.8340225229222256, -313.4638874422210506 ) ) ;
#47810 = CARTESIAN_POINT ( 'NONE',  ( -25.08384501134178990, -290.8901693776799107, -194.8426218403851067 ) ) ;
#47811 = CARTESIAN_POINT ( 'NONE',  ( 13.66911008037368269, -273.8473572301384706, -217.8129906166182934 ) ) ;
#47812 = CARTESIAN_POINT ( 'NONE',  ( -16.54243468085542901, -294.1389688019206687, -344.4480482461646034 ) ) ;
#47813 = CARTESIAN_POINT ( 'NONE',  ( -69.30093676245908796, -290.1037844213788048, -203.9445123520838479 ) ) ;
#47814 = CARTESIAN_POINT ( 'NONE',  ( -20.64101670490907736, -293.0747841058794165, -342.5184576341039246 ) ) ;
#47815 = CARTESIAN_POINT ( 'NONE',  ( -109.6707149694501169, -291.9247291296268827, -257.5948483605287720 ) ) ;
#47816 = CARTESIAN_POINT ( 'NONE',  ( 197.2116943569230045, 249.5000000000000568, -12.92446933126075592 ) ) ;
#47817 = CARTESIAN_POINT ( 'NONE',  ( -110.6060244640538741, -292.3463345844836567, -286.4029206480037715 ) ) ;
#47818 = CARTESIAN_POINT ( 'NONE',  ( -22.52952526021267587, -290.2410455688940374, -196.6152882260547301 ) ) ;
#47819 = CARTESIAN_POINT ( 'NONE',  ( 11.45536953088858745, -296.3760993425053698, -327.3835223753573018 ) ) ;
#47820 = CARTESIAN_POINT ( 'NONE',  ( 9.170723964078902668, -287.6506648680766602, -213.7925502753100773 ) ) ;
#47821 = CARTESIAN_POINT ( 'NONE',  ( 35.68509231518050484, -295.7811210911065132, -288.2228034533956702 ) ) ;
#47822 = CARTESIAN_POINT ( 'NONE',  ( -32.80731966488770013, -276.0888882189502738, -195.1295922292562182 ) ) ;
#47823 = CARTESIAN_POINT ( 'NONE',  ( 19.57185407617239292, -275.0468724302438659, -321.6531149912864294 ) ) ;
#47824 = CARTESIAN_POINT ( 'NONE',  ( -89.49119200185317879, -296.5370042798498957, -213.8568853697558723 ) ) ;
#47825 = CARTESIAN_POINT ( 'NONE',  ( 24.82349123551642478, -274.3416146429535161, -310.6235094109042620 ) ) ;
#47826 = CARTESIAN_POINT ( 'NONE',  ( 10.21492164000678748, -278.7933868655203469, -213.0253975684684917 ) ) ;
#47827 = CARTESIAN_POINT ( 'NONE',  ( -102.3894274533558786, -274.2187119351623323, -236.2521164373142142 ) ) ;
#47828 = CARTESIAN_POINT ( 'NONE',  ( -0.3149494975562946997, -273.1092464090923499, -203.5059354400994209 ) ) ;
#47829 = CARTESIAN_POINT ( 'NONE',  ( -107.4249011044205275, -297.6802210614119417, -292.9696548112023038 ) ) ;
#47830 = CARTESIAN_POINT ( 'NONE',  ( 199.5308170082005290, 67.35660163418374680, 10.35296668938518216 ) ) ;
#47831 = CARTESIAN_POINT ( 'NONE',  ( -70.54996040007995362, -298.4055021964833827, -205.1565836681555481 ) ) ;
#47832 = CARTESIAN_POINT ( 'NONE',  ( 169.8384340989974532, 249.5000000000000568, -24.41176470588233727 ) ) ;
#47834 = CARTESIAN_POINT ( 'NONE',  ( -106.3056896592338632, -272.7038119997216086, -246.4243648099739232 ) ) ;
#47833 = CARTESIAN_POINT ( 'NONE',  ( 2.293104917632814654, -286.5445401989034053, -334.5120132109231577 ) ) ;
#47835 = CARTESIAN_POINT ( 'NONE',  ( 38.97527028884086775, -287.4241708756740650, -260.1278376491272866 ) ) ;
#47836 = CARTESIAN_POINT ( 'NONE',  ( -8.245058753504640237, -288.3481472887648920, -341.6433934503226055 ) ) ;
#47837 = CARTESIAN_POINT ( 'NONE',  ( -96.94876041265688116, -299.1611270003007803, -224.2381665219304807 ) ) ;
#47838 = CARTESIAN_POINT ( 'NONE',  ( -68.07075690856088102, -293.4563744284378686, -338.6082530300341205 ) ) ;
#47839 = CARTESIAN_POINT ( 'NONE',  ( 3.744286426782932331, -279.7868918598464347, -205.3667571429196812 ) ) ;
#47840 = CARTESIAN_POINT ( 'NONE',  ( 152.6524812969444724, 129.6175404775655409, -12.50000000000000000 ) ) ;
#47841 = CARTESIAN_POINT ( 'NONE',  ( -97.17354021324520374, -277.1706422857423604, -225.1168075251522964 ) ) ;
#47842 = CARTESIAN_POINT ( 'NONE',  ( 201.2029632875019729, 287.9274539447415577, -5.251267118318729388 ) ) ;
#47843 = CARTESIAN_POINT ( 'NONE',  ( -58.81990368103672751, -288.1310301383136334, -340.5983800547072633 ) ) ;
#47844 = CARTESIAN_POINT ( 'NONE',  ( 196.0143093133015384, 42.36571313990103249, 11.99999999999998757 ) ) ;
#47845 = CARTESIAN_POINT ( 'NONE',  ( 30.28173832083462358, 95.44497268212424501, 10.00000000000000000 ) ) ;
#47846 = CARTESIAN_POINT ( 'NONE',  ( -102.8587301140240982, -289.0390828466231596, -233.7508212618621144 ) ) ;
#47847 = CARTESIAN_POINT ( 'NONE',  ( -110.8820953015494268, -274.1438931321728205, -264.8809920944484588 ) ) ;
#47848 = CARTESIAN_POINT ( 'NONE',  ( 15.36035717930338862, -283.7500232587835285, -325.6883214846540682 ) ) ;
#47850 = CARTESIAN_POINT ( 'NONE',  ( -92.55912865390867239, -283.8716113710611921, -318.1298587852643323 ) ) ;
#47849 = CARTESIAN_POINT ( 'NONE',  ( -105.5329531306852715, -271.0572056691246985, -237.8147324832247023 ) ) ;
#47851 = CARTESIAN_POINT ( 'NONE',  ( -6.296779724573521975, -275.8934980145440363, -203.6408973889737979 ) ) ;
#47852 = CARTESIAN_POINT ( 'NONE',  ( 34.99978909241605862, -276.2101060891602060, -259.3539608691125409 ) ) ;
#47853 = CARTESIAN_POINT ( 'NONE',  ( -41.43385859670913618, -285.1037115942406786, -345.3003689542235861 ) ) ;
#47854 = CARTESIAN_POINT ( 'NONE',  ( -107.4882964293772147, -271.7553894491489928, -248.8875465601180395 ) ) ;
#47855 = ORIENTED_EDGE ( 'NONE', *, *, #63702, .T. ) ;
#47856 = CARTESIAN_POINT ( 'NONE',  ( 202.9738562182569694, 293.9636489450776367, -44.00000000000000000 ) ) ;
#47857 = CARTESIAN_POINT ( 'NONE',  ( 37.08313043890141358, -293.1376742429494584, -250.5632276277583514 ) ) ;
#47858 = CARTESIAN_POINT ( 'NONE',  ( -111.6340153215883646, -286.6321279601000924, -262.6036241156826350 ) ) ;
#47859 = DIRECTION ( 'NONE',  ( -0.000000000000000000, 0.000000000000000000, 1.000000000000000000 ) ) ;
#47860 = CARTESIAN_POINT ( 'NONE',  ( 25.22466315766302358, -278.4094976428775681, -220.5068182859052968 ) ) ;
#47861 = CARTESIAN_POINT ( 'NONE',  ( -45.64235679010576519, -276.3518492002178277, -346.8029253531821041 ) ) ;
#47862 = CARTESIAN_POINT ( 'NONE',  ( -112.3806290127888019, -289.1194952750862512, -257.1097192530816073 ) ) ;
#47863 = CARTESIAN_POINT ( 'NONE',  ( 10.37220342581547250, -283.9000699950152580, -326.5895365445584275 ) ) ;
#47864 = CARTESIAN_POINT ( 'NONE',  ( -21.41339368267877319, -278.6053847980942919, -342.6928996487774270 ) ) ;
#47865 = CARTESIAN_POINT ( 'NONE',  ( -33.07337690516038009, -284.4246778165598357, -346.6656178578430172 ) ) ;
#47866 = CARTESIAN_POINT ( 'NONE',  ( -16.03179388071970735, -281.5652572259400586, -340.5965677191549617 ) ) ;
#47867 = CARTESIAN_POINT ( 'NONE',  ( -77.92492234900896619, -281.5074748229842498, -207.2277857257063829 ) ) ;
#47868 = CARTESIAN_POINT ( 'NONE',  ( 23.63154151060813746, -275.0910173866198534, -223.3155802605577946 ) ) ;
#47869 = CARTESIAN_POINT ( 'NONE',  ( -59.66703806442128410, -277.1668859834958312, -344.0535822548152396 ) ) ;
#47870 = ADVANCED_FACE ( 'NONE', ( #16760 ), #88252, .T. ) ;
#47871 = CARTESIAN_POINT ( 'NONE',  ( -109.3565713551685974, -298.2277058942799499, -289.2574722428213363 ) ) ;
#47872 = CARTESIAN_POINT ( 'NONE',  ( 156.4947056272797852, 20.00000000000000000, -15.00000000000000000 ) ) ;
#47873 = CARTESIAN_POINT ( 'NONE',  ( 169.2744399300530347, 8.542400036368780647, -9.000000000000001776 ) ) ;
#47874 = CARTESIAN_POINT ( 'NONE',  ( -103.5354707400467049, -294.2048701747056612, -307.3288421930412824 ) ) ;
#47875 = CARTESIAN_POINT ( 'NONE',  ( 19.22525981777495829, -275.7141878156453458, -316.6211532478974959 ) ) ;
#47876 = CARTESIAN_POINT ( 'NONE',  ( 19.09207634808648280, -299.8228228643003490, -193.6601402860643759 ) ) ;
#47877 = CARTESIAN_POINT ( 'NONE',  ( 27.24079331655068259, -288.8232758816945420, -234.1028129773707178 ) ) ;
#47878 = CARTESIAN_POINT ( 'NONE',  ( -76.70780334520587473, -297.0887118748589160, -335.7909046014019054 ) ) ;
#47879 = CARTESIAN_POINT ( 'NONE',  ( 37.07793189106546805, -294.9861650061301930, -288.5744393602686273 ) ) ;
#47880 = CARTESIAN_POINT ( 'NONE',  ( -95.51375768354770912, -291.9027365835846695, -317.4359536251132567 ) ) ;
#47881 = CARTESIAN_POINT ( 'NONE',  ( -94.47378737337868415, -277.2222716851174482, -222.0097174547422298 ) ) ;
#47882 = CARTESIAN_POINT ( 'NONE',  ( -111.5967618395086021, -280.5401514404231875, -265.1170731771273950 ) ) ;
#47883 = CARTESIAN_POINT ( 'NONE',  ( -111.5366246619025929, -294.5460533690520037, -277.0042905862908356 ) ) ;
#47884 = CARTESIAN_POINT ( 'NONE',  ( 3.893629279626806827, -284.3641351983017671, -333.9837616488585468 ) ) ;
#47885 = CARTESIAN_POINT ( 'NONE',  ( 0.3392986430308853052, -285.4868086662958149, -207.4181615756862413 ) ) ;
#47886 = CARTESIAN_POINT ( 'NONE',  ( -110.6519398798504454, -271.9518965266826740, -296.2779929517423625 ) ) ;
#47887 = ORIENTED_EDGE ( 'NONE', *, *, #21988, .F. ) ;
#47888 = CARTESIAN_POINT ( 'NONE',  ( -94.13580901942997059, -284.8679763692716165, -224.4444974290897790 ) ) ;
#47889 = ORIENTED_EDGE ( 'NONE', *, *, #77831, .F. ) ;
#47890 = AXIS2_PLACEMENT_3D ( 'NONE', #33112, #62000, #5187 ) ;
#47891 = CARTESIAN_POINT ( 'NONE',  ( 9.032857052580727242, -283.5118974878466247, -331.4421539527042455 ) ) ;
#47892 = CARTESIAN_POINT ( 'NONE',  ( -69.50409694271554883, -273.9499993768540094, -204.8045186350234133 ) ) ;
#47893 = CARTESIAN_POINT ( 'NONE',  ( -35.14417093109853596, -284.8740661733422144, -193.7766406045116980 ) ) ;
#47894 = CARTESIAN_POINT ( 'NONE',  ( 6.041379444771633800, -281.5664161416378306, -207.0308043942508505 ) ) ;
#47895 = EDGE_CURVE ( 'NONE', #86001, #41734, #3483, .T. ) ;
#47896 = CARTESIAN_POINT ( 'NONE',  ( 196.4287260171921332, 19.73406386204618457, -13.26569520083611842 ) ) ;
#47897 = CARTESIAN_POINT ( 'NONE',  ( -68.40813783438576934, -281.1715163391167494, -200.6504883552492231 ) ) ;
#47898 = CARTESIAN_POINT ( 'NONE',  ( 20.11007591016628382, -281.1904247046184082, -219.1061771533815943 ) ) ;
#47899 = CARTESIAN_POINT ( 'NONE',  ( 17.36665895637873192, -279.6952119285918457, -314.0302885647153062 ) ) ;
#47900 = CARTESIAN_POINT ( 'NONE',  ( 162.1785412711766128, 219.9095514846544290, -205.3156639783633750 ) ) ;
#47901 = ORIENTED_EDGE ( 'NONE', *, *, #15031, .T. ) ;
#47902 = CARTESIAN_POINT ( 'NONE',  ( -10.86481649574293229, -276.3981916849856475, -200.3128440212580301 ) ) ;
#47903 = CARTESIAN_POINT ( 'NONE',  ( -22.71367860124261639, -107.9710121992093548, -362.4982422966238573 ) ) ;
#47904 = CARTESIAN_POINT ( 'NONE',  ( -1.146933343844307229, -278.5550833281416203, -205.0787646125536696 ) ) ;
#47905 = CARTESIAN_POINT ( 'NONE',  ( -19.64482113742459291, -294.0366858884390808, -196.4098327872376899 ) ) ;
#47906 = CARTESIAN_POINT ( 'NONE',  ( -18.20178933767734719, -294.1474459971979059, -340.9129179794224456 ) ) ;
#47907 = CARTESIAN_POINT ( 'NONE',  ( -3.342891669507786823, -291.9966977106649324, -201.3276957806842802 ) ) ;
#47908 = CARTESIAN_POINT ( 'NONE',  ( 189.9243309297870610, 249.5000000000000568, 20.22542485937349355 ) ) ;
#47910 = CARTESIAN_POINT ( 'NONE',  ( 33.80588292249433380, -285.6957415018386541, -250.7534194303607364 ) ) ;
#47909 = CARTESIAN_POINT ( 'NONE',  ( -81.54573278372066625, -294.2150394297707408, -332.7523903131476573 ) ) ;
#47911 = CARTESIAN_POINT ( 'NONE',  ( 36.65756893977778219, -295.4892897801606182, -276.2749708596793425 ) ) ;
#47912 = CARTESIAN_POINT ( 'NONE',  ( -93.79016869040778204, -285.2039898738940451, -317.4229270886758059 ) ) ;
#47913 = ORIENTED_EDGE ( 'NONE', *, *, #64946, .F. ) ;
#47914 = CARTESIAN_POINT ( 'NONE',  ( -81.80388354382461102, -292.4039162023991594, -207.7836902768522691 ) ) ;
#47915 = CARTESIAN_POINT ( 'NONE',  ( -18.71389996809472223, -283.2982057526010635, -341.0605314025556822 ) ) ;
#47916 = CARTESIAN_POINT ( 'NONE',  ( -111.2349347311150467, -295.6035471771603511, -249.9712368565271845 ) ) ;
#47917 = CARTESIAN_POINT ( 'NONE',  ( -99.90552625284237820, -291.9470480884953076, -225.7525259700396987 ) ) ;
#47918 = CARTESIAN_POINT ( 'NONE',  ( -61.67506738337655037, -292.2367252449123498, -197.3158671677418567 ) ) ;
#47919 = CARTESIAN_POINT ( 'NONE',  ( 19.51482190470161626, -288.3661586537534731, -316.1468789446202550 ) ) ;
#47920 = ORIENTED_EDGE ( 'NONE', *, *, #92, .F. ) ;
#47921 = DIRECTION ( 'NONE',  ( 0.000000000000000000, 0.000000000000000000, -1.000000000000000000 ) ) ;
#47922 = CARTESIAN_POINT ( 'NONE',  ( -108.2726552023081581, -298.0685278649633005, -297.1380371930032425 ) ) ;
#47923 = CARTESIAN_POINT ( 'NONE',  ( -87.12856187305669664, -296.0606127347402889, -212.2002718345608230 ) ) ;
#47924 = EDGE_CURVE ( 'NONE', #10890, #4223, #53199, .T. ) ;
#47925 = CARTESIAN_POINT ( 'NONE',  ( -49.16813861137797659, -278.9564720564790150, -198.0870299540867734 ) ) ;
#47926 = CARTESIAN_POINT ( 'NONE',  ( 38.15957044152528965, -274.8745458836051512, -255.5595962432047941 ) ) ;
#47927 = CARTESIAN_POINT ( 'NONE',  ( -109.4536042943176142, -295.2312333953454981, -255.1156266051811201 ) ) ;
#47928 = CARTESIAN_POINT ( 'NONE',  ( -85.89553235068845538, -279.5931342318965562, -326.5842523410223635 ) ) ;
#47929 = CARTESIAN_POINT ( 'NONE',  ( 35.04339195995451917, -273.4774186380431615, -253.8341104500827612 ) ) ;
#47930 = CARTESIAN_POINT ( 'NONE',  ( -61.12741337681901399, -296.5728920410757041, -339.8510678751912337 ) ) ;
#47931 = CARTESIAN_POINT ( 'NONE',  ( -108.4782262616793105, -297.8652225752066443, -252.5946998227687175 ) ) ;
#47932 = DIRECTION ( 'NONE',  ( -0.000000000000000000, -1.000000000000000000, 0.000000000000000000 ) ) ;
#47933 = CARTESIAN_POINT ( 'NONE',  ( -108.1528092270744565, -298.5146699405961499, -242.0726934031937674 ) ) ;
#47934 = CARTESIAN_POINT ( 'NONE',  ( -54.15960630100301643, -295.8364965095256593, -197.1000338014080739 ) ) ;
#47935 = CARTESIAN_POINT ( 'NONE',  ( 10.99199535900419100, -293.3932271740039823, -215.4506523899968897 ) ) ;
#47936 = CARTESIAN_POINT ( 'NONE',  ( -108.9277979490158543, -288.9037021465399562, -287.4141387637314438 ) ) ;
#47937 = DIRECTION ( 'NONE',  ( 0.000000000000000000, 1.000000000000000000, 0.000000000000000000 ) ) ;
#47938 = CARTESIAN_POINT ( 'NONE',  ( 7.194257009148517845, -275.1330625948261286, -207.5575897496810001 ) ) ;
#47939 = CARTESIAN_POINT ( 'NONE',  ( -76.56601569282112507, -273.6778074237018927, -208.7944624539895244 ) ) ;
#47940 = CARTESIAN_POINT ( 'NONE',  ( 5.233733975371583469, -282.6048890810330363, -208.1860489321172167 ) ) ;
#47941 = CARTESIAN_POINT ( 'NONE',  ( 22.12928338929965832, -280.8867588966585345, -318.5118181721572341 ) ) ;
#47942 = EDGE_CURVE ( 'NONE', #74899, #52690, #57342, .T. ) ;
#47943 = CARTESIAN_POINT ( 'NONE',  ( -72.80106846456230585, -276.8578910992707733, -338.6102955469083327 ) ) ;
#47944 = CARTESIAN_POINT ( 'NONE',  ( -110.1540600138141315, -283.8498515584774395, -262.7230530015149839 ) ) ;
#47945 = CARTESIAN_POINT ( 'NONE',  ( 20.18997449898513707, -280.2192876561621233, -318.7360582357040357 ) ) ;
#47946 = CARTESIAN_POINT ( 'NONE',  ( -68.51580212926013758, -272.2090690184517143, -203.6873507035834621 ) ) ;
#47947 = CARTESIAN_POINT ( 'NONE',  ( -29.51147819262562066, -278.9532711824034550, -345.0022699460427589 ) ) ;
#47948 = DIRECTION ( 'NONE',  ( 0.9693563597868444237, 0.2456588035076248677, -0.000000000000000000 ) ) ;
#47949 = DIRECTION ( 'NONE',  ( -0.9531768234071980039, 0.3024135303179465994, 0.000000000000000000 ) ) ;
#47950 = CARTESIAN_POINT ( 'NONE',  ( 74.55052467484399870, -297.6744934986045905, -194.4074022689418086 ) ) ;
#47951 = CARTESIAN_POINT ( 'NONE',  ( -4.765771754016490114, -278.6242992926111697, -338.1162318610784041 ) ) ;
#47952 = CARTESIAN_POINT ( 'NONE',  ( -29.76311809300124978, -272.1479549999277197, -195.7449954456092485 ) ) ;
#47953 = FACE_OUTER_BOUND ( 'NONE', #54918, .T. ) ;
#47954 = CARTESIAN_POINT ( 'NONE',  ( -111.1137661218266288, -286.2640516088807772, -286.7011449547217126 ) ) ;
#47955 = ORIENTED_EDGE ( 'NONE', *, *, #73884, .T. ) ;
#47956 = CARTESIAN_POINT ( 'NONE',  ( 200.2349812190172713, 66.43136063442170780, 7.741079165001062634 ) ) ;
#47957 = CARTESIAN_POINT ( 'NONE',  ( 20.22899615849963695, -286.2161809148599332, -318.4496845795161448 ) ) ;
#47958 = CARTESIAN_POINT ( 'NONE',  ( 206.5090647127522629, 29.77167987842737773, 13.94198228246500548 ) ) ;
#47959 = CARTESIAN_POINT ( 'NONE',  ( -37.00907922970003483, -293.8427857833765415, -343.7699299751866988 ) ) ;
#47960 = CARTESIAN_POINT ( 'NONE',  ( 25.26760187291327142, -286.2340869954373375, -310.2477170166627616 ) ) ;
#47961 = CARTESIAN_POINT ( 'NONE',  ( 201.7194887906492795, 294.2213704821156739, -83.28174295417332473 ) ) ;
#47962 = CARTESIAN_POINT ( 'NONE',  ( -100.4290682116322841, -294.0045845161777720, -311.0147151388366638 ) ) ;
#47963 = CARTESIAN_POINT ( 'NONE',  ( -10.22210209114956569, -284.8795340388236923, -198.9799659732566965 ) ) ;
#47964 = CARTESIAN_POINT ( 'NONE',  ( 3.125813926382862817, -282.2053889370845354, -208.5841649242665596 ) ) ;
#47965 = CARTESIAN_POINT ( 'NONE',  ( 16.52085195812075469, -279.0444582799065643, -216.6888108236538812 ) ) ;
#47966 = CARTESIAN_POINT ( 'NONE',  ( 17.82553026358253945, -288.2341536596968581, -318.2445072733001439 ) ) ;
#47967 = CARTESIAN_POINT ( 'NONE',  ( -110.2078586681560068, -280.1167286527313536, -259.7162629346179301 ) ) ;
#47968 = CARTESIAN_POINT ( 'NONE',  ( -76.91778337390783804, -280.3103398369945580, -208.7675153864627191 ) ) ;
#47969 = CARTESIAN_POINT ( 'NONE',  ( 36.93130988676805515, -289.3684563766395286, -257.5603081369066558 ) ) ;
#47970 = ORIENTED_EDGE ( 'NONE', *, *, #66104, .T. ) ;
#47971 = CARTESIAN_POINT ( 'NONE',  ( -49.71923897398222891, -273.8985981582165437, -194.3086511941902472 ) ) ;
#47972 = CARTESIAN_POINT ( 'NONE',  ( -83.54504528438066302, -291.6693604290020403, -328.9878840192811822 ) ) ;
#47973 = CARTESIAN_POINT ( 'NONE',  ( 197.2116943569230330, 276.0000000000000568, -12.92446933126074882 ) ) ;
#47974 = CARTESIAN_POINT ( 'NONE',  ( -88.47809603358389552, -292.1948066931273615, -334.5364918783848793 ) ) ;
#47975 = VERTEX_POINT ( 'NONE', #74515 ) ;
#47976 = CARTESIAN_POINT ( 'NONE',  ( 34.83287086736124394, -273.2801550703312614, -249.1823495373240576 ) ) ;
#47977 = DIRECTION ( 'NONE',  ( 0.000000000000000000, 0.000000000000000000, 1.000000000000000000 ) ) ;
#47978 = CARTESIAN_POINT ( 'NONE',  ( -37.70582191463291366, -293.4564829181189793, -346.5731929530072648 ) ) ;
#47979 = CARTESIAN_POINT ( 'NONE',  ( -110.4433243138642950, -271.9367760107406866, -267.6251805984415455 ) ) ;
#47980 = CARTESIAN_POINT ( 'NONE',  ( -0.6293907000458592860, -290.0754301642651285, -334.3175481656742818 ) ) ;
#47981 = CARTESIAN_POINT ( 'NONE',  ( -37.52077331648934688, -284.8146010123085716, -344.3868395776810871 ) ) ;
#47982 = CARTESIAN_POINT ( 'NONE',  ( -96.81989079904772666, -291.3291805808991626, -318.3499770783621443 ) ) ;
#47983 = CARTESIAN_POINT ( 'NONE',  ( -111.8409139349781753, -292.0864858177499741, -252.9494719604173270 ) ) ;
#47984 = CARTESIAN_POINT ( 'NONE',  ( -33.15171718094730835, -288.1049510643959479, -195.4270590555443334 ) ) ;
#47985 = CARTESIAN_POINT ( 'NONE',  ( -99.42912640366540700, -279.3239181208564332, -224.7960109422399171 ) ) ;
#47986 = CARTESIAN_POINT ( 'NONE',  ( -112.2289013216337707, -294.4988804527592379, -280.8061139300600644 ) ) ;
#47987 = CARTESIAN_POINT ( 'NONE',  ( -5.457456127174665994, -282.4774799173404745, -340.4495976994124931 ) ) ;
#47988 = CARTESIAN_POINT ( 'NONE',  ( 8.068106416014980908, -276.5409992106419281, -211.6345060669696636 ) ) ;
#47989 = CARTESIAN_POINT ( 'NONE',  ( -67.68488546085839630, -279.9805209788415823, -333.4427485647536855 ) ) ;
#47990 = CARTESIAN_POINT ( 'NONE',  ( 21.98149345425066770, -273.1473032778117158, -222.8564501972736878 ) ) ;
#47991 = LINE ( 'NONE', #71208, #83307 ) ;
#47992 = CARTESIAN_POINT ( 'NONE',  ( 4.963885067016563291, -280.1490989473991249, -210.7941312970201579 ) ) ;
#47993 = CARTESIAN_POINT ( 'NONE',  ( -67.53788651524465081, -278.6446593559310827, -340.7613953044958066 ) ) ;
#47994 = CARTESIAN_POINT ( 'NONE',  ( -43.63498782813222476, -285.0333618627391843, -193.8017165078334756 ) ) ;
#47995 = CARTESIAN_POINT ( 'NONE',  ( -69.47758036835661244, -293.3835163385631972, -203.6743444191989454 ) ) ;
#47996 = CARTESIAN_POINT ( 'NONE',  ( 33.44869771128058744, -277.5153814249955531, -298.7020541683110650 ) ) ;
#47997 = CARTESIAN_POINT ( 'NONE',  ( 37.15087949335197237, -276.6471502468564267, -252.8641767520707901 ) ) ;
#47998 = LINE ( 'NONE', #26238, #590 ) ;
#47999 = CARTESIAN_POINT ( 'NONE',  ( 35.02078894712537505, -275.2584812730623867, -260.7345828143970721 ) ) ;
#48000 = CARTESIAN_POINT ( 'NONE',  ( -106.6505480030534869, -298.1835524515751672, -298.5801192096504906 ) ) ;
#48001 = CARTESIAN_POINT ( 'NONE',  ( -41.39744745795693603, -284.0008302525749855, -195.6249535250933320 ) ) ;
#48002 = CARTESIAN_POINT ( 'NONE',  ( -3.326869704139062911, -292.1557379576537414, -201.2905514753320517 ) ) ;
#48003 = CARTESIAN_POINT ( 'NONE',  ( 32.66956441985474413, -273.2346496894775782, -244.4715517938489597 ) ) ;
#48004 = CARTESIAN_POINT ( 'NONE',  ( 36.73160915207652977, -289.3788587385673736, -288.2932505926635258 ) ) ;
#48005 = CARTESIAN_POINT ( 'NONE',  ( -12.14108662838064490, -291.3081128841067198, -201.4654860045028215 ) ) ;
#48006 = ORIENTED_EDGE ( 'NONE', *, *, #33276, .F. ) ;
#48007 = CARTESIAN_POINT ( 'NONE',  ( -6.111030253669516910, -291.0292877846311512, -200.6099199626615359 ) ) ;
#48008 = CARTESIAN_POINT ( 'NONE',  ( 31.82243232952892242, -292.9059329285202011, -246.7855275763157010 ) ) ;
#48009 = ORIENTED_EDGE ( 'NONE', *, *, #1783, .T. ) ;
#48010 = CARTESIAN_POINT ( 'NONE',  ( 36.84888617535978739, -288.8759228471411689, -289.7840275117691249 ) ) ;
#48011 = CARTESIAN_POINT ( 'NONE',  ( -83.45437583940538673, -279.7332126978419069, -213.6766918098673216 ) ) ;
#48012 = CARTESIAN_POINT ( 'NONE',  ( -2.121727771319923850, -293.5172180888884554, -338.4863413428971626 ) ) ;
#48013 = CARTESIAN_POINT ( 'NONE',  ( -108.9366198916925725, -285.5613768696180159, -242.1541868155274244 ) ) ;
#48014 = EDGE_CURVE ( 'NONE', #86239, #29030, #4386, .T. ) ;
#48015 = CARTESIAN_POINT ( 'NONE',  ( 31.40100667542650115, -287.4395159495108487, -235.7174381439086801 ) ) ;
#48016 = CARTESIAN_POINT ( 'NONE',  ( -4.813932744860490942, -282.9447479105849084, -335.7371979807689399 ) ) ;
#48017 = CARTESIAN_POINT ( 'NONE',  ( 84.71888943659025983, 83.26956024130151945, -302.3639758324752620 ) ) ;
#48018 = CARTESIAN_POINT ( 'NONE',  ( 201.7738562182570092, 295.5636489450776594, -54.00000000002855671 ) ) ;
#48019 = CARTESIAN_POINT ( 'NONE',  ( -89.56232258695946769, -229.0018711643211873, -344.4782180464590624 ) ) ;
#48020 = CARTESIAN_POINT ( 'NONE',  ( 19.30012945229858801, -275.4037526847995991, -316.6874952372622261 ) ) ;
#48021 = CARTESIAN_POINT ( 'NONE',  ( 5.566627113730801213, -275.3762787172482831, -329.8636949792805240 ) ) ;
#48022 = CARTESIAN_POINT ( 'NONE',  ( -36.89101025102353759, -297.5653089202770047, -193.4226924278395643 ) ) ;
#48023 = CARTESIAN_POINT ( 'NONE',  ( -106.8704548483795662, -265.5134191007825279, -305.6964246945746595 ) ) ;
#48024 = CARTESIAN_POINT ( 'NONE',  ( 36.11711466448170427, -273.9650309417401672, -248.7959255013256268 ) ) ;
#48025 = CARTESIAN_POINT ( 'NONE',  ( -35.12482235915464202, -299.9406049207471483, -196.1251986654955601 ) ) ;
#48026 = VERTEX_POINT ( 'NONE', #38048 ) ;
#48027 = CARTESIAN_POINT ( 'NONE',  ( -37.61887856930841423, -298.9900076597199359, -193.5969115689300395 ) ) ;
#48028 = CARTESIAN_POINT ( 'NONE',  ( 27.71007851628496255, -287.5916504390248747, -236.9891850880193545 ) ) ;
#48029 = CARTESIAN_POINT ( 'NONE',  ( -110.6426745841473718, -297.0642769011980135, -293.4513091504965132 ) ) ;
#48030 = CARTESIAN_POINT ( 'NONE',  ( -113.5416880409491398, -297.1787943969002868, -259.6314414746778994 ) ) ;
#48031 = CARTESIAN_POINT ( 'NONE',  ( -68.51541026052402117, -295.6401757805547277, -336.3839378876151045 ) ) ;
#48032 = ORIENTED_EDGE ( 'NONE', *, *, #87216, .T. ) ;
#48033 = CARTESIAN_POINT ( 'NONE',  ( 31.23566484959737721, -277.0572388499058434, -238.5118658668309308 ) ) ;
#48034 = ADVANCED_FACE ( 'NONE', ( #2096 ), #30987, .F. ) ;
#48035 = ORIENTED_EDGE ( 'NONE', *, *, #19214, .T. ) ;
#48036 = CARTESIAN_POINT ( 'NONE',  ( -22.57184574353276929, -279.7438706481457302, -194.7994333121657462 ) ) ;
#48037 = CARTESIAN_POINT ( 'NONE',  ( -29.67691765190060238, -277.8941220625322330, -343.2452823305832794 ) ) ;
#48038 = CARTESIAN_POINT ( 'NONE',  ( -59.34981832276312730, -279.0933969597007831, -343.0908694280910822 ) ) ;
#48039 = CARTESIAN_POINT ( 'NONE',  ( -72.10481659460799619, -275.5296269296171658, -337.2330637282659609 ) ) ;
#48040 = CARTESIAN_POINT ( 'NONE',  ( -99.98842297843262372, -297.7223751282335229, -232.5893165343579199 ) ) ;
#48041 = CARTESIAN_POINT ( 'NONE',  ( -47.89533903294519490, -293.7635801623702037, -343.2413491619556112 ) ) ;
#48042 = CARTESIAN_POINT ( 'NONE',  ( 6.111556883886342995, -24.11587310938936568, 10.00000000000000000 ) ) ;
#48043 = CARTESIAN_POINT ( 'NONE',  ( -3.690190207552459523, -280.9766746888126363, -201.1577200415365780 ) ) ;
#48044 = CARTESIAN_POINT ( 'NONE',  ( -96.40695242730352277, -279.3191981735195100, -227.4624469617730824 ) ) ;
#48045 = CARTESIAN_POINT ( 'NONE',  ( -65.28262918174078777, -288.0945011380483720, -341.6393129022759467 ) ) ;
#48046 = CARTESIAN_POINT ( 'NONE',  ( 17.68567777649750639, -300.7396324122937017, -195.1757337735481599 ) ) ;
#48047 = DIRECTION ( 'NONE',  ( 0.000000000000000000, 1.000000000000000000, 0.000000000000000000 ) ) ;
#48048 = CARTESIAN_POINT ( 'NONE',  ( -72.44530278041899862, -288.7266332883917812, -334.5509832891495421 ) ) ;
#48049 = CARTESIAN_POINT ( 'NONE',  ( -19.26567184807625921, -278.5276300636957671, -198.5360193753688236 ) ) ;
#48051 = CARTESIAN_POINT ( 'NONE',  ( -18.39221623408244710, -280.8860927168760782, -342.4022665048565841 ) ) ;
#48050 = CARTESIAN_POINT ( 'NONE',  ( -9.003806268212764863, -279.0049341340961746, -202.4469170409232675 ) ) ;
#48052 = CARTESIAN_POINT ( 'NONE',  ( -108.2281543000945447, -286.8711772596206515, -245.7075857765453009 ) ) ;
#48053 = CARTESIAN_POINT ( 'NONE',  ( -91.60064415723140030, -280.4621314098903895, -220.9334182781018967 ) ) ;
#48054 = CARTESIAN_POINT ( 'NONE',  ( 153.1901962297478974, 19.73438857712020678, -11.80184082122059230 ) ) ;
#48055 = B_SPLINE_CURVE_WITH_KNOTS ( 'NONE', 3,
 ( #7914, #50552, #80351, #29718, #42984, #80820, #37265, #23052, #79895, #87441 ),
 .UNSPECIFIED., .F., .F.,
 ( 4, 2, 2, 2, 4 ),
 ( 0.000000000000000000, 0.0005225403654565069023, 0.001045080730913013805, 0.001567621096369520815, 0.002090161461826027609 ),
 .UNSPECIFIED. ) ;
#48056 = CARTESIAN_POINT ( 'NONE',  ( -68.80792055221564851, -293.6387011374982308, -202.2672117711913984 ) ) ;
#48057 = CARTESIAN_POINT ( 'NONE',  ( -59.39264490937714669, -275.5736814032318307, -343.0778962806397772 ) ) ;
#48058 = CARTESIAN_POINT ( 'NONE',  ( -48.61538653169022695, -277.8507698712830916, -342.6399734491885738 ) ) ;
#48059 = CARTESIAN_POINT ( 'NONE',  ( -84.92173646965555633, -285.7069368868990864, -328.5519124882036976 ) ) ;
#48060 = LINE ( 'NONE', #12093, #12633 ) ;
#48061 = CARTESIAN_POINT ( 'NONE',  ( -95.27101627565203046, -291.8067263863546259, -318.8941511515985212 ) ) ;
#48062 = CARTESIAN_POINT ( 'NONE',  ( -34.10445267766981914, -293.0114124838975158, -345.3414397977035151 ) ) ;
#48063 = CARTESIAN_POINT ( 'NONE',  ( -10.04174880431190964, -285.5967077281547404, -198.4791486451182152 ) ) ;
#48064 = CARTESIAN_POINT ( 'NONE',  ( 199.2296996224750387, 68.12454877777268791, 4.237361107270380067 ) ) ;
#48065 = CARTESIAN_POINT ( 'NONE',  ( -11.29990959133293948, -273.0833919180785756, -201.5821161541705351 ) ) ;
#48066 = CARTESIAN_POINT ( 'NONE',  ( 33.51891289664124685, -291.9800899656913202, -292.4889059963347790 ) ) ;
#48067 = CARTESIAN_POINT ( 'NONE',  ( 195.5098045679252721, 40.07219932029098430, 14.92550485056066911 ) ) ;
#48068 = DIRECTION ( 'NONE',  ( -0.000000000000000000, -0.000000000000000000, 1.000000000000000000 ) ) ;
#48069 = CARTESIAN_POINT ( 'NONE',  ( -108.8175379687289848, -289.3747428906872301, -243.4915026439281291 ) ) ;
#48070 = CARTESIAN_POINT ( 'NONE',  ( -57.63370431021008500, -287.3860382586756259, -199.3524795963443523 ) ) ;
#48071 = CARTESIAN_POINT ( 'NONE',  ( 27.84098234845882658, -285.2747797586742422, -231.2058855243546986 ) ) ;
#48072 = CARTESIAN_POINT ( 'NONE',  ( -97.85069855169591335, -286.5564883452727827, -228.4576230561168302 ) ) ;
#48073 = FACE_OUTER_BOUND ( 'NONE', #52174, .T. ) ;
#48074 = CARTESIAN_POINT ( 'NONE',  ( -49.45831668519996782, -286.6966947771290393, -198.1583483162472703 ) ) ;
#48075 = CARTESIAN_POINT ( 'NONE',  ( -1.606573172722747245, -294.5033311058045342, -204.0180135460299198 ) ) ;
#48076 = CARTESIAN_POINT ( 'NONE',  ( -8.458142772784642105, -274.7568828119530053, -340.1967224366917435 ) ) ;
#48077 = CARTESIAN_POINT ( 'NONE',  ( 24.35325641475179737, -276.4980245334587039, -316.3988919163520563 ) ) ;
#48078 = CARTESIAN_POINT ( 'NONE',  ( -3.935541531651221892, -290.5691221803448911, -202.5726450811971802 ) ) ;
#48079 = CARTESIAN_POINT ( 'NONE',  ( -109.6061909089342947, -278.8899014647486183, -243.6206563244084577 ) ) ;
#48080 = CARTESIAN_POINT ( 'NONE',  ( -112.0203564984756213, -298.5532047190371259, -268.7213695911513014 ) ) ;
#48081 = CARTESIAN_POINT ( 'NONE',  ( -48.18343439338451617, -250.1980903302585091, -483.8542798561345535 ) ) ;
#48082 = DIRECTION ( 'NONE',  ( -0.000000000000000000, -0.000000000000000000, -1.000000000000000000 ) ) ;
#48083 = CARTESIAN_POINT ( 'NONE',  ( -65.26517844446927086, -284.3643501987942841, -202.3251699399052939 ) ) ;
#48084 = CARTESIAN_POINT ( 'NONE',  ( -103.2416664613760418, -277.1501380423098908, -236.0724180431797947 ) ) ;
#48085 = CARTESIAN_POINT ( 'NONE',  ( 37.19810310196314163, -279.4396171916161506, -261.6093133841915233 ) ) ;
#48086 = DIRECTION ( 'NONE',  ( -0.000000000000000000, -0.000000000000000000, 1.000000000000000000 ) ) ;
#48087 = CARTESIAN_POINT ( 'NONE',  ( 24.77387833664412753, -273.4393883548008830, -226.0176265517116008 ) ) ;
#48088 = CARTESIAN_POINT ( 'NONE',  ( -39.16861357176617275, -276.4242668820821223, -343.4402193438015161 ) ) ;
#48089 = CARTESIAN_POINT ( 'NONE',  ( -12.75888253767304725, -296.2469795172567615, -339.8871329579883991 ) ) ;
#48090 = CARTESIAN_POINT ( 'NONE',  ( 35.04052959382801191, -280.1497475699191000, -244.8586807805911576 ) ) ;
#48091 = CARTESIAN_POINT ( 'NONE',  ( -10.39230126272301824, -295.6328916789736923, -338.4576549657351734 ) ) ;
#48092 = CARTESIAN_POINT ( 'NONE',  ( -36.26448459679993164, -296.3541164526544094, -346.8734047659946214 ) ) ;
#48093 = CARTESIAN_POINT ( 'NONE',  ( -68.04558847840438318, -297.4707818022457673, -204.1185230702592719 ) ) ;
#48094 = CARTESIAN_POINT ( 'NONE',  ( -107.5927280713699190, -292.8950539665082715, -243.9496914794908946 ) ) ;
#48095 = CARTESIAN_POINT ( 'NONE',  ( -43.66838422059648650, -286.1411151666180217, -193.5682139787643052 ) ) ;
#48096 = CARTESIAN_POINT ( 'NONE',  ( 33.57407779989951280, -273.3488435027134074, -243.6916987981893783 ) ) ;
#48097 = CARTESIAN_POINT ( 'NONE',  ( 34.04153349200878864, -287.7535908976397536, -299.3723852078082928 ) ) ;
#48098 = CARTESIAN_POINT ( 'NONE',  ( -69.24873593890242773, -281.6101677387080713, -202.8793584270936492 ) ) ;
#48099 = EDGE_CURVE ( 'NONE', #71727, #3540, #80024, .T. ) ;
#48100 = CARTESIAN_POINT ( 'NONE',  ( 10.25913087916912758, -287.4355165199410749, -326.0839733444259991 ) ) ;
#48101 = AXIS2_PLACEMENT_3D ( 'NONE', #69883, #70829, #91645 ) ;
#48102 = CARTESIAN_POINT ( 'NONE',  ( -76.11297254768760467, -289.5343665862042144, -206.1000723414180982 ) ) ;
#48103 = CARTESIAN_POINT ( 'NONE',  ( 206.7397234113112461, 289.2571863808457238, -82.84736978277094011 ) ) ;
#48104 = CARTESIAN_POINT ( 'NONE',  ( 4.765946453601778821, -286.1453991372242740, -210.5921317269410622 ) ) ;
#48105 = CARTESIAN_POINT ( 'NONE',  ( 208.4306832106271656, 1.063508326895939327, -7.500000000000014211 ) ) ;
#48106 = CARTESIAN_POINT ( 'NONE',  ( -5.542016770250216773, -283.5852327370769217, -340.2295683170670486 ) ) ;
#48107 = CARTESIAN_POINT ( 'NONE',  ( -109.2492104208645429, -289.9535196269534367, -243.3372180496246813 ) ) ;
#48108 = CARTESIAN_POINT ( 'NONE',  ( -28.33994573032229880, -281.7645389719714899, -194.6416201430762385 ) ) ;
#48109 = CARTESIAN_POINT ( 'NONE',  ( 5.891699245674284491, -281.9402779481541188, -207.2408244923067855 ) ) ;
#48110 = CARTESIAN_POINT ( 'NONE',  ( 17.96591689903805289, -280.7067189414089512, -222.6967033849904851 ) ) ;
#48111 = CARTESIAN_POINT ( 'NONE',  ( -0.7690224333663998602, -276.5380006619288338, -204.8678694244426595 ) ) ;
#48112 = CARTESIAN_POINT ( 'NONE',  ( -97.40743715241715961, -295.9064197607296478, -318.5598558583279214 ) ) ;
#48113 = CARTESIAN_POINT ( 'NONE',  ( -102.5485085179513334, -289.0593478732129711, -233.9243277277530240 ) ) ;
#48114 = CARTESIAN_POINT ( 'NONE',  ( -98.16367373487452141, -271.9161161942348031, -229.1874115693156568 ) ) ;
#48115 = VERTEX_POINT ( 'NONE', #3016 ) ;
#48116 = ORIENTED_EDGE ( 'NONE', *, *, #18207, .T. ) ;
#48117 = CARTESIAN_POINT ( 'NONE',  ( -100.8503879849079397, -286.9981649625802902, -231.4303869142295582 ) ) ;
#48118 = CARTESIAN_POINT ( 'NONE',  ( 37.48537491343476091, -294.8435770192777454, -287.2252398383371315 ) ) ;
#48119 = CARTESIAN_POINT ( 'NONE',  ( 18.57768135893347150, -282.8716615639164615, -317.4646838326616489 ) ) ;
#48120 = CARTESIAN_POINT ( 'NONE',  ( 0.9193240794713762876, -275.6137808110120204, -336.9714951117172177 ) ) ;
#48121 = CARTESIAN_POINT ( 'NONE',  ( -114.1490865168415496, -291.1568109996039766, -274.0945055092949474 ) ) ;
#48122 = CARTESIAN_POINT ( 'NONE',  ( -60.11569579609300007, -283.8997746002893905, -198.0454504107334230 ) ) ;
#48123 = CARTESIAN_POINT ( 'NONE',  ( -69.61816762772461686, -291.9720920344217916, -200.4613457950580937 ) ) ;
#48124 = CARTESIAN_POINT ( 'NONE',  ( 33.40799360663910988, -287.6463735253017830, -252.2394594944182415 ) ) ;
#48125 = CARTESIAN_POINT ( 'NONE',  ( 209.9972545312790544, 27.55378999303204068, 9.000000000000001776 ) ) ;
#48126 = CARTESIAN_POINT ( 'NONE',  ( 152.7546676148616029, 130.4533703983872783, -11.50000000000000178 ) ) ;
#48127 = CARTESIAN_POINT ( 'NONE',  ( 201.2023760237154022, 289.8772717810621771, -82.34854583857284638 ) ) ;
#48128 = CARTESIAN_POINT ( 'NONE',  ( -31.66834704498080910, -284.5019116313486052, -346.4697382252610964 ) ) ;
#48129 = CARTESIAN_POINT ( 'NONE',  ( -37.37352853689063181, -280.5523547857346784, -345.3611179825600175 ) ) ;
#48130 = EDGE_LOOP ( 'NONE', ( #24468, #44443, #13034, #52818 ) ) ;
#48131 = CARTESIAN_POINT ( 'NONE',  ( 34.37044507695362228, -280.2718136640810940, -255.0830286507073197 ) ) ;
#48132 = CARTESIAN_POINT ( 'NONE',  ( 38.71419002419975186, -275.3717312788068625, -282.5802417195464500 ) ) ;
#48133 = CARTESIAN_POINT ( 'NONE',  ( -65.52973139678472592, -281.6828876221191535, -201.0396687706584942 ) ) ;
#48134 = CARTESIAN_POINT ( 'NONE',  ( 86.48509054211875480, 81.40261763058097699, -300.6191915867298121 ) ) ;
#48135 = CARTESIAN_POINT ( 'NONE',  ( -2.641384495198680238, -279.0766083356290892, -202.2693806509963395 ) ) ;
#48136 = CARTESIAN_POINT ( 'NONE',  ( -80.23426965169983305, -283.4886673868447247, -209.2069716719045687 ) ) ;
#48137 = CARTESIAN_POINT ( 'NONE',  ( -112.3254095316165575, -274.5550457451084299, -259.1513055606759508 ) ) ;
#48138 = PRODUCT_DEFINITION_SHAPE ( 'NONE', 'NONE',  #45828 ) ;
#48139 = CARTESIAN_POINT ( 'NONE',  ( 34.77367263360802241, -293.8889931390622792, -258.5627964123414699 ) ) ;
#48140 = EDGE_LOOP ( 'NONE', ( #71186, #91570, #27393 ) ) ;
#48141 = CARTESIAN_POINT ( 'NONE',  ( -69.21643514041636536, -290.3086991821817833, -204.1260422614612651 ) ) ;
#48142 = CARTESIAN_POINT ( 'NONE',  ( 16.88923124050585400, -276.9560013031302788, -324.9544579712895711 ) ) ;
#48143 = CARTESIAN_POINT ( 'NONE',  ( -35.39032682862060142, -274.0772884858102429, -197.3746985426482752 ) ) ;
#48144 = CARTESIAN_POINT ( 'NONE',  ( -108.8732912634602314, -271.8258429508988456, -242.5613660887286187 ) ) ;
#48145 = DIRECTION ( 'NONE',  ( 0.000000000000000000, -1.000000000000000000, 0.000000000000000000 ) ) ;
#48146 = CARTESIAN_POINT ( 'NONE',  ( 31.39124254195288444, -273.1576487003497959, -240.2202605137360081 ) ) ;
#48147 = CARTESIAN_POINT ( 'NONE',  ( -43.53450532834227715, -248.8283547351244067, -480.0763058130885383 ) ) ;
#48148 = CARTESIAN_POINT ( 'NONE',  ( 35.33738724059130476, -282.5008974009485883, -260.3938012047546522 ) ) ;
#48149 = CARTESIAN_POINT ( 'NONE',  ( 20.84865420022137883, -283.9789812043584902, -319.2268184223113963 ) ) ;
#48150 = CARTESIAN_POINT ( 'NONE',  ( -110.4210618144994811, -283.8576144872841951, -273.6344385098506109 ) ) ;
#48151 = CARTESIAN_POINT ( 'NONE',  ( -27.15986309337434790, -272.5834449228148628, -197.2154022288762008 ) ) ;
#48152 = CARTESIAN_POINT ( 'NONE',  ( -2.591510683314547148, -282.3771793671254500, -204.7472373271185404 ) ) ;
#48153 = CARTESIAN_POINT ( 'NONE',  ( 36.07072427727253228, -273.9407200308869506, -263.3740828805771343 ) ) ;
#48154 = CARTESIAN_POINT ( 'NONE',  ( 208.4306832106270804, -148.7221692137691491, 7.500000000000012434 ) ) ;
#48155 = CARTESIAN_POINT ( 'NONE',  ( 30.45546947606247556, -276.2580272155894363, -242.3393587185985041 ) ) ;
#48156 = DIRECTION ( 'NONE',  ( -0.6023974895724014678, -0.000000000000000000, 0.7981962569173501887 ) ) ;
#48157 = CARTESIAN_POINT ( 'NONE',  ( -35.35048106932609358, -280.8793458563240506, -193.5352891781130609 ) ) ;
#48158 = EDGE_CURVE ( 'NONE', #41591, #4350, #69405, .T. ) ;
#48159 = EDGE_LOOP ( 'NONE', ( #60231, #58105, #8414, #18953 ) ) ;
#48160 = DIRECTION ( 'NONE',  ( -0.000000000000000000, 1.000000000000000000, -0.000000000000000000 ) ) ;
#48161 = CARTESIAN_POINT ( 'NONE',  ( -89.06065693698418784, -287.1950952844992457, -214.9231892402815731 ) ) ;
#48162 = CARTESIAN_POINT ( 'NONE',  ( -90.53164746971077648, -295.0266919885551715, -320.6678543587751733 ) ) ;
#48163 = EDGE_CURVE ( 'NONE', #48925, #78455, #40646, .T. ) ;
#48164 = CARTESIAN_POINT ( 'NONE',  ( -112.1654381582483069, -289.6778751024993426, -288.1578626059623502 ) ) ;
#48165 = CARTESIAN_POINT ( 'NONE',  ( 24.39149250408241087, -285.2322303745413024, -229.4395364344854329 ) ) ;
#48167 = CARTESIAN_POINT ( 'NONE',  ( -91.48540141591061570, -289.5078895091708091, -219.8801859189374852 ) ) ;
#48166 = CARTESIAN_POINT ( 'NONE',  ( 29.35156276043435497, -285.7102677632536256, -239.2583270995723410 ) ) ;
#48168 = TOROIDAL_SURFACE ( 'NONE', #22501, 24.00000000000000355, 1.000000000000000000 ) ;
#48169 = CARTESIAN_POINT ( 'NONE',  ( -94.58510355949549364, -285.1113264748915412, -316.3193605643512569 ) ) ;
#48170 = CARTESIAN_POINT ( 'NONE',  ( -26.09567069839383180, -274.9087881577153780, -344.5131743840228182 ) ) ;
#48171 = CARTESIAN_POINT ( 'NONE',  ( 24.90351194010699132, -285.3640387415452437, -226.3843873973165444 ) ) ;
#48172 = CARTESIAN_POINT ( 'NONE',  ( -103.5016762719473462, -299.0222371892259616, -234.9258414638996726 ) ) ;
#48173 = CARTESIAN_POINT ( 'NONE',  ( 4.188483759107254123, -284.6098817907607668, -207.6471174207159152 ) ) ;
#48174 = CARTESIAN_POINT ( 'NONE',  ( -3.049495471550309311, -281.4581639829564210, -205.6363620462592792 ) ) ;
#48175 = CARTESIAN_POINT ( 'NONE',  ( -3.854061793760648946, -290.6116789360389134, -337.6703220621185437 ) ) ;
#48176 = CARTESIAN_POINT ( 'NONE',  ( 193.1193385863660978, 276.0000000000001137, 16.90038786543260940 ) ) ;
#48177 = DIRECTION ( 'NONE',  ( -0.000000000000000000, -1.000000000000000000, -0.000000000000000000 ) ) ;
#48178 = CARTESIAN_POINT ( 'NONE',  ( -65.05220623504222033, -297.3315034624819191, -340.6704632836123778 ) ) ;
#48179 = CARTESIAN_POINT ( 'NONE',  ( -103.9198863114396119, -277.0104159929051093, -235.7178019441233516 ) ) ;
#48180 = CARTESIAN_POINT ( 'NONE',  ( 19.30354945160366142, -292.0415279096809513, -218.4431584635558465 ) ) ;
#48181 = CARTESIAN_POINT ( 'NONE',  ( -95.41545011542045529, -294.3168545863970849, -315.9009904023843092 ) ) ;
#48182 = CARTESIAN_POINT ( 'NONE',  ( 18.86073536142054508, -280.9053923955477785, -317.7360035651342969 ) ) ;
#48183 = CARTESIAN_POINT ( 'NONE',  ( -59.88897828414093993, -271.8377124552929445, -199.3639816523339903 ) ) ;
#48184 = CARTESIAN_POINT ( 'NONE',  ( 28.84592326470875889, -295.2981185180726698, -302.4228937726682602 ) ) ;
#48185 = CARTESIAN_POINT ( 'NONE',  ( 21.27581636871892101, -295.4090924074130839, -223.5744983911110353 ) ) ;
#48186 = CARTESIAN_POINT ( 'NONE',  ( -111.9315635258766548, -294.8289132191052886, -286.4564599686050883 ) ) ;
#48187 = CARTESIAN_POINT ( 'NONE',  ( 32.47651884501699016, -292.1806182556719591, -300.4837451469400662 ) ) ;
#48188 = CARTESIAN_POINT ( 'NONE',  ( -89.06240403470538070, -291.2223359890217012, -322.7094102557475708 ) ) ;
#48189 = DIRECTION ( 'NONE',  ( -1.000000000000000000, 0.000000000000000000, 0.000000000000000000 ) ) ;
#48190 = CARTESIAN_POINT ( 'NONE',  ( -28.09605347149809518, -292.9752033197778474, -197.7353328131947876 ) ) ;
#48191 = FACE_OUTER_BOUND ( 'NONE', #65993, .T. ) ;
#48192 = CARTESIAN_POINT ( 'NONE',  ( -109.4863796075772910, -291.4287114631408144, -296.2700622463460718 ) ) ;
#48194 = CARTESIAN_POINT ( 'NONE',  ( -28.10634817360825011, -292.1725000703404476, -197.8969160183965528 ) ) ;
#48193 = CARTESIAN_POINT ( 'NONE',  ( 12.57203154460730765, -280.3810623515549878, -326.8843052278369896 ) ) ;
#48195 = CARTESIAN_POINT ( 'NONE',  ( -6.230367260804436036, -280.4497173260231762, -199.9118759752091705 ) ) ;
#48196 = CARTESIAN_POINT ( 'NONE',  ( -104.4006824616695042, -283.7270248147945608, -308.2690538005964527 ) ) ;
#48197 = CARTESIAN_POINT ( 'NONE',  ( 24.24457226759903605, -286.1298346627839351, -312.8943929153469412 ) ) ;
#48198 = CARTESIAN_POINT ( 'NONE',  ( -45.80340010422668229, -281.2999921081806747, -344.1643498713454505 ) ) ;
#48199 = LINE ( 'NONE', #56272, #57865 ) ;
#48200 = CARTESIAN_POINT ( 'NONE',  ( -70.91197008725632145, -278.0971406944752857, -201.8356137489730031 ) ) ;
#48201 = CARTESIAN_POINT ( 'NONE',  ( -35.14326549877506523, -284.9994502276404660, -193.6886549248184224 ) ) ;
#48202 = CARTESIAN_POINT ( 'NONE',  ( 31.33745725645997737, -295.5112275111496842, -297.5124002757800667 ) ) ;
#48203 = CARTESIAN_POINT ( 'NONE',  ( 18.48520459717543574, -277.6944423838507419, -322.5335532492172774 ) ) ;
#48204 = CARTESIAN_POINT ( 'NONE',  ( -29.71543538952376906, -276.6197943412473137, -343.0338504192867504 ) ) ;
#48205 = CARTESIAN_POINT ( 'NONE',  ( -113.1723885649860790, -290.8860182774737950, -256.9929956124397563 ) ) ;
#48206 = CARTESIAN_POINT ( 'NONE',  ( 18.69876228800809415, -280.3340898087510595, -321.1207778022061348 ) ) ;
#48207 = CARTESIAN_POINT ( 'NONE',  ( 35.94337457124368740, -292.6163125183845750, -270.7731708454860495 ) ) ;
#48208 = CARTESIAN_POINT ( 'NONE',  ( -109.3037970399574021, -294.2793639761447935, -291.5360056562745967 ) ) ;
#48209 = ORIENTED_EDGE ( 'NONE', *, *, #26879, .F. ) ;
#48210 = DIRECTION ( 'NONE',  ( 0.6056179655966483777, -0.7957555401921979632, 0.000000000000000000 ) ) ;
#48211 = CARTESIAN_POINT ( 'NONE',  ( -28.89508416255553769, -294.4499753546238594, -342.9838155983697447 ) ) ;
#48212 = DIRECTION ( 'NONE',  ( 1.000000000000000000, 0.000000000000000000, 0.000000000000000000 ) ) ;
#48213 = CARTESIAN_POINT ( 'NONE',  ( -109.1418805571601069, -282.0523547857346784, -270.3284710469131937 ) ) ;
#48214 = CARTESIAN_POINT ( 'NONE',  ( -91.46112644410375481, -296.3630665602345857, -215.9193334063130862 ) ) ;
#48215 = CARTESIAN_POINT ( 'NONE',  ( 38.38447587388164806, -279.7224820264187883, -272.7801562233553341 ) ) ;
#48216 = ADVANCED_FACE ( 'NONE', ( #84410 ), #62192, .F. ) ;
#48217 = EDGE_CURVE ( 'NONE', #66186, #62642, #48904, .T. ) ;
#48218 = CARTESIAN_POINT ( 'NONE',  ( -64.38862046288612362, -287.0216211162978652, -198.7805505694091153 ) ) ;
#48219 = CARTESIAN_POINT ( 'NONE',  ( 21.99282024748162456, -286.7900700911326908, -227.7504317409685370 ) ) ;
#48220 = CARTESIAN_POINT ( 'NONE',  ( -59.38411559195876777, -278.8629099092265164, -340.6806719609382412 ) ) ;
#48221 = CARTESIAN_POINT ( 'NONE',  ( -106.4949680734156487, -294.2041406121150544, -298.4622270833087896 ) ) ;
#48222 = CARTESIAN_POINT ( 'NONE',  ( -80.73096090367614863, -297.4101122009274718, -330.3223226113856867 ) ) ;
#48223 = CARTESIAN_POINT ( 'NONE',  ( -107.5007011856816774, -277.0610164495790855, -292.0916920042543552 ) ) ;
#48224 = VERTEX_POINT ( 'NONE', #83470 ) ;
#48225 = LINE ( 'NONE', #77127, #37947 ) ;
#48226 = CARTESIAN_POINT ( 'NONE',  ( -103.8293999450873883, -296.7250128119463852, -231.4600736546301789 ) ) ;
#48227 = CARTESIAN_POINT ( 'NONE',  ( -111.4080644413768795, -292.5686752247817708, -262.9120996640185695 ) ) ;
#48228 = CARTESIAN_POINT ( 'NONE',  ( 37.82059482285082197, -295.3116620276945241, -282.9730546295761542 ) ) ;
#48229 = CARTESIAN_POINT ( 'NONE',  ( 201.2258855950020120, 292.9574286262273404, -53.99999999998392042 ) ) ;
#48230 = CARTESIAN_POINT ( 'NONE',  ( -61.28057334557731650, -290.0228310720435161, -339.4322625883503974 ) ) ;
#48231 = CARTESIAN_POINT ( 'NONE',  ( -48.18343439339133027, -258.6462052220223882, -448.1683005986033663 ) ) ;
#48232 = CARTESIAN_POINT ( 'NONE',  ( 39.04270912039385166, -280.7130715193023320, -278.5055142916631894 ) ) ;
#48233 = CARTESIAN_POINT ( 'NONE',  ( -105.8631005652257500, -296.7521921598509493, -305.3801170956911619 ) ) ;
#48234 = CARTESIAN_POINT ( 'NONE',  ( -104.0793199474377673, -288.2204817048622658, -306.2274751834333415 ) ) ;
#48235 = AXIS2_PLACEMENT_3D ( 'NONE', #55562, #4886, #83954 ) ;
#48236 = CARTESIAN_POINT ( 'NONE',  ( 76.34370912324891378, -299.7723574772524557, -193.3759528850984850 ) ) ;
#48237 = CARTESIAN_POINT ( 'NONE',  ( 188.7149167944524493, -12.49482340714361506, 10.00000000000000000 ) ) ;
#48238 = CARTESIAN_POINT ( 'NONE',  ( 165.2494399300530290, -11.64849832608277325, 10.00000000000000000 ) ) ;
#48239 = DIRECTION ( 'NONE',  ( 0.000000000000000000, 0.000000000000000000, 1.000000000000000000 ) ) ;
#48240 = CARTESIAN_POINT ( 'NONE',  ( -2.103535665248870146, -290.1142860229408029, -338.0440517228934709 ) ) ;
#48241 = CARTESIAN_POINT ( 'NONE',  ( 44.71564893372296723, -284.0519495502702512, -270.3284710469131937 ) ) ;
#48242 = ORIENTED_EDGE ( 'NONE', *, *, #82962, .T. ) ;
#48243 = CARTESIAN_POINT ( 'NONE',  ( 37.58007017541937955, -280.6831690714219008, -252.9815412302551181 ) ) ;
#48244 = CARTESIAN_POINT ( 'NONE',  ( -112.1504076022523151, -286.5087614331251302, -273.7458378903837115 ) ) ;
#48245 = CARTESIAN_POINT ( 'NONE',  ( 37.14931278864178665, -285.9117211328272674, -253.2825489496468094 ) ) ;
#48246 = CARTESIAN_POINT ( 'NONE',  ( 34.63013171584941574, -273.2854874025736649, -249.6797832033184648 ) ) ;
#48247 = CARTESIAN_POINT ( 'NONE',  ( -77.35853366648174756, -275.4309988540003360, -207.5919597100882186 ) ) ;
#48248 = CARTESIAN_POINT ( 'NONE',  ( -90.83444329595218392, -289.3656453919955425, -218.5939408731165656 ) ) ;
#48249 = CARTESIAN_POINT ( 'NONE',  ( -108.5673249219375407, -280.0792343271966729, -296.3449803599485222 ) ) ;
#48251 = CARTESIAN_POINT ( 'NONE',  ( -16.88525478471229491, -279.6720178844207112, -200.1797350393848944 ) ) ;
#48250 = CARTESIAN_POINT ( 'NONE',  ( -62.30894776949511282, -279.7182842829084848, -201.7101182751092097 ) ) ;
#48252 = CARTESIAN_POINT ( 'NONE',  ( -31.46019730038518247, -278.0593344818556147, -346.8785573851295680 ) ) ;
#48253 = CARTESIAN_POINT ( 'NONE',  ( 37.59942885551402725, -280.1467957857979059, -254.4289681991214138 ) ) ;
#48254 = CARTESIAN_POINT ( 'NONE',  ( 137.1361844366198284, 179.7607878149970873, -239.0752527614820906 ) ) ;
#48255 = CARTESIAN_POINT ( 'NONE',  ( 17.91188411107352962, -275.7607703711248632, -216.9944729222064552 ) ) ;
#48256 = ITEM_DEFINED_TRANSFORMATION ( 'NONE', 'NONE', #28012,  #18940 ) ;
#48257 = CARTESIAN_POINT ( 'NONE',  ( -113.1758016124685469, -274.1792792852132266, -261.8819196752850189 ) ) ;
#48258 = CARTESIAN_POINT ( 'NONE',  ( -95.95921662488163406, -292.4090924074130839, -317.1477375740089997 ) ) ;
#48259 = ORIENTED_EDGE ( 'NONE', *, *, #20584, .F. ) ;
#48260 = CARTESIAN_POINT ( 'NONE',  ( 156.4947056272798136, 20.99999999999998934, -15.00000000000000711 ) ) ;
#48261 = CARTESIAN_POINT ( 'NONE',  ( 33.68464352486044078, -288.3926430302678341, -252.1587781654427545 ) ) ;
#48262 = CARTESIAN_POINT ( 'NONE',  ( 38.08754324716364437, -289.4340977047092451, -279.9724771504866112 ) ) ;
#48263 = CARTESIAN_POINT ( 'NONE',  ( -71.22736778932592472, -288.8604619849172082, -335.1491306327570214 ) ) ;
#48264 = CARTESIAN_POINT ( 'NONE',  ( -89.83966968000169118, -284.8427110194635361, -214.0437511867768308 ) ) ;
#48265 = CARTESIAN_POINT ( 'NONE',  ( -55.04033302849770593, -170.0623274831404501, -364.4220463826554237 ) ) ;
#48266 = CARTESIAN_POINT ( 'NONE',  ( -33.47446041278221429, -281.4025652945214802, -344.0724367632854523 ) ) ;
#48267 = CARTESIAN_POINT ( 'NONE',  ( 0.7830223900123518543, -288.4264218532675841, -206.6037034371304628 ) ) ;
#48268 = CARTESIAN_POINT ( 'NONE',  ( 5.984242604995782422, -280.9322072682146541, -329.9729493334255039 ) ) ;
#48269 = CARTESIAN_POINT ( 'NONE',  ( -46.53463803143360167, -281.2483632428370015, -197.3937359102122855 ) ) ;
#48270 = CARTESIAN_POINT ( 'NONE',  ( -59.20744856401751832, -277.8353006702819243, -340.0739395211526244 ) ) ;
#48271 = CARTESIAN_POINT ( 'NONE',  ( -87.13802472664364984, -288.5225688464320797, -328.6402068824518210 ) ) ;
#48272 = CARTESIAN_POINT ( 'NONE',  ( -111.5679106737709674, -285.6065000147708588, -250.2957787312075197 ) ) ;
#48273 = CARTESIAN_POINT ( 'NONE',  ( -97.12061319322400266, -284.3941279144026453, -318.8174311157850411 ) ) ;
#48274 = CARTESIAN_POINT ( 'NONE',  ( 35.56602825606886853, -281.7672363353926244, -274.0303340226344631 ) ) ;
#48275 = ORIENTED_EDGE ( 'NONE', *, *, #67622, .T. ) ;
#48276 = CARTESIAN_POINT ( 'NONE',  ( 207.1626556784407001, 29.88353989719039916, 14.95883904121434860 ) ) ;
#48277 = CARTESIAN_POINT ( 'NONE',  ( -98.85336085966375208, -291.8164170333934635, -314.6170461761369097 ) ) ;
#48278 = CARTESIAN_POINT ( 'NONE',  ( -2.266904459064136734, -291.1912931058530489, -202.3533679012895732 ) ) ;
#48279 = CARTESIAN_POINT ( 'NONE',  ( 15.62522702115081152, -273.8830356304416114, -219.7118805459503221 ) ) ;
#48280 = CARTESIAN_POINT ( 'NONE',  ( -68.19290821783590673, -294.7954055040969479, -340.7991456826188141 ) ) ;
#48281 = CARTESIAN_POINT ( 'NONE',  ( -57.82930486894797184, -290.2627198948393357, -199.5195675322050874 ) ) ;
#48282 = CARTESIAN_POINT ( 'NONE',  ( -87.18875795470485457, -293.9981015954780332, -325.0716730659176505 ) ) ;
#48283 = CARTESIAN_POINT ( 'NONE',  ( -106.4010151430424429, -291.4279441581856531, -295.2195474187745390 ) ) ;
#48284 = CARTESIAN_POINT ( 'NONE',  ( 200.9306832106270804, -142.7221692137691775, 0.000000000000000000 ) ) ;
#48285 = CARTESIAN_POINT ( 'NONE',  ( -107.9732148254756510, -292.2236681064712229, -295.7377400441716304 ) ) ;
#48286 = CARTESIAN_POINT ( 'NONE',  ( -36.37571562165233985, -290.0640810556073461, -195.1879316464278702 ) ) ;
#48287 = CARTESIAN_POINT ( 'NONE',  ( 34.13697829171586307, -295.8473533208329513, -293.2405296360474836 ) ) ;
#48288 = CARTESIAN_POINT ( 'NONE',  ( -85.89106717455422313, -286.3015191168598790, -215.4629765413057214 ) ) ;
#48289 = CARTESIAN_POINT ( 'NONE',  ( 7.825334897150399094, -296.4369795928970461, -330.4441219903541196 ) ) ;
#48290 = CARTESIAN_POINT ( 'NONE',  ( 16.88800983094458275, -276.7992430895737357, -217.9646831585044140 ) ) ;
#48291 = EDGE_CURVE ( 'NONE', #34891, #60602, #53602, .T. ) ;
#48292 = CARTESIAN_POINT ( 'NONE',  ( -80.52580401830833523, -296.6804488125075068, -206.7417257793347289 ) ) ;
#48293 = CARTESIAN_POINT ( 'NONE',  ( -18.78421973913642162, -275.0497598008045657, -342.0102207865367632 ) ) ;
#48294 = CARTESIAN_POINT ( 'NONE',  ( -30.09839855958027144, -278.2242163915004767, -196.2230040988926589 ) ) ;
#48295 = CARTESIAN_POINT ( 'NONE',  ( -64.73113572071081023, -274.8914451269762935, -202.2524143782383703 ) ) ;
#48296 = CARTESIAN_POINT ( 'NONE',  ( 21.40953634539815553, -273.4647390110447986, -221.5052226612841935 ) ) ;
#48297 = CARTESIAN_POINT ( 'NONE',  ( -47.85945287511258073, -296.6136657269190664, -343.2465373170531961 ) ) ;
#48298 = DIRECTION ( 'NONE',  ( 0.000000000000000000, 0.000000000000000000, -1.000000000000000000 ) ) ;
#48299 = CARTESIAN_POINT ( 'NONE',  ( -110.2592475881748726, -297.2686014344033651, -276.9242794681202895 ) ) ;
#48300 = AXIS2_PLACEMENT_3D ( 'NONE', #34838, #92114, #56155 ) ;
#48301 = CARTESIAN_POINT ( 'NONE',  ( -54.94434090351493438, -212.1443419142231051, 22.50000000000000000 ) ) ;
#48303 = CARTESIAN_POINT ( 'NONE',  ( -76.56243908317212288, -273.3445010671472915, -208.7921839304540583 ) ) ;
#48302 = CARTESIAN_POINT ( 'NONE',  ( -34.74920894124682036, -287.0398363969529782, -345.6717134848606179 ) ) ;
#48304 = CARTESIAN_POINT ( 'NONE',  ( -12.70370912436400346, -286.3638245121680370, -197.4092886751276410 ) ) ;
#48305 = AXIS2_PLACEMENT_3D ( 'NONE', #81607, #37140, #24318 ) ;
#48306 = CARTESIAN_POINT ( 'NONE',  ( -3.073958341812169426, -288.2786149031339846, -339.3066218145507946 ) ) ;
#48307 = CARTESIAN_POINT ( 'NONE',  ( -110.3682943135602414, -298.2937635201168405, -289.0013984510330829 ) ) ;
#48308 = CARTESIAN_POINT ( 'NONE',  ( 27.36546434194725919, -292.0550941575467050, -307.9511604220298295 ) ) ;
#48309 = CARTESIAN_POINT ( 'NONE',  ( 26.58186677002952791, -281.3117356188814142, -312.9983835544960016 ) ) ;
#48310 = CARTESIAN_POINT ( 'NONE',  ( -69.91165696735023971, -292.9809262143061801, -337.9199732462171255 ) ) ;
#48311 = CARTESIAN_POINT ( 'NONE',  ( -40.23143059711612324, -278.0158033824083077, -195.3666499803061640 ) ) ;
#48312 = CARTESIAN_POINT ( 'NONE',  ( 197.4027394742815602, 40.84896208771628068, 12.00000000000000000 ) ) ;
#48313 = CARTESIAN_POINT ( 'NONE',  ( -13.17151362372341161, -287.5259493857911934, -339.6643111905694923 ) ) ;
#48314 = CARTESIAN_POINT ( 'NONE',  ( 145.2857639756989272, -299.5541904835127980, -195.3611179825600175 ) ) ;
#48315 = CARTESIAN_POINT ( 'NONE',  ( -104.6512700280956096, -288.1156943258516776, -303.4431742292746321 ) ) ;
#48316 = CARTESIAN_POINT ( 'NONE',  ( -109.8151229117183050, -274.2503445683700534, -256.7344692846174894 ) ) ;
#48317 = CARTESIAN_POINT ( 'NONE',  ( -30.25136146452663510, -284.3893788874253801, -346.4422154389332604 ) ) ;
#48319 = CARTESIAN_POINT ( 'NONE',  ( 32.73458966462342801, -281.2815865231557950, -249.9084015642242775 ) ) ;
#48318 = CARTESIAN_POINT ( 'NONE',  ( -40.34881800459285728, -296.0347712644656895, -195.0149243524149085 ) ) ;
#48320 = CARTESIAN_POINT ( 'NONE',  ( -112.2748472428251034, -296.9404662471065421, -252.6404106598941155 ) ) ;
#48321 = CARTESIAN_POINT ( 'NONE',  ( -35.39276809505724231, -275.5023302713062776, -196.7850927431614707 ) ) ;
#48322 = CARTESIAN_POINT ( 'NONE',  ( 37.64001326412503801, -283.5106729013216409, -267.1177837441419456 ) ) ;
#48323 = CARTESIAN_POINT ( 'NONE',  ( -93.14015919119425746, -272.1461418700350237, -222.7943157374531324 ) ) ;
#48324 = VERTEX_POINT ( 'NONE', #54140 ) ;
#48325 = DIRECTION ( 'NONE',  ( 1.000000000000000000, 0.000000000000000000, 0.000000000000000000 ) ) ;
#48326 = CARTESIAN_POINT ( 'NONE',  ( -73.18549626151961718, -287.5544330567582278, -204.8708652353481909 ) ) ;
#48327 = CARTESIAN_POINT ( 'NONE',  ( 143.6449502718966755, 0.000000000000000000, 21.50000000000000000 ) ) ;
#48328 = CARTESIAN_POINT ( 'NONE',  ( -2.602324593224659921, -277.9809262143061233, -198.2974183793908196 ) ) ;
#48329 = CARTESIAN_POINT ( 'NONE',  ( -113.5555853299319296, -277.8769297596418255, -260.1791036389054739 ) ) ;
#48330 = EDGE_CURVE ( 'NONE', #42209, #10045, #61277, .T. ) ;
#48331 = CARTESIAN_POINT ( 'NONE',  ( -108.0636303958906552, -288.5882183118450257, -298.7309786267562117 ) ) ;
#48332 = CARTESIAN_POINT ( 'NONE',  ( -40.24245257090158390, -284.6093989717445538, -343.9973413310283945 ) ) ;
#48333 = CARTESIAN_POINT ( 'NONE',  ( 18.93149402914985302, -277.8237901899742042, -318.1080344928448653 ) ) ;
#48334 = CARTESIAN_POINT ( 'NONE',  ( -102.4067645159229443, -285.4497173072661553, -310.4253624932176763 ) ) ;
#48335 = CARTESIAN_POINT ( 'NONE',  ( -92.86953636848627980, -282.6667304108290750, -318.3780606137623295 ) ) ;
#48336 = CARTESIAN_POINT ( 'NONE',  ( 28.19444638708343120, -283.0669582107580027, -233.8917589790296745 ) ) ;
#48337 = CARTESIAN_POINT ( 'NONE',  ( -2.559442880076310711, -274.6660035731552512, -201.6500210935546136 ) ) ;
#48338 = CARTESIAN_POINT ( 'NONE',  ( -103.6068740789867348, -277.8734136366252869, -309.6820917713292829 ) ) ;
#48339 = CARTESIAN_POINT ( 'NONE',  ( -61.45698932821379401, -297.2878551452225793, -340.8413559345464705 ) ) ;
#48340 = DIRECTION ( 'NONE',  ( 0.000000000000000000, 0.000000000000000000, -1.000000000000000000 ) ) ;
#48341 = DIRECTION ( 'NONE',  ( 0.000000000000000000, 1.000000000000000000, 0.000000000000000000 ) ) ;
#48342 = CARTESIAN_POINT ( 'NONE',  ( -85.62663953305602149, -293.8517246473459750, -328.7466479061922087 ) ) ;
#48343 = CARTESIAN_POINT ( 'NONE',  ( 33.95193598306571658, -275.2711147623555235, -286.3931504640509615 ) ) ;
#48344 = CARTESIAN_POINT ( 'NONE',  ( -29.11472206127396589, -299.2325517387172908, -193.6687589893388974 ) ) ;
#48345 = CARTESIAN_POINT ( 'NONE',  ( -37.30253330699734704, -287.8127541948342696, -196.3351800257841830 ) ) ;
#48346 = CARTESIAN_POINT ( 'NONE',  ( 19.03066992430094473, -295.7784688558535322, -321.8663426198303341 ) ) ;
#48347 = CARTESIAN_POINT ( 'NONE',  ( 36.69483933173619761, -294.5092082844912511, -250.6484148318101006 ) ) ;
#48348 = CARTESIAN_POINT ( 'NONE',  ( -93.05468292082453274, -293.2499372506653685, -220.3810392619222682 ) ) ;
#48349 = CARTESIAN_POINT ( 'NONE',  ( -57.58528846773011622, -277.7900246710119632, -198.3178979343840922 ) ) ;
#48350 = CARTESIAN_POINT ( 'NONE',  ( -60.19858852931782423, -281.6738427201626678, -199.4627235524875744 ) ) ;
#48351 = CARTESIAN_POINT ( 'NONE',  ( -61.50323121599836185, -293.4481658126289290, -340.8255182577509004 ) ) ;
#48352 = CARTESIAN_POINT ( 'NONE',  ( -92.51552991585175789, -285.6920635472461640, -322.3046338264631459 ) ) ;
#48353 = CARTESIAN_POINT ( 'NONE',  ( -110.3006262632761008, -283.5730573429611354, -262.7041560976790606 ) ) ;
#48354 = CARTESIAN_POINT ( 'NONE',  ( -69.03337401324819211, -197.1869525245530497, -359.5623982929876092 ) ) ;
#48355 = ORIENTED_EDGE ( 'NONE', *, *, #77442, .T. ) ;
#48356 = CARTESIAN_POINT ( 'NONE',  ( -83.65800552672159540, -285.0631796683132393, -213.8429002867146949 ) ) ;
#48357 = VERTEX_POINT ( 'NONE', #70705 ) ;
#48358 = CARTESIAN_POINT ( 'NONE',  ( 37.84522866867033741, -282.8215958024190400, -285.4746301119304235 ) ) ;
#48359 = CARTESIAN_POINT ( 'NONE',  ( -40.78018372585002993, -274.3411336451096645, -197.3712610901739595 ) ) ;
#48360 = CARTESIAN_POINT ( 'NONE',  ( -10.12063317540506624, -285.1945294551290999, -198.7013773986871001 ) ) ;
#48361 = CARTESIAN_POINT ( 'NONE',  ( 38.56022927156001145, -282.3451071180677445, -258.5398940096742422 ) ) ;
#48362 = CARTESIAN_POINT ( 'NONE',  ( -88.73077615254480577, -279.2783275606940379, -326.7691902467350360 ) ) ;
#48363 = CARTESIAN_POINT ( 'NONE',  ( -50.92977659393751821, -280.5342955611226330, -194.6730940669284848 ) ) ;
#48364 = TOROIDAL_SURFACE ( 'NONE', #90651, 203.9779373800640485, 1.000000000000000000 ) ;
#48365 = CARTESIAN_POINT ( 'NONE',  ( 17.40634833298269157, -272.4094976428775681, -226.7417163044926838 ) ) ;
#48366 = CARTESIAN_POINT ( 'NONE',  ( -112.8250949930600342, -274.3352372842284694, -284.1850902867908530 ) ) ;
#48367 = EDGE_LOOP ( 'NONE', ( #33227, #45407, #14886, #45118 ) ) ;
#48368 = CARTESIAN_POINT ( 'NONE',  ( -32.59967766544144041, -276.1122001132225705, -195.6653361609325827 ) ) ;
#48369 = CARTESIAN_POINT ( 'NONE',  ( 24.68374711691411250, -22.60613715962459835, -344.8050946662477259 ) ) ;
#48370 = CIRCLE ( 'NONE', #72595, 1.000000000000000888 ) ;
#48371 = CARTESIAN_POINT ( 'NONE',  ( -13.76600370310567989, -278.3795911341124452, -199.4825077167134282 ) ) ;
#48372 = CARTESIAN_POINT ( 'NONE',  ( -25.20566085914393639, -293.9649894280912008, -195.3498484120852083 ) ) ;
#48373 = CARTESIAN_POINT ( 'NONE',  ( -63.61336347081373077, -294.7523016461514089, -338.6327307080335913 ) ) ;
#48374 = CARTESIAN_POINT ( 'NONE',  ( -86.46891560568977297, -290.8988238997511644, -211.0800931791311541 ) ) ;
#48375 = FACE_OUTER_BOUND ( 'NONE', #527, .T. ) ;
#48377 = CARTESIAN_POINT ( 'NONE',  ( 23.39685592856236696, -286.5298021907969428, -312.3031679155489542 ) ) ;
#48376 = CARTESIAN_POINT ( 'NONE',  ( -102.6216885265388470, -294.6043399248806622, -310.0742065885632996 ) ) ;
#48378 = CARTESIAN_POINT ( 'NONE',  ( 36.52187393452328479, -295.3099115456131472, -262.4470789572811782 ) ) ;
#48379 = CARTESIAN_POINT ( 'NONE',  ( -103.9393927611244379, -286.2856263280274334, -239.1600271303572640 ) ) ;
#48380 = CARTESIAN_POINT ( 'NONE',  ( -39.21799212274207491, -292.9704245363171253, -193.6063496476391208 ) ) ;
#48381 = CARTESIAN_POINT ( 'NONE',  ( -21.36865974107884014, -283.3342165910232211, -341.7072876758564917 ) ) ;
#48382 = CARTESIAN_POINT ( 'NONE',  ( -76.89044581166889714, -294.3639536327408450, -336.0269928067512524 ) ) ;
#48383 = CARTESIAN_POINT ( 'NONE',  ( -93.46783919006307428, -290.6371201916478526, -322.9165015005222017 ) ) ;
#48384 = CARTESIAN_POINT ( 'NONE',  ( -105.0988082359836682, -290.5728660934659047, -306.8097284351090934 ) ) ;
#48385 = CARTESIAN_POINT ( 'NONE',  ( 34.28456961682574189, -287.9056257663229985, -284.5210461893441902 ) ) ;
#48386 = VERTEX_POINT ( 'NONE', #56021 ) ;
#48387 = DIRECTION ( 'NONE',  ( 0.000000000000000000, 0.000000000000000000, 1.000000000000000000 ) ) ;
#48388 = CARTESIAN_POINT ( 'NONE',  ( -106.6527944323064929, -298.8107939000017268, -239.6326587553027991 ) ) ;
#48389 = CARTESIAN_POINT ( 'NONE',  ( -112.6507146381146924, -295.4067209459291234, -256.8759184266080524 ) ) ;
#48390 = CARTESIAN_POINT ( 'NONE',  ( 17.24617079671854114, -279.9146824177398116, -221.5392704513667468 ) ) ;
#48391 = ORIENTED_EDGE ( 'NONE', *, *, #17135, .T. ) ;
#48392 = CARTESIAN_POINT ( 'NONE',  ( 7.204470190248506434, -274.1485267188602393, -207.5648335849591604 ) ) ;
#48393 = CARTESIAN_POINT ( 'NONE',  ( -111.0674747947812477, -295.0537537471150813, -268.6981155592530399 ) ) ;
#48394 = CARTESIAN_POINT ( 'NONE',  ( -32.31362477967866909, -278.8486366233668150, -344.4766572952412957 ) ) ;
#48395 = CARTESIAN_POINT ( 'NONE',  ( -43.56240282120956664, -272.1124542684461858, -196.3354438154922263 ) ) ;
#48396 = CARTESIAN_POINT ( 'NONE',  ( -105.3239414312393052, -297.3885957285963286, -298.0296085683576166 ) ) ;
#48397 = CARTESIAN_POINT ( 'NONE',  ( -109.0844819342029837, -297.8306052815145222, -255.2275716800408532 ) ) ;
#48398 = DIRECTION ( 'NONE',  ( -1.000000000000000000, 0.000000000000000000, 0.000000000000000000 ) ) ;
#48399 = CARTESIAN_POINT ( 'NONE',  ( -61.32029111936589061, -296.9584460591776178, -342.7451568002657041 ) ) ;
#48400 = CARTESIAN_POINT ( 'NONE',  ( -95.64702959962350803, -271.2274239832901230, -222.6032128009957205 ) ) ;
#48401 = CARTESIAN_POINT ( 'NONE',  ( -12.23297577692504490, -293.0389183995652047, -201.6526366028926134 ) ) ;
#48402 = CARTESIAN_POINT ( 'NONE',  ( -109.2828030577999101, -289.3295433326570105, -254.8739417330797039 ) ) ;
#48403 = CYLINDRICAL_SURFACE ( 'NONE', #15530, 4.025000000000000355 ) ;
#48404 = CARTESIAN_POINT ( 'NONE',  ( 37.84687850303124890, -276.2494818356835253, -286.7384708335228538 ) ) ;
#48405 = CARTESIAN_POINT ( 'NONE',  ( -108.4985990204608015, -297.1016445856391215, -253.9665082921558792 ) ) ;
#48406 = CARTESIAN_POINT ( 'NONE',  ( -39.56455599133202838, -282.0042896937175669, -195.0259346131890652 ) ) ;
#48407 = CARTESIAN_POINT ( 'NONE',  ( 36.51337515722941873, -279.9847435268589493, -250.3432676603068501 ) ) ;
#48408 = CARTESIAN_POINT ( 'NONE',  ( -62.38065179035082508, -276.7179619073056642, -343.1247379986887154 ) ) ;
#48409 = CARTESIAN_POINT ( 'NONE',  ( 21.36750515004459317, -279.2922091855626832, -221.7846871383528651 ) ) ;
#48410 = CARTESIAN_POINT ( 'NONE',  ( 28.29141934333785002, -281.1877589585512851, -302.8008974023246651 ) ) ;
#48411 = CARTESIAN_POINT ( 'NONE',  ( 34.84633991521791074, -279.2823340536546084, -249.3646139553059413 ) ) ;
#48412 = CARTESIAN_POINT ( 'NONE',  ( -24.47571664943014014, -272.7941649313326025, -197.8533217057401714 ) ) ;
#48413 = CARTESIAN_POINT ( 'NONE',  ( -111.5200163286703372, -280.6955736523474911, -259.2036772537322236 ) ) ;
#48414 = CARTESIAN_POINT ( 'NONE',  ( 199.0061125298537377, 275.0000000000000568, -7.725424859374024678 ) ) ;
#48415 = CARTESIAN_POINT ( 'NONE',  ( 169.2744399300530347, -11.64849832608277325, 10.00000000000000000 ) ) ;
#48416 = CARTESIAN_POINT ( 'NONE',  ( -82.35206105707813151, -295.6874400992537062, -209.0745063143155846 ) ) ;
#48417 = CARTESIAN_POINT ( 'NONE',  ( -111.6327960696554129, -290.8062707679650885, -250.0667521518485330 ) ) ;
#48418 = CARTESIAN_POINT ( 'NONE',  ( 37.79750349199251502, -277.5262850201946208, -268.3292462118521939 ) ) ;
#48419 = CYLINDRICAL_SURFACE ( 'NONE', #4517, 24.00000000000001066 ) ;
#48420 = CARTESIAN_POINT ( 'NONE',  ( -108.6269844898742463, -286.7943788840112802, -245.3067285406265512 ) ) ;
#48421 = EDGE_LOOP ( 'NONE', ( #57904, #76580, #91691, #85614 ) ) ;
#48422 = CARTESIAN_POINT ( 'NONE',  ( 207.8645969454241538, 36.34083695896440958, 14.87498546835719360 ) ) ;
#48423 = CARTESIAN_POINT ( 'NONE',  ( 35.14691788232295266, -285.3023664409815865, -250.9209653761595575 ) ) ;
#48424 = CARTESIAN_POINT ( 'NONE',  ( 113.5000000000000568, -298.0521521680024080, -397.9547385950631337 ) ) ;
#48425 = CARTESIAN_POINT ( 'NONE',  ( -2.971326231395900574, -293.3821643461020017, -335.2133184378173496 ) ) ;
#48426 = CARTESIAN_POINT ( 'NONE',  ( 36.68162543543989784, -285.7727716755440497, -276.6084761632639015 ) ) ;
#48427 = CARTESIAN_POINT ( 'NONE',  ( 202.9737475146022803, 296.4636489462809550, -68.70538243550777224 ) ) ;
#48428 = CARTESIAN_POINT ( 'NONE',  ( 26.10596288904169526, -292.0908665098451706, -310.4510551253961808 ) ) ;
#48429 = CARTESIAN_POINT ( 'NONE',  ( -89.39897259387291228, -283.8151017518756589, -214.4972623201564943 ) ) ;
#48430 = CARTESIAN_POINT ( 'NONE',  ( -110.7641900578178706, -280.2559743114786102, -262.4149096979377305 ) ) ;
#48431 = CARTESIAN_POINT ( 'NONE',  ( 0.07636131580060794011, -287.7438180743660041, -203.5038169974123718 ) ) ;
#48432 = CARTESIAN_POINT ( 'NONE',  ( 12.34669393533375370, -278.9729366182945682, -212.8716623681657154 ) ) ;
#48433 = CARTESIAN_POINT ( 'NONE',  ( -10.72409956425161859, -288.6952319305488572, -338.3896182484019164 ) ) ;
#48434 = CARTESIAN_POINT ( 'NONE',  ( -81.65706671060000588, -280.8610423810284260, -211.5474554116948127 ) ) ;
#48435 = CARTESIAN_POINT ( 'NONE',  ( -9.194650087268422922, -281.2326790994700332, -202.8307892314358014 ) ) ;
#48436 = ADVANCED_FACE ( 'NONE', ( #12956 ), #47492, .T. ) ;
#48437 = CARTESIAN_POINT ( 'NONE',  ( -46.33475724499292170, -287.9184698278778001, -195.5444639200435972 ) ) ;
#48438 = CIRCLE ( 'NONE', #45383, 2.046895004029262832 ) ;
#48439 = ORIENTED_EDGE ( 'NONE', *, *, #38852, .T. ) ;
#48440 = CARTESIAN_POINT ( 'NONE',  ( -92.16906346390284455, -273.2947722073475916, -216.2967098230155045 ) ) ;
#48441 = CARTESIAN_POINT ( 'NONE',  ( -101.7098150102609253, -292.0232716020706789, -308.2595933551771736 ) ) ;
#48442 = DIRECTION ( 'NONE',  ( 0.000000000000000000, 0.000000000000000000, -1.000000000000000000 ) ) ;
#48443 = CARTESIAN_POINT ( 'NONE',  ( -99.90806341382572953, -293.6948066931273047, -220.5068182859052968 ) ) ;
#48444 = ORIENTED_EDGE ( 'NONE', *, *, #43976, .F. ) ;
#48445 = CARTESIAN_POINT ( 'NONE',  ( -62.90898176987437296, -271.7198730224327505, -199.6763067759649743 ) ) ;
#48446 = EDGE_CURVE ( 'NONE', #9431, #12419, #70246, .T. ) ;
#48447 = LINE ( 'NONE', #68376, #8035 ) ;
#48448 = CARTESIAN_POINT ( 'NONE',  ( -53.14345620473566356, -293.6512212790958074, -344.9586749577342744 ) ) ;
#48449 = CARTESIAN_POINT ( 'NONE',  ( -36.47620041754861120, -297.5709263286453279, -197.2996537443671343 ) ) ;
#48450 = CARTESIAN_POINT ( 'NONE',  ( -45.41940187598815726, -290.6764806551607876, -343.6104079885153624 ) ) ;
#48451 = CARTESIAN_POINT ( 'NONE',  ( 26.44355838259787461, -283.8220636521855909, -308.0046169842578934 ) ) ;
#48452 = CARTESIAN_POINT ( 'NONE',  ( -38.88990001302435218, -290.4964849865502856, -346.7562053372633954 ) ) ;
#48453 = CARTESIAN_POINT ( 'NONE',  ( -111.4401933423845179, -291.6268495340742106, -289.4584695119689854 ) ) ;
#48454 = CARTESIAN_POINT ( 'NONE',  ( -87.07080284692968064, -287.3602571608963103, -214.1488561749995370 ) ) ;
#48455 = CARTESIAN_POINT ( 'NONE',  ( 3.820177922163388029, -280.7562482401743296, -205.2235664643215785 ) ) ;
#48456 = CARTESIAN_POINT ( 'NONE',  ( -97.14993227689251398, -294.0039261174249532, -316.5378390554113253 ) ) ;
#48457 = CARTESIAN_POINT ( 'NONE',  ( -83.88489227565895590, -283.5045877140880748, -331.7692036055802873 ) ) ;
#48458 = CARTESIAN_POINT ( 'NONE',  ( 36.58621853088934017, -277.5001032749867704, -277.1085857651668789 ) ) ;
#48459 = EDGE_CURVE ( 'NONE', #85436, #51665, #13474, .T. ) ;
#48460 = CARTESIAN_POINT ( 'NONE',  ( 17.36665895637874613, -277.4090924074130839, -226.6919474004047572 ) ) ;
#48461 = CARTESIAN_POINT ( 'NONE',  ( 34.23874395593382047, -274.1199092519049714, -296.0153740787582706 ) ) ;
#48462 = DIRECTION ( 'NONE',  ( -0.000000000000000000, 1.000000000000000000, -0.000000000000000000 ) ) ;
#48463 = CARTESIAN_POINT ( 'NONE',  ( 21.05531482523297981, -281.6760586903100716, -314.2882480912825827 ) ) ;
#48464 = CARTESIAN_POINT ( 'NONE',  ( -64.93762771809339540, -278.6096719128904056, -341.8767019737751411 ) ) ;
#48465 = CARTESIAN_POINT ( 'NONE',  ( -32.30983546127264816, -285.1728684155979749, -193.7483800310014317 ) ) ;
#48466 = CARTESIAN_POINT ( 'NONE',  ( 29.64626065593770932, -294.8915279826618985, -238.7666438857950766 ) ) ;
#48467 = CARTESIAN_POINT ( 'NONE',  ( -27.12417642901079873, -275.7799538497902745, -194.7963733936756512 ) ) ;
#48468 = CARTESIAN_POINT ( 'NONE',  ( -93.79278064000719439, -274.5743418909764841, -218.7028914374340616 ) ) ;
#48469 = DIRECTION ( 'NONE',  ( 0.000000000000000000, 0.000000000000000000, -1.000000000000000000 ) ) ;
#48470 = CARTESIAN_POINT ( 'NONE',  ( -7.509593793271800877, -276.4830933680128169, -336.9872797822364987 ) ) ;
#48471 = CARTESIAN_POINT ( 'NONE',  ( -110.3756934308333655, -298.3424059734609273, -286.6725941078428832 ) ) ;
#48472 = CARTESIAN_POINT ( 'NONE',  ( -78.02491738921889919, -283.5042462350346568, -207.4911749699294887 ) ) ;
#48473 = CARTESIAN_POINT ( 'NONE',  ( -5.891690441461046923, -292.1211023267514406, -200.0855977994165471 ) ) ;
#48474 = CARTESIAN_POINT ( 'NONE',  ( 20.43913502912967317, -274.2268835606034258, -317.6382277688815634 ) ) ;
#48475 = CARTESIAN_POINT ( 'NONE',  ( -2.151864020904867836, -290.1942795054138742, -337.9489560309091871 ) ) ;
#48476 = EDGE_CURVE ( 'NONE', #57275, #12480, #24239, .T. ) ;
#48477 = CARTESIAN_POINT ( 'NONE',  ( -107.6880524943663460, -289.7448004320496580, -249.6860919924308178 ) ) ;
#48478 = ORIENTED_EDGE ( 'NONE', *, *, #77975, .T. ) ;
#48479 = CARTESIAN_POINT ( 'NONE',  ( -66.77160279676913035, -290.2487522309768337, -199.8452536505324133 ) ) ;
#48480 = CARTESIAN_POINT ( 'NONE',  ( -106.5899974854495724, -290.5264821146903387, -247.1930192287348120 ) ) ;
#48481 = ORIENTED_EDGE ( 'NONE', *, *, #34233, .F. ) ;
#48482 = CARTESIAN_POINT ( 'NONE',  ( 38.47788378599893377, -288.4859750989545546, -258.7462869889035346 ) ) ;
#48483 = CARTESIAN_POINT ( 'NONE',  ( -97.66390361071735526, -278.3130895153622646, -311.5110785389270518 ) ) ;
#48484 = CARTESIAN_POINT ( 'NONE',  ( 19.29208684184133205, -293.1790951085636152, -322.1502179590457899 ) ) ;
#48485 = CARTESIAN_POINT ( 'NONE',  ( -112.8996694329544539, -285.3859865675398169, -255.7903329040109952 ) ) ;
#48486 = CARTESIAN_POINT ( 'NONE',  ( -37.98652757589916718, -286.3775594891009746, -193.3849626536423330 ) ) ;
#48487 = CARTESIAN_POINT ( 'NONE',  ( -53.69027532592874508, -283.6009191893111847, -341.5807062375296823 ) ) ;
#48488 = CARTESIAN_POINT ( 'NONE',  ( 174.1719164811267717, 243.3713473155254974, -179.7619469166268971 ) ) ;
#48489 = CARTESIAN_POINT ( 'NONE',  ( 178.5843439615907187, 254.0915921303116818, -166.0334337346760663 ) ) ;
#48490 = CARTESIAN_POINT ( 'NONE',  ( -98.92547009169517480, -245.9928705138712814, -331.3919335924819620 ) ) ;
#48491 = CARTESIAN_POINT ( 'NONE',  ( 35.00286357884867527, -274.6047000715706190, -259.3741877010614303 ) ) ;
#48492 = CARTESIAN_POINT ( 'NONE',  ( 34.19187683319228910, -274.6838856643095710, -286.4547810613709089 ) ) ;
#48493 = CARTESIAN_POINT ( 'NONE',  ( -112.5463371017922753, -295.8565216530885209, -286.6027152311422697 ) ) ;
#48494 = ADVANCED_FACE ( 'NONE', ( #83009 ), #84876, .T. ) ;
#48495 = CARTESIAN_POINT ( 'NONE',  ( 139.7900897011093946, 178.0076021264288784, -238.7226697176948278 ) ) ;
#48496 = CARTESIAN_POINT ( 'NONE',  ( 38.24585406340965221, -274.3899969387756528, -282.5177053876520290 ) ) ;
#48497 = CARTESIAN_POINT ( 'NONE',  ( -21.74200613358737399, -276.0149943206727130, -198.0104195880617510 ) ) ;
#48498 = ORIENTED_EDGE ( 'NONE', *, *, #87845, .F. ) ;
#48499 = CARTESIAN_POINT ( 'NONE',  ( -108.6744119391808567, -297.8558996268588430, -241.8551319269994906 ) ) ;
#48500 = CARTESIAN_POINT ( 'NONE',  ( -23.76759780397865285, -289.3664951167810955, -342.2023603892083088 ) ) ;
#48501 = CARTESIAN_POINT ( 'NONE',  ( -112.7322456164178845, -297.5418981753459207, -255.4467094823427828 ) ) ;
#48502 = CARTESIAN_POINT ( 'NONE',  ( -95.52867704675838922, -297.7256810389183670, -219.9447052457241512 ) ) ;
#48503 = CARTESIAN_POINT ( 'NONE',  ( 35.20717371541275753, -293.8315864005167555, -278.9084309542953974 ) ) ;
#48504 = ORIENTED_EDGE ( 'NONE', *, *, #29582, .F. ) ;
#48505 = CARTESIAN_POINT ( 'NONE',  ( 37.71030135641018433, -277.5893913046390935, -279.5480825915715855 ) ) ;
#48506 = CARTESIAN_POINT ( 'NONE',  ( 15.12395755914652717, -280.2763467993574409, -214.0132291253211179 ) ) ;
#48507 = CARTESIAN_POINT ( 'NONE',  ( -80.94991160790036133, -278.6022145625182134, -329.1976061421860891 ) ) ;
#48508 = CARTESIAN_POINT ( 'NONE',  ( 37.22003691802383685, -277.1266701044235106, -255.7145694236638747 ) ) ;
#48509 = CARTESIAN_POINT ( 'NONE',  ( -69.61985833287917558, -275.4949673230672715, -338.4672990523591238 ) ) ;
#48510 = CARTESIAN_POINT ( 'NONE',  ( -107.5595865702545950, -297.4720976119592137, -250.0303262631050529 ) ) ;
#48511 = CARTESIAN_POINT ( 'NONE',  ( -92.64539109941854633, -294.4394483787563672, -318.9087923146258845 ) ) ;
#48512 = DIRECTION ( 'NONE',  ( -4.095251346825558428E-15, 1.000000000000000000, 0.000000000000000000 ) ) ;
#48513 = CARTESIAN_POINT ( 'NONE',  ( 24.53851280884602915, -281.4363912407335420, -224.6405957821803554 ) ) ;
#48514 = CARTESIAN_POINT ( 'NONE',  ( -3.865575368489865049, -276.7642761889835583, -335.2329075031861407 ) ) ;
#48515 = EDGE_CURVE ( 'NONE', #88799, #34891, #66379, .T. ) ;
#48516 = CARTESIAN_POINT ( 'NONE',  ( 37.24265694736835997, -286.0218015860756964, -253.2596803548573519 ) ) ;
#48517 = CARTESIAN_POINT ( 'NONE',  ( -26.56445917831958070, -300.1869189658202686, -195.1907785223500582 ) ) ;
#48518 = CARTESIAN_POINT ( 'NONE',  ( 82.67621202554614968, -297.4092476797243307, -196.6572098816457128 ) ) ;
#48519 = CARTESIAN_POINT ( 'NONE',  ( 8.072200834668189273, -287.6098455814253043, -327.7212027607546929 ) ) ;
#48520 = CARTESIAN_POINT ( 'NONE',  ( -5.097046267291682753, -278.7224341710114004, -203.7408784592001609 ) ) ;
#48522 = CARTESIAN_POINT ( 'NONE',  ( -76.91292002685007390, -281.6660331980692149, -333.4731236785188457 ) ) ;
#48521 = CARTESIAN_POINT ( 'NONE',  ( -51.92652732298921592, -278.4367009428111714, -198.1795208908974644 ) ) ;
#48523 = CARTESIAN_POINT ( 'NONE',  ( 37.67126975303213499, -289.5831405755807282, -272.7617249258289007 ) ) ;
#48524 = CARTESIAN_POINT ( 'NONE',  ( -96.40344299156578245, -279.1495234529978688, -313.9578722329522975 ) ) ;
#48525 = CYLINDRICAL_SURFACE ( 'NONE', #45712, 2.999999999999999556 ) ;
#48526 = CARTESIAN_POINT ( 'NONE',  ( 23.18494719328650788, -294.9485837885573574, -226.0720040256993855 ) ) ;
#48527 = CARTESIAN_POINT ( 'NONE',  ( -56.68796319367613989, -275.5379502510399448, -343.8980754507609277 ) ) ;
#48528 = CARTESIAN_POINT ( 'NONE',  ( -24.30328498879935140, -277.5328323974271143, -342.3424154904254806 ) ) ;
#48529 = CARTESIAN_POINT ( 'NONE',  ( 14.50778077475415984, -284.3248188407257544, -324.7822513295351996 ) ) ;
#48530 = CARTESIAN_POINT ( 'NONE',  ( 198.6884013828325521, 64.61450673763174279, 9.555809373750797420 ) ) ;
#48531 = CARTESIAN_POINT ( 'NONE',  ( -109.4010151578765999, -292.1792126301169219, -293.2644311013637548 ) ) ;
#48532 = CARTESIAN_POINT ( 'NONE',  ( -110.6491284464200504, -294.3477994234162338, -286.2643238697359038 ) ) ;
#48533 = CARTESIAN_POINT ( 'NONE',  ( -97.44768269725072685, -284.3915695113563515, -222.4922378949848678 ) ) ;
#48534 = CARTESIAN_POINT ( 'NONE',  ( 200.3359402460285139, 61.72811464988816965, -8.999999999999998224 ) ) ;
#48535 = CARTESIAN_POINT ( 'NONE',  ( -8.763707148622318144, -273.1187530463055282, -202.5975911649564694 ) ) ;
#48536 = CARTESIAN_POINT ( 'NONE',  ( -37.52968995737902702, -290.1893948565007122, -196.1134975340727067 ) ) ;
#48537 = DIRECTION ( 'NONE',  ( -0.000000000000000000, 1.000000000000000000, -0.000000000000000000 ) ) ;
#48538 = CARTESIAN_POINT ( 'NONE',  ( 175.2296996224750103, 140.2072866198470251, 21.95310499597075804 ) ) ;
#48539 = CARTESIAN_POINT ( 'NONE',  ( -76.79406813884942551, -290.0143276955342344, -204.9838922623639235 ) ) ;
#48540 = CARTESIAN_POINT ( 'NONE',  ( -108.5274800976382039, -285.8972967721289820, -289.8773481186418053 ) ) ;
#48541 = CARTESIAN_POINT ( 'NONE',  ( 31.79942591476769920, -285.3822833631823528, -238.7148740462976093 ) ) ;
#48542 = CARTESIAN_POINT ( 'NONE',  ( -108.3247488557336311, -285.7224689388157230, -289.8195149053919977 ) ) ;
#48543 = CARTESIAN_POINT ( 'NONE',  ( -41.34195792098572042, -286.8033705861726617, -197.2965581104351998 ) ) ;
#48544 = EDGE_CURVE ( 'NONE', #69489, #86306, #31632, .T. ) ;
#48545 = CARTESIAN_POINT ( 'NONE',  ( 35.86818148910214177, -295.7608560810044196, -288.2679181945184155 ) ) ;
#48546 = CARTESIAN_POINT ( 'NONE',  ( 19.71648825643512737, -274.3143712625620196, -319.9153000638197000 ) ) ;
#48547 = CARTESIAN_POINT ( 'NONE',  ( 35.70854587149006676, -275.5778372274126014, -245.9154365035611818 ) ) ;
#48548 = CARTESIAN_POINT ( 'NONE',  ( 33.12884984009559020, -291.2784084006629541, -242.9544201776374734 ) ) ;
#48549 = CARTESIAN_POINT ( 'NONE',  ( -111.8274409895666821, -278.3072764748673649, -289.9289303317952999 ) ) ;
#48550 = CARTESIAN_POINT ( 'NONE',  ( -100.1028850609206557, -297.9839955258374289, -310.8646754240701284 ) ) ;
#48551 = DIRECTION ( 'NONE',  ( 0.000000000000000000, 1.000000000000000000, 0.000000000000000000 ) ) ;
#48552 = DIRECTION ( 'NONE',  ( 1.000000000000000000, 0.000000000000000000, -0.000000000000000000 ) ) ;
#48553 = CARTESIAN_POINT ( 'NONE',  ( -109.4092864213582033, -283.4257270079277191, -255.9560325915904571 ) ) ;
#48554 = CARTESIAN_POINT ( 'NONE',  ( -103.0293296677127870, -277.0333375170012573, -234.1653175139212237 ) ) ;
#48555 = CARTESIAN_POINT ( 'NONE',  ( 165.2494399300530290, -11.64849832608277325, 10.00000000000000000 ) ) ;
#48556 = CARTESIAN_POINT ( 'NONE',  ( 37.22398974777998149, -274.2373383866365089, -286.6290596188400173 ) ) ;
#48557 = CARTESIAN_POINT ( 'NONE',  ( -69.30346389650966898, -276.8326780654829236, -336.1194676859682318 ) ) ;
#48558 = CARTESIAN_POINT ( 'NONE',  ( 21.89522449714161922, -295.6811020158600058, -314.1982542349576875 ) ) ;
#48559 = CARTESIAN_POINT ( 'NONE',  ( -31.08520886551058737, -279.0496433150603366, -193.8733797925853253 ) ) ;
#48560 = CARTESIAN_POINT ( 'NONE',  ( -80.28308419656772799, -296.5913547891394728, -329.6860367077647993 ) ) ;
#48561 = CARTESIAN_POINT ( 'NONE',  ( -83.87191789193516911, -296.9909501468564486, -331.1587595875762418 ) ) ;
#48562 = CARTESIAN_POINT ( 'NONE',  ( -84.07320627970419480, -297.2224491615630768, -214.2133381966015691 ) ) ;
#48563 = CARTESIAN_POINT ( 'NONE',  ( -102.8835268438573394, -293.0387598443886645, -233.7952358678388691 ) ) ;
#48564 = CARTESIAN_POINT ( 'NONE',  ( -40.81859718022990791, -286.1763649603586259, -193.3874638339882210 ) ) ;
#48565 = CARTESIAN_POINT ( 'NONE',  ( 37.51159335903436443, -273.8448430344791404, -282.4068221268042862 ) ) ;
#48566 = CARTESIAN_POINT ( 'NONE',  ( -5.628433901237086090, -288.4797803625827441, -340.5271264891952683 ) ) ;
#48567 = CARTESIAN_POINT ( 'NONE',  ( -70.49298316036426115, -281.5928280043658560, -203.4676691104416477 ) ) ;
#48568 = ADVANCED_FACE ( 'NONE', ( #20027 ), #61725, .T. ) ;
#48569 = CARTESIAN_POINT ( 'NONE',  ( -68.86539035052989277, -284.6859499126771311, -204.2438406562552586 ) ) ;
#48570 = B_SPLINE_CURVE_WITH_KNOTS ( 'NONE', 3,
 ( #18832, #68082, #17434, #32575, #91231, #11251, #3207, #89840, #40106, #54329, #26397, #76118, #47687, #82739, #69021, #55285, #17892, #90750, #84139, #12180, #25908, #76589, #69478, #33483, #46745, #62387, #19288, #48147, #77051, #41023, #69948 ),
 .UNSPECIFIED., .F., .F.,
 ( 4, 2, 2, 2, 2, 2, 2, 2, 2, 2, 2, 1, 2, 2, 2, 4 ),
 ( 0.000000000000000000, 0.006842119823167555626, 0.01026317973475138201, 0.01368423964633520840, 0.02052635946950286117, 0.02223688942529476048, 0.02394741938108666326, 0.02736847929267014964, 0.03421059911583700791, 0.03592112907162879620, 0.03763165902742058450, 0.04105271893900415414, 0.04447377885058772379, 0.04618430880637957453, 0.04789483876217142527, 0.05473695858533866865 ),
 .UNSPECIFIED. ) ;
#48571 = CARTESIAN_POINT ( 'NONE',  ( -89.37944076373352686, -289.3196994197348886, -216.2791188411365795 ) ) ;
#48572 = CARTESIAN_POINT ( 'NONE',  ( 193.8665746513534316, 275.1768195097669150, -123.9090917457166938 ) ) ;
#48573 = CARTESIAN_POINT ( 'NONE',  ( -30.51929870519063570, -285.6482580331405643, -197.5679691028414595 ) ) ;
#48574 = LINE ( 'NONE', #85030, #61143 ) ;
#48575 = CARTESIAN_POINT ( 'NONE',  ( 37.91724765769303929, -282.6831987777285349, -285.4909227368766551 ) ) ;
#48576 = EDGE_CURVE ( 'NONE', #12173, #30016, #49082, .T. ) ;
#48577 = CARTESIAN_POINT ( 'NONE',  ( -112.9038302107002778, -289.4401844526968830, -283.9700036400129193 ) ) ;
#48578 = CARTESIAN_POINT ( 'NONE',  ( 36.89345403409696900, -282.9343461429411377, -253.1113499512093199 ) ) ;
#48579 = CARTESIAN_POINT ( 'NONE',  ( -104.5344324371445595, -279.3908246714688062, -306.9457458526396181 ) ) ;
#48580 = CARTESIAN_POINT ( 'NONE',  ( 35.70279637953220941, -281.3980658527124774, -271.3158764120159958 ) ) ;
#48581 = CARTESIAN_POINT ( 'NONE',  ( -18.80118689711731506, -276.2909034945998314, -197.6350496608846186 ) ) ;
#48582 = CARTESIAN_POINT ( 'NONE',  ( -79.47696455969719409, -295.6044586643631646, -334.8096981940573755 ) ) ;
#48583 = CARTESIAN_POINT ( 'NONE',  ( -107.2422238976989064, -288.9156423444279653, -244.0274977234545304 ) ) ;
#48584 = CARTESIAN_POINT ( 'NONE',  ( -35.79364542511192582, -296.9923055376416983, -197.0522957913235871 ) ) ;
#48585 = ORIENTED_EDGE ( 'NONE', *, *, #61465, .F. ) ;
#48586 = EDGE_LOOP ( 'NONE', ( #65566, #9240, #24506, #9137 ) ) ;
#48587 = CARTESIAN_POINT ( 'NONE',  ( 12.90637352302024787, -284.2642277782934457, -325.2832928299513924 ) ) ;
#48588 = CARTESIAN_POINT ( 'NONE',  ( -101.4879127869722026, -295.7427776016064627, -305.2516738424444611 ) ) ;
#48589 = CARTESIAN_POINT ( 'NONE',  ( -40.63297081429274016, -293.0913668607279305, -193.7277561580065992 ) ) ;
#48590 = CARTESIAN_POINT ( 'NONE',  ( -86.99199381964908184, -284.4165389495634031, -324.0842638890283069 ) ) ;
#48591 = CARTESIAN_POINT ( 'NONE',  ( 38.26246997598464361, -274.4431446383857178, -256.9882097258093268 ) ) ;
#48592 = CARTESIAN_POINT ( 'NONE',  ( -113.0314947971882731, -291.0325923373216597, -284.0136592794058288 ) ) ;
#48593 = CARTESIAN_POINT ( 'NONE',  ( -111.3241663741660545, -282.4840936314431019, -286.6981976738247226 ) ) ;
#48594 = CARTESIAN_POINT ( 'NONE',  ( -96.37210939784807806, -290.2201101636690055, -319.7896087343793283 ) ) ;
#48595 = CARTESIAN_POINT ( 'NONE',  ( 35.47333885171664036, -287.9661155069417191, -276.4788832650269796 ) ) ;
#48596 = FACE_OUTER_BOUND ( 'NONE', #36358, .T. ) ;
#48597 = CARTESIAN_POINT ( 'NONE',  ( 219.8344101925596021, 0.000000000000000000, -7.000000000000000888 ) ) ;
#48598 = CARTESIAN_POINT ( 'NONE',  ( 153.5077555025204674, 204.5572234277026951, -214.3296801316302833 ) ) ;
#48599 = CARTESIAN_POINT ( 'NONE',  ( -63.65460609925754909, -284.9091580461238777, -341.9875009121750509 ) ) ;
#48600 = CARTESIAN_POINT ( 'NONE',  ( -106.6662871844225293, -287.6237833571633473, -303.7098442033569086 ) ) ;
#48601 = ORIENTED_EDGE ( 'NONE', *, *, #46545, .F. ) ;
#48602 = CARTESIAN_POINT ( 'NONE',  ( 28.42231367664016517, -280.9109646802627935, -302.8694950075523025 ) ) ;
#48603 = CARTESIAN_POINT ( 'NONE',  ( 3.486687757114208086, -276.1861857862203919, -335.6832454544615416 ) ) ;
#48604 = CARTESIAN_POINT ( 'NONE',  ( -69.32950092992300029, -281.6304327545341266, -202.7090002712346575 ) ) ;
#48605 = CARTESIAN_POINT ( 'NONE',  ( -110.6141395889435444, -273.5598078522675110, -270.3739478531805389 ) ) ;
#48606 = CARTESIAN_POINT ( 'NONE',  ( 30.54527415402887414, -280.5824565906594330, -305.4319750315027022 ) ) ;
#48607 = CARTESIAN_POINT ( 'NONE',  ( -108.0831924592627757, -282.8836220214131458, -246.3774263537814022 ) ) ;
#48608 = CARTESIAN_POINT ( 'NONE',  ( -109.8263395877805806, -298.0214310851353616, -293.2070633060387763 ) ) ;
#48609 = CARTESIAN_POINT ( 'NONE',  ( 18.51959070595551893, -293.3760210719144084, -223.2707301291225974 ) ) ;
#48610 = VERTEX_POINT ( 'NONE', #69287 ) ;
#48611 = CARTESIAN_POINT ( 'NONE',  ( -110.1136098019441221, -289.1012062508485769, -280.7225087094647620 ) ) ;
#48612 = CARTESIAN_POINT ( 'NONE',  ( -11.89208267636104566, -277.3809297720416680, -342.9816323633611432 ) ) ;
#48613 = CARTESIAN_POINT ( 'NONE',  ( -40.52009549172851166, -298.1777894119178995, -197.4177951610524815 ) ) ;
#48614 = EDGE_LOOP ( 'NONE', ( #71440, #8111, #75262 ) ) ;
#48615 = CARTESIAN_POINT ( 'NONE',  ( -69.98764049375895979, -272.5525468762258470, -200.9512658247716388 ) ) ;
#48616 = LINE ( 'NONE', #5564, #65824 ) ;
#48617 = CARTESIAN_POINT ( 'NONE',  ( 219.8344101925596021, 35.72494958537217968, 7.000000000000000000 ) ) ;
#48618 = CARTESIAN_POINT ( 'NONE',  ( 157.2528655986780564, 19.19772955881679621, 10.67418916507565640 ) ) ;
#48619 = CARTESIAN_POINT ( 'NONE',  ( 30.62624173263163385, -282.9981252987232665, -297.8308277024957533 ) ) ;
#48620 = CARTESIAN_POINT ( 'NONE',  ( 36.00097875808192072, -283.0595617717870027, -250.4416142702418142 ) ) ;
#48621 = CARTESIAN_POINT ( 'NONE',  ( -99.23629206093487198, -283.0705484777093375, -309.6028282686647231 ) ) ;
#48622 = CARTESIAN_POINT ( 'NONE',  ( 21.48038547099317341, -282.7855586275067594, -225.0544016685380200 ) ) ;
#48623 = CARTESIAN_POINT ( 'NONE',  ( 28.64276842741217166, -274.4741628800491071, -303.2900804249841826 ) ) ;
#48624 = CARTESIAN_POINT ( 'NONE',  ( 175.2296996224750103, 214.5000000000000568, -25.00000000000000355 ) ) ;
#48625 = CARTESIAN_POINT ( 'NONE',  ( 32.81619808134219340, -276.9126943323491901, -291.6671964193691338 ) ) ;
#48626 = DIRECTION ( 'NONE',  ( -0.7981962569173501887, 0.000000000000000000, -0.6023974895724014678 ) ) ;
#48627 = B_SPLINE_CURVE_WITH_KNOTS ( 'NONE', 3,
 ( #73894, #1009, #66344, #80068 ),
 .UNSPECIFIED., .F., .F.,
 ( 4, 4 ),
 ( 0.000000000000000000, 1.000000000000000000 ),
 .UNSPECIFIED. ) ;
#48628 = CARTESIAN_POINT ( 'NONE',  ( -68.93960902322382367, -278.2599749774199154, -340.4164149230530825 ) ) ;
#48629 = VERTEX_POINT ( 'NONE', #7228 ) ;
#48630 = ORIENTED_EDGE ( 'NONE', *, *, #14407, .F. ) ;
#48631 = CARTESIAN_POINT ( 'NONE',  ( 199.1517898866434848, 16.71555987447338509, 10.28330198088196568 ) ) ;
#48632 = CARTESIAN_POINT ( 'NONE',  ( -109.7526578126973362, -286.6991158459916846, -247.8917827598084216 ) ) ;
#48633 = EDGE_CURVE ( 'NONE', #557, #46575, #79958, .T. ) ;
#48634 = CARTESIAN_POINT ( 'NONE',  ( 16.27052435803078723, -293.4632947254200985, -320.1439575232039942 ) ) ;
#48635 = CARTESIAN_POINT ( 'NONE',  ( 7.867873377023919979, -287.8014451439553341, -332.6313369672537874 ) ) ;
#48636 = CARTESIAN_POINT ( 'NONE',  ( -94.01680278720040462, -283.4587832512517025, -222.7595764697107938 ) ) ;
#48638 = CARTESIAN_POINT ( 'NONE',  ( -34.56209227983678289, -287.2567436409054267, -344.3725126396180940 ) ) ;
#48637 = CARTESIAN_POINT ( 'NONE',  ( -105.7684773673082788, -282.7659416136862092, -297.5766785372172194 ) ) ;
#48639 = CARTESIAN_POINT ( 'NONE',  ( -102.1144633797219541, -285.2880576461042779, -304.9890918100404633 ) ) ;
#48640 = CARTESIAN_POINT ( 'NONE',  ( -35.77939073807909409, -275.0324271141458894, -345.3576315030629758 ) ) ;
#48641 = CIRCLE ( 'NONE', #77388, 2.000000000000001776 ) ;
#48642 = CARTESIAN_POINT ( 'NONE',  ( 22.37775995481749547, -285.3118579654935729, -223.0113948479123565 ) ) ;
#48643 = CARTESIAN_POINT ( 'NONE',  ( -34.86830155287925948, -300.0832707502397056, -195.3602660063473877 ) ) ;
#48644 = CARTESIAN_POINT ( 'NONE',  ( -32.40086865808414274, -284.1141308801414311, -195.3441546556174728 ) ) ;
#48645 = CIRCLE ( 'NONE', #38090, 0.5000000000000004441 ) ;
#48646 = CARTESIAN_POINT ( 'NONE',  ( 2.823044080410989309, -281.5466186746336348, -209.0613828178042581 ) ) ;
#48647 = CARTESIAN_POINT ( 'NONE',  ( 34.63735439783157233, -289.8312778957915725, -292.0633002730257317 ) ) ;
#48648 = CARTESIAN_POINT ( 'NONE',  ( 129.8975571001389540, -299.5541904835127980, -189.5200328990441676 ) ) ;
#48649 = CARTESIAN_POINT ( 'NONE',  ( 115.2448031289451222, -299.5541904835127980, -195.3611179825600175 ) ) ;
#48650 = CARTESIAN_POINT ( 'NONE',  ( -5.094472566048152018, -296.5511684722085306, -338.7085512838760337 ) ) ;
#48651 = TOROIDAL_SURFACE ( 'NONE', #29002, 24.00000000000002132, 2.046895004029262388 ) ;
#48652 = CARTESIAN_POINT ( 'NONE',  ( -98.00890200388300855, -277.1527077877407237, -226.2647318786002018 ) ) ;
#48653 = CARTESIAN_POINT ( 'NONE',  ( -92.68866013613964583, -290.4812271823700485, -216.9855939435808523 ) ) ;
#48654 = CARTESIAN_POINT ( 'NONE',  ( -87.04362444260598863, -294.1580886682608593, -324.9153032753341108 ) ) ;
#48655 = CARTESIAN_POINT ( 'NONE',  ( -94.31226766204004264, -277.8897917451836292, -223.9327008822564835 ) ) ;
#48656 = CARTESIAN_POINT ( 'NONE',  ( -72.56799164928743551, -271.6622520192747174, -204.7260835902301892 ) ) ;
#48657 = CARTESIAN_POINT ( 'NONE',  ( 31.05059737066502734, -295.2263190217694842, -297.4028006318079633 ) ) ;
#48658 = CARTESIAN_POINT ( 'NONE',  ( -95.95921662488163406, -298.4090924074130271, -317.1477375740089997 ) ) ;
#48659 = CARTESIAN_POINT ( 'NONE',  ( -75.41700247900409693, -296.0343040350450110, -204.1719798737433962 ) ) ;
#48660 = CARTESIAN_POINT ( 'NONE',  ( -16.87768598829033451, -290.5527697436305630, -197.1818986863124792 ) ) ;
#48661 = CARTESIAN_POINT ( 'NONE',  ( -106.2688782327282553, -292.3202583836008444, -244.4401000466931464 ) ) ;
#48662 = CYLINDRICAL_SURFACE ( 'NONE', #82312, 4.999999999999990230 ) ;
#48663 = CARTESIAN_POINT ( 'NONE',  ( -64.14025613729464226, -292.4962417075998928, -202.2708391292083263 ) ) ;
#48664 = DIRECTION ( 'NONE',  ( -1.000000000000000000, 0.000000000000000000, 0.000000000000000000 ) ) ;
#48665 = CARTESIAN_POINT ( 'NONE',  ( -97.16315361736587874, -292.4014366067572723, -222.5134176920644791 ) ) ;
#48667 = CARTESIAN_POINT ( 'NONE',  ( 14.87550773271745008, -292.8133860569886906, -219.2753541556567995 ) ) ;
#48666 = CARTESIAN_POINT ( 'NONE',  ( 28.31612186058764991, -280.0637668547256567, -307.4465468986252858 ) ) ;
#48668 = CARTESIAN_POINT ( 'NONE',  ( 30.72181242903524279, -281.0859349570575318, -234.2424698133636412 ) ) ;
#48669 = CARTESIAN_POINT ( 'NONE',  ( -47.25784273800507407, -282.8415961742917375, -346.6986212637596623 ) ) ;
#48670 = CARTESIAN_POINT ( 'NONE',  ( -72.04502145922313616, -287.5119327611447488, -336.6757324763734687 ) ) ;
#48671 = CARTESIAN_POINT ( 'NONE',  ( -18.44368065994072126, -280.9458212278611313, -342.2038899071018250 ) ) ;
#48672 = CARTESIAN_POINT ( 'NONE',  ( -56.36492323362677581, -278.2913641307645207, -196.4092236741880129 ) ) ;
#48673 = CARTESIAN_POINT ( 'NONE',  ( -21.03623025897670828, -285.1769925888909825, -195.4236496424816778 ) ) ;
#48674 = CARTESIAN_POINT ( 'NONE',  ( 195.1454508245391537, 40.17711433623591688, 15.11173962605491461 ) ) ;
#48675 = CARTESIAN_POINT ( 'NONE',  ( -5.717094902473006002, -294.0752255445763126, -203.6664197533825700 ) ) ;
#48676 = CARTESIAN_POINT ( 'NONE',  ( 27.98926628453845922, -276.4549636358787552, -230.6308349732857153 ) ) ;
#48677 = CARTESIAN_POINT ( 'NONE',  ( -32.42337306950857823, -276.6552935947437959, -343.2664181305506759 ) ) ;
#48678 = CARTESIAN_POINT ( 'NONE',  ( -96.58022936636687916, -291.3804808366754742, -221.1493126920573502 ) ) ;
#48679 = CARTESIAN_POINT ( 'NONE',  ( -34.55699062133827937, -281.0972555984808992, -345.8697902880177253 ) ) ;
#48680 = CARTESIAN_POINT ( 'NONE',  ( 30.07703001190188630, -292.2265660479265534, -241.6284717467557925 ) ) ;
#48681 = CARTESIAN_POINT ( 'NONE',  ( -111.1658611851397040, -294.7218451615552794, -257.1325921787241668 ) ) ;
#48682 = ORIENTED_EDGE ( 'NONE', *, *, #55414, .T. ) ;
#48683 = CARTESIAN_POINT ( 'NONE',  ( 21.04675612459715950, -292.4436093660203255, -226.4432785746563468 ) ) ;
#48684 = FACE_OUTER_BOUND ( 'NONE', #18906, .T. ) ;
#48685 = CARTESIAN_POINT ( 'NONE',  ( -21.33282851196157992, -289.7666405000204009, -200.3683826091710216 ) ) ;
#48686 = CARTESIAN_POINT ( 'NONE',  ( -112.0794853578401273, -295.3903608627329618, -287.9418139558929397 ) ) ;
#48687 = CARTESIAN_POINT ( 'NONE',  ( 32.05127500298549847, -279.2975804070017602, -239.9486126536436643 ) ) ;
#48688 = CARTESIAN_POINT ( 'NONE',  ( -2.462770587989639104, -287.8189127430741223, -202.2527129722085419 ) ) ;
#48689 = CARTESIAN_POINT ( 'NONE',  ( 2.448791765869307024, -286.4353333299612814, -209.1588569186809536 ) ) ;
#48690 = CARTESIAN_POINT ( 'NONE',  ( -32.35448218255530151, -278.5083975788343196, -343.9359449434364251 ) ) ;
#48691 = CARTESIAN_POINT ( 'NONE',  ( -106.2716475864877879, -294.9479352107847490, -241.7165872052857196 ) ) ;
#48692 = CARTESIAN_POINT ( 'NONE',  ( -110.1347373103682656, -298.1372364562573694, -283.8158207499173500 ) ) ;
#48693 = EDGE_CURVE ( 'NONE', #37428, #60407, #25532, .T. ) ;
#48694 = CARTESIAN_POINT ( 'NONE',  ( -108.2076255699320200, -277.0960325370430155, -289.4700456591623947 ) ) ;
#48695 = VERTEX_POINT ( 'NONE', #6775 ) ;
#48696 = LINE ( 'NONE', #27409, #68257 ) ;
#48697 = CARTESIAN_POINT ( 'NONE',  ( -107.1489830521686315, -295.8035128274034946, -302.8062646487720713 ) ) ;
#48698 = CARTESIAN_POINT ( 'NONE',  ( -108.3178125325267018, -292.1785513154541150, -292.9748155868963408 ) ) ;
#48699 = CARTESIAN_POINT ( 'NONE',  ( 195.9765076956177268, 73.46773880466290052, -12.06523745212588139 ) ) ;
#48700 = ADVANCED_FACE ( 'NONE', ( #14807 ), #92043, .T. ) ;
#48701 = CARTESIAN_POINT ( 'NONE',  ( -31.85543656554987280, -289.6326526977358071, -343.3075840503252607 ) ) ;
#48702 = ORIENTED_EDGE ( 'NONE', *, *, #16793, .F. ) ;
#48703 = CARTESIAN_POINT ( 'NONE',  ( -19.79831161777381610, -279.3309790245659201, -195.5733223984542235 ) ) ;
#48704 = CARTESIAN_POINT ( 'NONE',  ( -95.49896296905055237, -296.5230147947148680, -320.6706157507477428 ) ) ;
#48705 = CARTESIAN_POINT ( 'NONE',  ( -72.83377190921757460, -289.7267650075502274, -203.4090383468069660 ) ) ;
#48706 = CARTESIAN_POINT ( 'NONE',  ( -111.6028049752585787, -297.1416555585039987, -249.8901708905887062 ) ) ;
#48708 = CARTESIAN_POINT ( 'NONE',  ( 21.34599126082868992, -294.4944530964592104, -313.8104259894918755 ) ) ;
#48707 = AXIS2_PLACEMENT_3D ( 'NONE', #19182, #48512, #11134 ) ;
#48709 = CARTESIAN_POINT ( 'NONE',  ( 199.4392256788250961, 65.82574266882505754, -7.741079165001063522 ) ) ;
#48710 = AXIS2_PLACEMENT_3D ( 'NONE', #68021, #67564, #31575 ) ;
#48711 = LINE ( 'NONE', #42070, #11371 ) ;
#48712 = CARTESIAN_POINT ( 'NONE',  ( 23.60026902073524724, -289.6892833505908698, -316.2826178583721344 ) ) ;
#48713 = CARTESIAN_POINT ( 'NONE',  ( 40.65961533371913106, -284.2662352645559167, -288.1317622949166548 ) ) ;
#48714 = ORIENTED_EDGE ( 'NONE', *, *, #37168, .T. ) ;
#48715 = VECTOR ( 'NONE', #55205, 1000.000000000000000 ) ;
#48716 = CARTESIAN_POINT ( 'NONE',  ( 17.15673458860114309, -280.1530075973298040, -216.0348683170665254 ) ) ;
#48717 = CARTESIAN_POINT ( 'NONE',  ( -112.0604175095280368, -286.6165758692659438, -265.3676268376449343 ) ) ;
#48718 = CARTESIAN_POINT ( 'NONE',  ( 39.11262168029700348, -286.1419939503098817, -271.5602958330769070 ) ) ;
#48719 = CARTESIAN_POINT ( 'NONE',  ( -84.32226885479330747, -271.4038055219076000, -212.1129026839008702 ) ) ;
#48720 = CARTESIAN_POINT ( 'NONE',  ( -84.11398248106308984, -275.3234891689962183, -212.4502571845264640 ) ) ;
#48722 = CARTESIAN_POINT ( 'NONE',  ( -91.79622353690605507, -289.3479024907310304, -219.5877803274311191 ) ) ;
#48721 = AXIS2_PLACEMENT_3D ( 'NONE', #76042, #55211, #54254 ) ;
#48723 = CARTESIAN_POINT ( 'NONE',  ( -51.06525538948874754, -279.0861702300503566, -344.8726574175473729 ) ) ;
#48725 = CARTESIAN_POINT ( 'NONE',  ( -7.950860760758045487, -279.7962448637267698, -203.4140914288397823 ) ) ;
#48724 = CARTESIAN_POINT ( 'NONE',  ( -93.09020038426017152, -279.2221087320643278, -223.2132920592192136 ) ) ;
#48726 = CARTESIAN_POINT ( 'NONE',  ( -2.851758475184907216, -277.6867484368544297, -338.8734492916458407 ) ) ;
#48727 = CARTESIAN_POINT ( 'NONE',  ( -94.65446285177091568, -278.0392945534433125, -219.5353769835632818 ) ) ;
#48728 = CARTESIAN_POINT ( 'NONE',  ( -32.42903041750177806, -123.8281167454940999, -361.7435837593322390 ) ) ;
#48729 = CARTESIAN_POINT ( 'NONE',  ( -41.19299589062352140, -274.9461739899020358, -193.6409824334107839 ) ) ;
#48730 = CARTESIAN_POINT ( 'NONE',  ( -102.1405766910263964, -274.6042108955197705, -230.0645505358623097 ) ) ;
#48731 = CARTESIAN_POINT ( 'NONE',  ( -110.4683760289727132, -293.2662352645559167, -253.7030783399848985 ) ) ;
#48732 = ORIENTED_EDGE ( 'NONE', *, *, #2955, .F. ) ;
#48733 = CARTESIAN_POINT ( 'NONE',  ( 82.64126209800332390, -300.1542085700246503, -192.9280458966490528 ) ) ;
#48734 = CARTESIAN_POINT ( 'NONE',  ( 25.20733400835214155, -288.1072502891944396, -232.1270441503878033 ) ) ;
#48735 = CARTESIAN_POINT ( 'NONE',  ( 36.16985707124061378, -289.5562826470426216, -289.5971512037937714 ) ) ;
#48736 = CARTESIAN_POINT ( 'NONE',  ( 34.85859135095023476, -287.0525672471521261, -281.8868190740270734 ) ) ;
#48737 = CARTESIAN_POINT ( 'NONE',  ( -76.73178316510245622, -283.0718821535951406, -336.5133457140380528 ) ) ;
#48738 = CARTESIAN_POINT ( 'NONE',  ( -59.95964621383821935, -278.1541272356391801, -200.0586118444897465 ) ) ;
#48739 = CARTESIAN_POINT ( 'NONE',  ( -5.286379073223693048, -288.3388638479190149, -203.3894899003055343 ) ) ;
#48740 = CARTESIAN_POINT ( 'NONE',  ( 34.61324238663527098, -280.2399601952778312, -286.2731889461723540 ) ) ;
#48741 = CARTESIAN_POINT ( 'NONE',  ( -91.67260161652997397, -280.5722119163197590, -220.8697387136645318 ) ) ;
#48742 = CARTESIAN_POINT ( 'NONE',  ( -16.35720136710627415, -277.2659766378330346, -340.3973085479157135 ) ) ;
#48743 = CARTESIAN_POINT ( 'NONE',  ( -37.51616981767915604, -287.8491851459787654, -346.9768523904389781 ) ) ;
#48744 = CARTESIAN_POINT ( 'NONE',  ( -66.50547387911690578, -284.2273124513799303, -341.4641831580120197 ) ) ;
#48745 = CARTESIAN_POINT ( 'NONE',  ( -108.1680342657487301, -284.6601246523491113, -300.5499602784155968 ) ) ;
#48746 = CARTESIAN_POINT ( 'NONE',  ( -1.250160080634530324, -282.7256401586120660, -333.8150441141625038 ) ) ;
#48747 = ORIENTED_EDGE ( 'NONE', *, *, #52360, .F. ) ;
#48748 = ORIENTED_EDGE ( 'NONE', *, *, #4833, .T. ) ;
#48749 = CARTESIAN_POINT ( 'NONE',  ( 194.3470905245161191, 19.98788413800966168, -14.59400273035306483 ) ) ;
#48750 = CARTESIAN_POINT ( 'NONE',  ( -110.4473060167651681, -292.6663860667849235, -250.4152013358639124 ) ) ;
#48751 = CARTESIAN_POINT ( 'NONE',  ( 22.73133772193494906, -291.5990471942290014, -222.9637230989866623 ) ) ;
#48752 = CARTESIAN_POINT ( 'NONE',  ( -8.868317561797425697, -273.4926146706915802, -202.8335151676897681 ) ) ;
#48753 = CARTESIAN_POINT ( 'NONE',  ( 8.838316208477916547, -293.7858326752867697, -331.8486685715480462 ) ) ;
#48754 = CARTESIAN_POINT ( 'NONE',  ( -87.21269467351521598, -288.2417882476885893, -324.6852384590505380 ) ) ;
#48755 = CARTESIAN_POINT ( 'NONE',  ( 35.31491773729234751, -291.9755473941751802, -284.4674958264220663 ) ) ;
#48756 = CARTESIAN_POINT ( 'NONE',  ( -96.87172919699636964, -291.1600270849020262, -313.2948593123961700 ) ) ;
#48757 = CARTESIAN_POINT ( 'NONE',  ( 156.8041522122653930, 250.5000000000000568, 16.89672165344857646 ) ) ;
#48758 = CARTESIAN_POINT ( 'NONE',  ( -81.65004257335596094, -291.6555331179454811, -330.8736905244816171 ) ) ;
#48759 = CARTESIAN_POINT ( 'NONE',  ( 33.72776378554834764, -291.2341105423036538, -245.7256645272244384 ) ) ;
#48760 = CARTESIAN_POINT ( 'NONE',  ( 6.717849444255739044, -294.6510772731249972, -209.6039066691162702 ) ) ;
#48761 = CARTESIAN_POINT ( 'NONE',  ( 16.13812384942448475, -287.7757202324366403, -220.3094575983584207 ) ) ;
#48762 = CARTESIAN_POINT ( 'NONE',  ( 34.62208415254949045, -295.8334690835096126, -292.2457552112653616 ) ) ;
#48763 = CARTESIAN_POINT ( 'NONE',  ( 20.57027291757417231, -276.8693526485226357, -222.1469065468835709 ) ) ;
#48764 = CARTESIAN_POINT ( 'NONE',  ( -33.33465842890517905, -297.2982953954544314, -193.5231230048669886 ) ) ;
#48765 = CARTESIAN_POINT ( 'NONE',  ( -9.629465080767708685, -274.9249340678638873, -339.0043537721063558 ) ) ;
#48766 = CARTESIAN_POINT ( 'NONE',  ( -4.909440609980757486, -278.5624472350443739, -203.3576647534698907 ) ) ;
#48767 = CARTESIAN_POINT ( 'NONE',  ( -94.09514317038249942, -274.4131280210744421, -223.7992525931428531 ) ) ;
#48768 = CARTESIAN_POINT ( 'NONE',  ( 22.30983858929492314, -273.4821179802898996, -222.5878733686120654 ) ) ;
#48769 = CARTESIAN_POINT ( 'NONE',  ( -110.9641573957463692, -297.9986740797583025, -268.7378648852824767 ) ) ;
#48770 = DIRECTION ( 'NONE',  ( 0.000000000000000000, 0.000000000000000000, 1.000000000000000000 ) ) ;
#48771 = CARTESIAN_POINT ( 'NONE',  ( -106.8634283265061953, -297.6586798984685629, -247.4116025793694007 ) ) ;
#48772 = DIRECTION ( 'NONE',  ( 0.000000000000000000, 0.000000000000000000, 1.000000000000000000 ) ) ;
#48773 = CIRCLE ( 'NONE', #26129, 3.000000000000000000 ) ;
#48775 = CARTESIAN_POINT ( 'NONE',  ( -47.27274760131920317, -297.9225879078319394, -197.9885806972592661 ) ) ;
#48774 = CARTESIAN_POINT ( 'NONE',  ( 36.41883083574412439, -285.3744006158579509, -254.8780723520905838 ) ) ;
#48776 = CIRCLE ( 'NONE', #29193, 9.103929867429224387 ) ;
#48777 = CARTESIAN_POINT ( 'NONE',  ( -43.66626749914844652, -285.9744620146761918, -193.5680395735372201 ) ) ;
#48778 = CARTESIAN_POINT ( 'NONE',  ( -93.58025189592885340, -289.5011897254220230, -323.0019022192084321 ) ) ;
#48779 = CARTESIAN_POINT ( 'NONE',  ( -96.08044335633468336, -299.1784132186828629, -223.1576556985411344 ) ) ;
#48780 = CARTESIAN_POINT ( 'NONE',  ( -20.45871956450569229, -292.8348034763471901, -343.3185278757484866 ) ) ;
#48781 = CARTESIAN_POINT ( 'NONE',  ( 20.01497926838791130, -280.0544944302019985, -219.2104189070933273 ) ) ;
#48782 = CARTESIAN_POINT ( 'NONE',  ( 35.78497577281001440, -284.8380690714490129, -253.7030783399848985 ) ) ;
#48783 = AXIS2_PLACEMENT_3D ( 'NONE', #72458, #21, #22259 ) ;
#48784 = CARTESIAN_POINT ( 'NONE',  ( -10.59362080976867482, -287.4903506443534411, -338.7652451165742491 ) ) ;
#48785 = DIRECTION ( 'NONE',  ( -5.551115123125789802E-15, 0.000000000000000000, 1.000000000000000000 ) ) ;
#48786 = CARTESIAN_POINT ( 'NONE',  ( -64.57010964823807342, -287.4072960800537544, -340.2996576680407657 ) ) ;
#48787 = CARTESIAN_POINT ( 'NONE',  ( -101.3293075261046710, -274.5696475339431686, -233.7031034039917472 ) ) ;
#48788 = CARTESIAN_POINT ( 'NONE',  ( 22.40315372552599271, -282.3344857988484478, -222.7046354972477502 ) ) ;
#48790 = CARTESIAN_POINT ( 'NONE',  ( 33.32351073033067479, -281.7945278179896604, -288.7256019913251635 ) ) ;
#48789 = CARTESIAN_POINT ( 'NONE',  ( -112.1155930067112649, -270.7750857621161913, -259.1340169022741975 ) ) ;
#48791 = CARTESIAN_POINT ( 'NONE',  ( -97.40610338847450578, -296.0730728061060972, -318.5615180661544628 ) ) ;
#48792 = CARTESIAN_POINT ( 'NONE',  ( -35.14096886606251502, -299.6003140158371707, -196.6671976274662370 ) ) ;
#48793 = CARTESIAN_POINT ( 'NONE',  ( 30.20875484378765208, -283.1217076874604572, -237.6543525513209829 ) ) ;
#48794 = CARTESIAN_POINT ( 'NONE',  ( 52.04239232965979767, -298.2568191073556818, -197.1405908929531847 ) ) ;
#48795 = DIRECTION ( 'NONE',  ( -0.000000000000000000, -1.000000000000000000, -0.000000000000000000 ) ) ;
#48796 = CARTESIAN_POINT ( 'NONE',  ( -98.72252273868838301, -287.1110187090874319, -227.8621508393838440 ) ) ;
#48797 = CARTESIAN_POINT ( 'NONE',  ( 175.2296996224750103, 20.00000000000000000, 0.000000000000000000 ) ) ;
#48798 = CARTESIAN_POINT ( 'NONE',  ( -115.3430155898818299, -275.8380690714489560, -288.1317622949166548 ) ) ;
#48799 = CARTESIAN_POINT ( 'NONE',  ( 35.04539715609341499, -275.0770636427558316, -296.2912665264293537 ) ) ;
#48800 = VECTOR ( 'NONE', #70044, 1000.000000000000000 ) ;
#48801 = CARTESIAN_POINT ( 'NONE',  ( -94.81367959793740852, -285.4263216955772009, -316.5079593686362500 ) ) ;
#48802 =( BOUNDED_CURVE ( )  B_SPLINE_CURVE ( 3, ( #9209, #67474, #10615, #17278 ),
 .UNSPECIFIED., .F., .F. ) 
 B_SPLINE_CURVE_WITH_KNOTS ( ( 4, 4 ),
 ( 1.570796326794896558, 2.411864997362828333 ),
 .UNSPECIFIED. ) 
 CURVE ( )  GEOMETRIC_REPRESENTATION_ITEM ( )  RATIONAL_B_SPLINE_CURVE ( ( 1.000000000000000000, 0.9419139527835176384, 0.9419139527835176384, 1.000000000000000000 ) ) 
 REPRESENTATION_ITEM ( '' )  );
#48803 = CARTESIAN_POINT ( 'NONE',  ( 21.48683435282068643, -277.7716642127030582, -314.9216829241832443 ) ) ;
#48804 = CIRCLE ( 'NONE', #18609, 0.9999999999999896749 ) ;
#48805 = CARTESIAN_POINT ( 'NONE',  ( -78.82449837061346898, -285.0247907745338694, -334.5310777917760561 ) ) ;
#48806 = CARTESIAN_POINT ( 'NONE',  ( -91.04238729555980569, -282.6314891182660745, -320.3947736833543445 ) ) ;
#48807 = CARTESIAN_POINT ( 'NONE',  ( 8.340899652445068924, -282.6770541029541732, -210.8134886029699260 ) ) ;
#48808 = CARTESIAN_POINT ( 'NONE',  ( -70.13369836670366908, -273.7986963956612385, -200.6783123985541408 ) ) ;
#48809 = CARTESIAN_POINT ( 'NONE',  ( 31.85435142406308628, -275.8205306064180036, -304.2598640022296763 ) ) ;
#48810 =( BOUNDED_SURFACE ( )  B_SPLINE_SURFACE ( 3, 2, ( 
 ( #359, #43442, #51462 ),
 ( #59052, #29246, #35883 ),
 ( #21676, #22140, #72338 ),
 ( #28782, #1287, #7457 ) ),
 .UNSPECIFIED., .F., .F., .F. ) 
 B_SPLINE_SURFACE_WITH_KNOTS ( ( 4, 4 ),
 ( 3, 3 ),
 ( 0.000000000000000000, 0.0009300155619514785879 ),
 ( 0.000000000000000000, 1.000000000000000000 ),
 .UNSPECIFIED. ) 
 GEOMETRIC_REPRESENTATION_ITEM ( )  RATIONAL_B_SPLINE_SURFACE ( (
 ( 1.000000000000000000, 0.8255171224912171146, 1.000000000000000000),
 ( 1.000000000000000000, 0.8158797882023639536, 1.000000000000000000),
 ( 1.000000000000000000, 0.8010468905540685247, 1.000000000000000000),
 ( 1.000000000000000000, 0.7827533893364954087, 1.000000000000000000) ) ) 
 REPRESENTATION_ITEM ( '' )  SURFACE ( )  );
#48811 = CARTESIAN_POINT ( 'NONE',  ( -69.11009981657500134, -297.3933657055421236, -337.6958654890304956 ) ) ;
#48812 = DIRECTION ( 'NONE',  ( 0.6632250457539263788, -0.000000000000000000, 0.7484200282493129741 ) ) ;
#48813 = EDGE_CURVE ( 'NONE', #8064, #90187, #71642, .T. ) ;
#48814 = DIRECTION ( 'NONE',  ( -1.000000000000000000, 0.000000000000000000, 0.000000000000000000 ) ) ;
#48815 = CARTESIAN_POINT ( 'NONE',  ( -101.2613947813466098, -295.2336151009571950, -229.6846122945249249 ) ) ;
#48816 = CARTESIAN_POINT ( 'NONE',  ( 3.163017461392574337, -275.9992441355225878, -331.1670082773658805 ) ) ;
#48817 = CARTESIAN_POINT ( 'NONE',  ( -71.66782037961642970, -287.3521951186393153, -204.7890851943573693 ) ) ;
#48818 = CARTESIAN_POINT ( 'NONE',  ( 38.13364687008371590, -295.2140308440156673, -281.5940939132642598 ) ) ;
#48819 = CARTESIAN_POINT ( 'NONE',  ( 30.53990758182080967, -294.2955605422340568, -234.7491367700766318 ) ) ;
#48820 = CARTESIAN_POINT ( 'NONE',  ( -112.2024507298690139, -292.5770464885447950, -268.4394741229540955 ) ) ;
#48821 = CARTESIAN_POINT ( 'NONE',  ( -111.9993164492161952, -276.4768869494644150, -276.1971161971118818 ) ) ;
#48822 = CARTESIAN_POINT ( 'NONE',  ( -71.62622501710009715, -281.5157508758462654, -204.2719024443072726 ) ) ;
#48823 = CARTESIAN_POINT ( 'NONE',  ( -45.26790214284979896, -293.2330298569958131, -344.4294100322289296 ) ) ;
#48824 = CARTESIAN_POINT ( 'NONE',  ( -64.78237100356091105, -285.2671086301278365, -340.9960170492306020 ) ) ;
#48825 = CARTESIAN_POINT ( 'NONE',  ( -110.6998422714887624, -283.4654230564982527, -270.8978990543860164 ) ) ;
#48826 = CARTESIAN_POINT ( 'NONE',  ( 169.7661770085315140, 230.6591521943099110, -191.8278467606775450 ) ) ;
#48827 = ORIENTED_EDGE ( 'NONE', *, *, #90014, .T. ) ;
#48828 = CARTESIAN_POINT ( 'NONE',  ( -81.48798803269406221, -285.0990964972142478, -212.1958985561396958 ) ) ;
#48829 = ORIENTED_EDGE ( 'NONE', *, *, #11258, .T. ) ;
#48830 = CARTESIAN_POINT ( 'NONE',  ( 38.56727514591051431, -282.7689826971383127, -281.2844866282564453 ) ) ;
#48831 = CIRCLE ( 'NONE', #8021, 1.000000000000000888 ) ;
#48832 = CARTESIAN_POINT ( 'NONE',  ( -97.26016824723730281, -283.9893914948825113, -222.6349626906605579 ) ) ;
#48833 = CARTESIAN_POINT ( 'NONE',  ( -107.2099568342708267, -279.9025493815156551, -238.4329833986973881 ) ) ;
#48834 = SHAPE_REPRESENTATION_RELATIONSHIP ( 'NONE' , 'NONE' ,  #61554, #75750 ) ;
#48835 = CARTESIAN_POINT ( 'NONE',  ( -23.04960382704055988, -278.3927875219746397, -345.3710959646958258 ) ) ;
#48836 = CARTESIAN_POINT ( 'NONE',  ( -11.55136634270433227, -281.0306925004511527, -197.8609480248495913 ) ) ;
#48837 = CARTESIAN_POINT ( 'NONE',  ( -37.37352853689063181, -300.5519495502701375, -200.3611179825600459 ) ) ;
#48838 = CARTESIAN_POINT ( 'NONE',  ( 190.8961174813688615, 270.6925287644853029, -139.5879506144360676 ) ) ;
#48839 = AXIS2_PLACEMENT_3D ( 'NONE', #47481, #89624, #11514 ) ;
#48840 = CARTESIAN_POINT ( 'NONE',  ( 3.920097784138138142, -276.6089133133280598, -207.8693004201030590 ) ) ;
#48841 = CARTESIAN_POINT ( 'NONE',  ( -64.29435065518906356, -182.4202019385718643, -362.1134662045771506 ) ) ;
#48842 = AXIS2_PLACEMENT_3D ( 'NONE', #54450, #41152, #91361 ) ;
#48843 = CARTESIAN_POINT ( 'NONE',  ( -109.5575993125019210, -276.8167122651744876, -251.4241912110171029 ) ) ;
#48844 = CARTESIAN_POINT ( 'NONE',  ( 37.06501242101278848, -295.1161266534670062, -254.8826641732230769 ) ) ;
#48845 = CARTESIAN_POINT ( 'NONE',  ( -7.954933637996020046, -294.0052857975274492, -337.3098359824493286 ) ) ;
#48846 = CARTESIAN_POINT ( 'NONE',  ( -113.7532073829613211, -289.9417846639206005, -279.7905033142632192 ) ) ;
#48847 = CARTESIAN_POINT ( 'NONE',  ( 188.3531807883583440, 45.29379214021909661, 9.000000000000001776 ) ) ;
#48848=STYLED_ITEM('',(#93738),#28963);
#48850 = CARTESIAN_POINT ( 'NONE',  ( -46.80750696547797673, -284.3299768624214607, -197.1193578559215496 ) ) ;
#48849 = CARTESIAN_POINT ( 'NONE',  ( -64.07715268106635165, -293.9689222698381172, -341.9419944045560555 ) ) ;
#48851 = CARTESIAN_POINT ( 'NONE',  ( -63.25370804099521393, -293.5713874822761795, -200.7950822612816921 ) ) ;
#48852 = CARTESIAN_POINT ( 'NONE',  ( -46.79480603712902820, -284.4099703930809824, -197.2253447062450675 ) ) ;
#48853 = CARTESIAN_POINT ( 'NONE',  ( -108.2324381847122226, -285.6123884490899627, -289.7927781901291269 ) ) ;
#48854 = ORIENTED_EDGE ( 'NONE', *, *, #6237, .T. ) ;
#48855 = CARTESIAN_POINT ( 'NONE',  ( -37.80567232658941634, -292.9877206998336874, -193.5978133120024154 ) ) ;
#48856 = VECTOR ( 'NONE', #87426, 1000.000000000000000 ) ;
#48857 = CARTESIAN_POINT ( 'NONE',  ( 3.429756406300124016, -282.9802314699958856, -331.0496782240537073 ) ) ;
#48858 = CARTESIAN_POINT ( 'NONE',  ( -88.35251561539841703, -294.5428128083704564, -327.5803626996567459 ) ) ;
#48859 = CARTESIAN_POINT ( 'NONE',  ( -109.7100097668032674, -291.0265331231349819, -296.3448835064751847 ) ) ;
#48860 = CARTESIAN_POINT ( 'NONE',  ( -80.50090365319508123, -290.1121457277528179, -334.1185680935244591 ) ) ;
#48861 = CARTESIAN_POINT ( 'NONE',  ( 35.55250553501682731, -287.6558229110160028, -265.5845879727958732 ) ) ;
#48862 = ORIENTED_EDGE ( 'NONE', *, *, #5103, .T. ) ;
#48863 = CARTESIAN_POINT ( 'NONE',  ( 175.2296996224750103, 20.00000000000000000, 0.000000000000000000 ) ) ;
#48864 = CARTESIAN_POINT ( 'NONE',  ( -111.3927971968902142, -298.2089040087636249, -286.3842421237368967 ) ) ;
#48865 = AXIS2_PLACEMENT_3D ( 'NONE', #79871, #58577, #72767 ) ;
#48866 = CARTESIAN_POINT ( 'NONE',  ( -9.318050067021886207, -297.0809218362947490, -193.8603748128029736 ) ) ;
#48867 = CARTESIAN_POINT ( 'NONE',  ( -76.93903086589591567, -278.5665362596325281, -208.6933674503681289 ) ) ;
#48868 = ORIENTED_EDGE ( 'NONE', *, *, #53950, .T. ) ;
#48869 = CARTESIAN_POINT ( 'NONE',  ( 36.82462404239806375, -275.3169603148791680, -290.8768648620383601 ) ) ;
#48870 = CARTESIAN_POINT ( 'NONE',  ( -94.13562889880033424, -295.6916931295959898, -223.3823892766719723 ) ) ;
#48871 = CARTESIAN_POINT ( 'NONE',  ( 26.25761974421145339, -277.8256077703858296, -308.2174321690018814 ) ) ;
#48872 = CARTESIAN_POINT ( 'NONE',  ( -13.64916646131800526, -272.5025748830576617, -200.0082265890458473 ) ) ;
#48873 = CARTESIAN_POINT ( 'NONE',  ( -38.33234156308011364, -296.2699215360458425, -343.7515065605587665 ) ) ;
#48874 = CARTESIAN_POINT ( 'NONE',  ( -20.76496692736728633, -295.9141398178044255, -341.8237951098844860 ) ) ;
#48875 = CARTESIAN_POINT ( 'NONE',  ( 85.55100297371609486, -298.0521521680024080, -525.1711561948568487 ) ) ;
#48876 = CARTESIAN_POINT ( 'NONE',  ( -58.60830574555028960, -296.9226618092444596, -343.5883154043546597 ) ) ;
#48877 = AXIS2_PLACEMENT_3D ( 'NONE', #79069, #57307, #50655 ) ;
#48878 = CARTESIAN_POINT ( 'NONE',  ( -36.88444583258380760, -296.0577074479207909, -195.1945980807678325 ) ) ;
#48879 = CARTESIAN_POINT ( 'NONE',  ( -52.39885591807911425, -292.5057482764098040, -198.7747129985252741 ) ) ;
#48880 = CARTESIAN_POINT ( 'NONE',  ( -68.78735336093448893, -274.4520380518480920, -200.2373395437965939 ) ) ;
#48881 = CARTESIAN_POINT ( 'NONE',  ( -105.6668342468205140, -288.7623754021108198, -297.8301995730903400 ) ) ;
#48882 = CARTESIAN_POINT ( 'NONE',  ( 165.2494399300530290, -11.64849832608277325, 10.00000000000000000 ) ) ;
#48883 = CARTESIAN_POINT ( 'NONE',  ( -110.9800606624915815, -273.3265990528932434, -247.8872775669179589 ) ) ;
#48884 = EDGE_CURVE ( 'NONE', #65856, #49322, #79208, .T. ) ;
#48885 = CARTESIAN_POINT ( 'NONE',  ( -107.9889556372695552, -296.6410895767857028, -288.8781580677458578 ) ) ;
#48886 = EDGE_CURVE ( 'NONE', #46489, #78077, #51217, .T. ) ;
#48887 = CARTESIAN_POINT ( 'NONE',  ( -50.67392717452807460, -281.8625606862206610, -196.1946934897722770 ) ) ;
#48888 = CARTESIAN_POINT ( 'NONE',  ( 38.92147502931899083, -280.1601826203132077, -264.2597749594601169 ) ) ;
#48889 = CARTESIAN_POINT ( 'NONE',  ( -11.90773598810970846, -276.0783133199085455, -342.9871152434971009 ) ) ;
#48890 = CARTESIAN_POINT ( 'NONE',  ( 38.84169934355085019, -279.9109634800678350, -267.1120261466754755 ) ) ;
#48891 = CARTESIAN_POINT ( 'NONE',  ( 32.86582971841230716, -279.9002235044725353, -297.2112795726115451 ) ) ;
#48892 = CARTESIAN_POINT ( 'NONE',  ( -74.55581212949162762, -272.1217423160327940, -206.8159976636424062 ) ) ;
#48893 = CARTESIAN_POINT ( 'NONE',  ( -18.58858278732690295, -278.8109108328932848, -343.0316977440042479 ) ) ;
#48894 = CARTESIAN_POINT ( 'NONE',  ( 191.4749582765727212, -21.37379927922774314, 13.00000000000000178 ) ) ;
#48895 = DIRECTION ( 'NONE',  ( 0.000000000000000000, 1.000000000000000000, 0.000000000000000000 ) ) ;
#48896 = CARTESIAN_POINT ( 'NONE',  ( -31.97581412555593161, -296.3583192041082839, -194.3760267278788092 ) ) ;
#48897 = CARTESIAN_POINT ( 'NONE',  ( -13.86645436775929596, -292.3484273333282886, -196.9708888462583900 ) ) ;
#48898 = CARTESIAN_POINT ( 'NONE',  ( 35.46937008295187610, -277.7916533625960369, -289.0313211020973085 ) ) ;
#48899 = CARTESIAN_POINT ( 'NONE',  ( -72.83225659644364214, -271.5822585212394529, -204.2319261592077737 ) ) ;
#48900 = CARTESIAN_POINT ( 'NONE',  ( 186.6539576904058890, 276.0000000000000568, -11.60392986742922439 ) ) ;
#48901 = CARTESIAN_POINT ( 'NONE',  ( 27.09011957082900324, -283.9989411684799734, -309.9299922774285960 ) ) ;
#48902 = CARTESIAN_POINT ( 'NONE',  ( 158.6539576904058606, 293.9636489450775230, 11.60392986742922439 ) ) ;
#48903 = CARTESIAN_POINT ( 'NONE',  ( -5.239512184654298466, -284.4743694816795596, -202.5648510644412568 ) ) ;
#48904 = LINE ( 'NONE', #48424, #7427 ) ;
#48905 = CARTESIAN_POINT ( 'NONE',  ( -5.382408334676391348, -293.4169320221702151, -336.4487045733047239 ) ) ;
#48906 = CARTESIAN_POINT ( 'NONE',  ( 15.93214297801810098, -284.9567541479334523, -218.6623450708501082 ) ) ;
#48907 = CARTESIAN_POINT ( 'NONE',  ( 157.4642333713238429, 15.57755555264425240, -7.027845929950948367 ) ) ;
#48908 = CARTESIAN_POINT ( 'NONE',  ( 20.35582022997981611, -292.2135310197681974, -318.2776787626873443 ) ) ;
#48909 = CARTESIAN_POINT ( 'NONE',  ( -69.48300058784650446, -284.1167174138755627, -201.1396252506790745 ) ) ;
#48910 = CARTESIAN_POINT ( 'NONE',  ( -38.38542137872376969, -281.6389881503830566, -196.5559589294611840 ) ) ;
#48911 = CARTESIAN_POINT ( 'NONE',  ( -23.87089300761373423, -287.4255132498776106, -194.8979917461260811 ) ) ;
#48912 = CARTESIAN_POINT ( 'NONE',  ( 20.31208404138603285, -279.1148563649746848, -220.8436973572415525 ) ) ;
#48913 = CARTESIAN_POINT ( 'NONE',  ( 27.65814003892320017, -287.0993824648368218, -237.0228571196263658 ) ) ;
#48914 = VECTOR ( 'NONE', #24422, 1000.000000000000000 ) ;
#48915 = CARTESIAN_POINT ( 'NONE',  ( -66.31829895787133466, -281.0904749840060504, -202.7032126429618586 ) ) ;
#48916 = CARTESIAN_POINT ( 'NONE',  ( 17.17633097946117715, -281.6584852969534154, -221.5719182415239459 ) ) ;
#48917 = CARTESIAN_POINT ( 'NONE',  ( -67.85827863381908287, -287.6335187730401799, -201.4475162250844278 ) ) ;
#48918 =( GEOMETRIC_REPRESENTATION_CONTEXT ( 3 ) GLOBAL_UNCERTAINTY_ASSIGNED_CONTEXT ( ( #86909 ) ) GLOBAL_UNIT_ASSIGNED_CONTEXT ( ( #60100, #52041, #68118 ) ) REPRESENTATION_CONTEXT ( 'NONE', 'WORKASPACE' ) );
#48919 = ORIENTED_EDGE ( 'NONE', *, *, #8888, .T. ) ;
#48920 = VECTOR ( 'NONE', #48160, 1000.000000000000000 ) ;
#48921 = CARTESIAN_POINT ( 'NONE',  ( -98.23266610948735433, -297.0149026693531482, -223.2092732495960945 ) ) ;
#48922 = CARTESIAN_POINT ( 'NONE',  ( -92.91419131404576603, -293.2296722294915412, -220.5068134914450297 ) ) ;
#48923 = CARTESIAN_POINT ( 'NONE',  ( 209.8744251295252354, 28.03846817292548366, 12.00000000000000000 ) ) ;
#48924 = CARTESIAN_POINT ( 'NONE',  ( -72.08107566293803359, -300.1233781216987495, -198.2974183793908196 ) ) ;
#48925 = VERTEX_POINT ( 'NONE', #80116 ) ;
#48926 = CARTESIAN_POINT ( 'NONE',  ( -80.18403987036899139, -271.4738533065243473, -208.5359152840082402 ) ) ;
#48927 = DIRECTION ( 'NONE',  ( -0.000000000000000000, -0.000000000000000000, -1.000000000000000000 ) ) ;
#48928 = CARTESIAN_POINT ( 'NONE',  ( -105.2540632708972765, -294.5010128878602700, -305.0368010975247444 ) ) ;
#48929 = CARTESIAN_POINT ( 'NONE',  ( -60.52949302720537617, -297.2509154886362239, -201.0233020330287559 ) ) ;
#48930 = AXIS2_PLACEMENT_3D ( 'NONE', #63734, #58013, #72220 ) ;
#48931 = CARTESIAN_POINT ( 'NONE',  ( 4.019609066241355499, -290.0042790554126668, -331.4140517803542139 ) ) ;
#48932 = CARTESIAN_POINT ( 'NONE',  ( 22.92578535756121383, -282.7203185387714370, -227.3982944264695618 ) ) ;
#48933 = CARTESIAN_POINT ( 'NONE',  ( -112.0799808880328925, -291.6614590135502567, -286.7161680874208400 ) ) ;
#48934 = CARTESIAN_POINT ( 'NONE',  ( 10.28133781032519956, -288.7094029330172020, -212.4210894774008409 ) ) ;
#48935 = CARTESIAN_POINT ( 'NONE',  ( -31.07587571008332716, -280.2957936943342929, -193.5637893441634958 ) ) ;
#48936 = CARTESIAN_POINT ( 'NONE',  ( -37.70702677364511857, -293.1365090615122995, -345.9330722352666498 ) ) ;
#48937 = CARTESIAN_POINT ( 'NONE',  ( 39.64073502675631744, -281.3441811152776495, -267.0594941863539020 ) ) ;
#48938 = VECTOR ( 'NONE', #34123, 1000.000000000000000 ) ;
#48939 = CARTESIAN_POINT ( 'NONE',  ( 20.80852366203457748, -276.7717962356991848, -224.1951808642405126 ) ) ;
#48940 = CARTESIAN_POINT ( 'NONE',  ( -21.39648532958013050, -276.7662352645559167, -200.3538533559491555 ) ) ;
#48941 = CARTESIAN_POINT ( 'NONE',  ( 36.25166463110930692, -274.0319597747138687, -289.2817596117944277 ) ) ;
#48942 = CARTESIAN_POINT ( 'NONE',  ( 73.43068321062709458, -134.2641364535880939, -4.999999999999990230 ) ) ;
#48943 = CARTESIAN_POINT ( 'NONE',  ( 31.13017105736646783, -280.7184194820921448, -244.7288588045542781 ) ) ;
#48944 = CIRCLE ( 'NONE', #85244, 4.500000000000003553 ) ;
#48945 = CARTESIAN_POINT ( 'NONE',  ( -59.53523291736747325, -278.5384208520371203, -343.6786180763897391 ) ) ;
#48946 = CARTESIAN_POINT ( 'NONE',  ( -83.51331696775213231, -274.7186064872564089, -213.1822296148037879 ) ) ;
#48947 = CARTESIAN_POINT ( 'NONE',  ( -110.6976144103448121, -283.8978999627197481, -247.5608459168789182 ) ) ;
#48948 = CARTESIAN_POINT ( 'NONE',  ( -94.23293937510810281, -292.9749340288964277, -222.9983115447663522 ) ) ;
#48949 = CARTESIAN_POINT ( 'NONE',  ( -94.50002868054474447, -274.8417268522022141, -219.9689966385420519 ) ) ;
#48950 = CARTESIAN_POINT ( 'NONE',  ( -112.5863935297308700, -274.0450845658967296, -256.2383464419285701 ) ) ;
#48951 = FACE_OUTER_BOUND ( 'NONE', #83487, .T. ) ;
#48952 = CARTESIAN_POINT ( 'NONE',  ( 19.18024537832320675, -276.0398022582805311, -316.5789716663322793 ) ) ;
#48953 = CARTESIAN_POINT ( 'NONE',  ( -89.76852189558813677, -297.7936146566669890, -323.8329496689507323 ) ) ;
#48954 = CARTESIAN_POINT ( 'NONE',  ( -86.92223003320941643, -283.3605800723489097, -214.2401237080880492 ) ) ;
#48955 = CARTESIAN_POINT ( 'NONE',  ( -42.04842835355492525, -291.6610673955120205, -193.5262886344245601 ) ) ;
#48956 = CARTESIAN_POINT ( 'NONE',  ( 25.35245526591383580, -274.1218991087860104, -310.9692089050035975 ) ) ;
#48957 = CARTESIAN_POINT ( 'NONE',  ( 38.90232380747248442, -289.1669077958005687, -271.5185865521456776 ) ) ;
#48958 = VECTOR ( 'NONE', #18896, 1000.000000000000000 ) ;
#48959 = CARTESIAN_POINT ( 'NONE',  ( -49.72747728650247723, -290.8109238110834553, -198.0543438882310170 ) ) ;
#48960 = ORIENTED_EDGE ( 'NONE', *, *, #78765, .F. ) ;
#48961 = CARTESIAN_POINT ( 'NONE',  ( 21.76509671230398979, -291.4716276612833212, -221.9359916285157794 ) ) ;
#48962 = ORIENTED_EDGE ( 'NONE', *, *, #70919, .F. ) ;
#48963 = CARTESIAN_POINT ( 'NONE',  ( -104.0687647103991225, -289.8182357120257961, -300.1438274952589040 ) ) ;
#48964 = EDGE_LOOP ( 'NONE', ( #19956, #91595, #64152, #84029, #5399, #63171, #61692, #78667, #78545, #38812, #46043, #54674, #45052, #85068, #62755, #78586, #56784, #57147, #69490 ) ) ;
#48965 = CARTESIAN_POINT ( 'NONE',  ( 14.02958246012962995, -287.8326412374968299, -213.3470710461920703 ) ) ;
#48966 = CARTESIAN_POINT ( 'NONE',  ( -109.5123143934463741, -278.7388836678495068, -281.4737199890546435 ) ) ;
#48967 = CARTESIAN_POINT ( 'NONE',  ( 10.99279277905546515, -293.3218042508020744, -329.9717075471970134 ) ) ;
#48968 = CARTESIAN_POINT ( 'NONE',  ( -33.74041141479603567, -286.7477657199906389, -193.5474245002785381 ) ) ;
#48969 = CARTESIAN_POINT ( 'NONE',  ( -110.9070844177439454, -285.1722274901824221, -247.5127842735608397 ) ) ;
#48970 = CARTESIAN_POINT ( 'NONE',  ( 33.67170838645847653, -282.1104001074387497, -287.4197168481941844 ) ) ;
#48971 = CARTESIAN_POINT ( 'NONE',  ( -71.22237285446017552, -196.1705862519446839, -360.4586094979653126 ) ) ;
#48972 = CARTESIAN_POINT ( 'NONE',  ( 24.11042299814977952, -22.50654057154123677, -344.0834433819322840 ) ) ;
#48973 = CARTESIAN_POINT ( 'NONE',  ( 172.5076325409972640, 241.1453524790508709, -177.1370813373998203 ) ) ;
#48974 = CIRCLE ( 'NONE', #12696, 0.4999999999999979461 ) ;
#48975 = CARTESIAN_POINT ( 'NONE',  ( 26.90366985021008261, -275.2273247194847272, -305.4689148819937827 ) ) ;
#48976 = CARTESIAN_POINT ( 'NONE',  ( 26.91406211954589978, -273.9912076777142147, -234.9647298189462674 ) ) ;
#48977 = CARTESIAN_POINT ( 'NONE',  ( -36.53512604192584945, -297.5696527736715211, -193.4227212417192732 ) ) ;
#48978 = CARTESIAN_POINT ( 'NONE',  ( -106.9971877404514089, -265.1276182340686205, -305.5655013973570817 ) ) ;
#48979 = CARTESIAN_POINT ( 'NONE',  ( 32.56234815641699498, -274.6363849193725173, -301.4532762367821874 ) ) ;
#48980 = CARTESIAN_POINT ( 'NONE',  ( -60.93047101697215595, -299.6032995918266693, -199.9189876645664299 ) ) ;
#48981 = CARTESIAN_POINT ( 'NONE',  ( -86.14501698932035367, -292.4363451673487475, -215.5893768787423994 ) ) ;
#48982 = ORIENTED_EDGE ( 'NONE', *, *, #7422, .F. ) ;
#48983 = CARTESIAN_POINT ( 'NONE',  ( -60.08983448113527714, -298.7057179334694865, -196.9890344714140156 ) ) ;
#48984 = CARTESIAN_POINT ( 'NONE',  ( -15.82754909324679282, -289.2586977555125145, -340.2361187236685396 ) ) ;
#48985 = CARTESIAN_POINT ( 'NONE',  ( -114.2044050404693252, -297.3284836599280538, -272.4755725938329078 ) ) ;
#48986 = CARTESIAN_POINT ( 'NONE',  ( -33.43168903299599748, -295.4965446677736054, -347.2132710480843798 ) ) ;
#48987 = CARTESIAN_POINT ( 'NONE',  ( 35.53452752329296516, -293.6522563999161548, -265.3142274651738717 ) ) ;
#48988 = ORIENTED_EDGE ( 'NONE', *, *, #3347, .F. ) ;
#48989 = CARTESIAN_POINT ( 'NONE',  ( 38.18523616417426325, -277.5180562508114690, -273.9507054344690005 ) ) ;
#48990 = ORIENTED_EDGE ( 'NONE', *, *, #5970, .T. ) ;
#48991 = CARTESIAN_POINT ( 'NONE',  ( -2.412472829965490728, -280.0093825389647577, -201.7936774572754928 ) ) ;
#48992 = EDGE_CURVE ( 'NONE', #11198, #13924, #73928, .T. ) ;
#48993 = CIRCLE ( 'NONE', #73201, 7.500000000000012434 ) ;
#48994 = CARTESIAN_POINT ( 'NONE',  ( -91.13255127911651243, -278.7812074471644337, -320.1334881098632081 ) ) ;
#48995 = CARTESIAN_POINT ( 'NONE',  ( 34.76120917754666095, -277.0044672212106320, -246.2132351918195070 ) ) ;
#48996 = CARTESIAN_POINT ( 'NONE',  ( -51.03892439605401421, -275.2464802822533443, -344.4610022425868010 ) ) ;
#48997 = CARTESIAN_POINT ( 'NONE',  ( -47.29482503177550967, -298.5738962064230577, -197.8886506911530603 ) ) ;
#48998 = CARTESIAN_POINT ( 'NONE',  ( -108.5442712301038739, -294.8828204433801830, -289.0004685252769150 ) ) ;
#48999 = CARTESIAN_POINT ( 'NONE',  ( 186.6539576904058890, 293.9636489450775230, 11.60392986742922439 ) ) ;
#49000 = CARTESIAN_POINT ( 'NONE',  ( -72.48430026534484227, -280.0919815571037361, -201.9028911782505986 ) ) ;
#49001 = EDGE_CURVE ( 'NONE', #59807, #75996, #46671, .T. ) ;
#49002 = CARTESIAN_POINT ( 'NONE',  ( 19.18294190099698326, -276.3731083802287571, -316.5756738829676351 ) ) ;
#49003 = VECTOR ( 'NONE', #71520, 1000.000000000000000 ) ;
#49004 = CARTESIAN_POINT ( 'NONE',  ( 34.39766258241920127, -285.8987117250308074, -243.7761201490658891 ) ) ;
#49005 = CARTESIAN_POINT ( 'NONE',  ( -9.970657782087727128, -300.3941834529350103, -195.1851368233604092 ) ) ;
#49006 = DIRECTION ( 'NONE',  ( 0.000000000000000000, 1.000000000000000000, 0.000000000000000000 ) ) ;
#49007 = AXIS2_PLACEMENT_3D ( 'NONE', #56861, #13293, #473 ) ;
#49008 = CARTESIAN_POINT ( 'NONE',  ( 35.11888246362659061, -286.8834932232098254, -280.5549972923389532 ) ) ;
#49009 = CIRCLE ( 'NONE', #20296, 25.00000000000000355 ) ;
#49010 = CARTESIAN_POINT ( 'NONE',  ( -68.93579284816676989, -277.8707398123788721, -203.4299046234843615 ) ) ;
#49012 = CARTESIAN_POINT ( 'NONE',  ( -93.66437921015022994, -281.9517676457292055, -319.0536172771480210 ) ) ;
#49011 = CARTESIAN_POINT ( 'NONE',  ( -91.72008948157430552, -277.8322080479310330, -220.7792090945039831 ) ) ;
#49013 = CARTESIAN_POINT ( 'NONE',  ( 27.73743617622592339, -289.0538613437115600, -232.9797186796481583 ) ) ;
#49014 = CARTESIAN_POINT ( 'NONE',  ( 27.12280758407763770, -277.2349098643475713, -305.5595377799446624 ) ) ;
#49015 = CARTESIAN_POINT ( 'NONE',  ( 197.2116943569230330, 275.5000000000000568, -12.42446933126074882 ) ) ;
#49016 = CARTESIAN_POINT ( 'NONE',  ( -94.16280059709950478, -293.2310980993468661, -221.3888169776338373 ) ) ;
#49018 = CARTESIAN_POINT ( 'NONE',  ( -69.88761212159255365, -275.7146826772521990, -339.0393140790539519 ) ) ;
#49017 = VECTOR ( 'NONE', #53544, 1000.000000000000000 ) ;
#49019 = CARTESIAN_POINT ( 'NONE',  ( -16.34366499675604700, -277.4250170473829940, -340.4354509730983978 ) ) ;
#49020 = CARTESIAN_POINT ( 'NONE',  ( 37.45652204134463403, -283.6540100234881834, -278.2989887279164805 ) ) ;
#49021 = DIRECTION ( 'NONE',  ( 0.000000000000000000, 0.000000000000000000, 1.000000000000000000 ) ) ;
#49022 = CARTESIAN_POINT ( 'NONE',  ( 2.443119307038749355, -290.4439577755627511, -334.6602095165745254 ) ) ;
#49023 = CARTESIAN_POINT ( 'NONE',  ( -110.6984052826173297, -294.7532517441525215, -254.6867332384633471 ) ) ;
#49024 = AXIS2_PLACEMENT_3D ( 'NONE', #11437, #85277, #76774 ) ;
#49025 = DIRECTION ( 'NONE',  ( 1.110223024625152438E-14, 0.000000000000000000, 1.000000000000000000 ) ) ;
#49026 = CARTESIAN_POINT ( 'NONE',  ( 27.07680156465469423, -273.7557429711135910, -234.8784612666853491 ) ) ;
#49027 = CARTESIAN_POINT ( 'NONE',  ( 21.17088218009146416, -291.0583096145643367, -224.6552685211873666 ) ) ;
#49028 = CARTESIAN_POINT ( 'NONE',  ( 195.4695817506115532, 39.54252710742871812, 15.00000000000000355 ) ) ;
#49029 = DIRECTION ( 'NONE',  ( -0.000000000000000000, 1.000000000000000000, -0.000000000000000000 ) ) ;
#49030 = CARTESIAN_POINT ( 'NONE',  ( -111.6377407753095525, -289.2516488475491201, -252.9597933251780262 ) ) ;
#49031 = CARTESIAN_POINT ( 'NONE',  ( 38.34747920006685007, -285.6996990605342717, -263.0769924213881836 ) ) ;
#49032 = CARTESIAN_POINT ( 'NONE',  ( -96.24842740309239275, -286.5915563871333802, -226.2547420232250204 ) ) ;
#49033 = CARTESIAN_POINT ( 'NONE',  ( -14.52533024915295812, -287.1583125684668971, -200.7952885247583481 ) ) ;
#49034 = CARTESIAN_POINT ( 'NONE',  ( -28.07686869166656507, -294.1489522567524091, -195.5251062565476161 ) ) ;
#49035 = CARTESIAN_POINT ( 'NONE',  ( 36.49322979734465378, -273.8373710457436800, -286.4750576180215944 ) ) ;
#49036 = CARTESIAN_POINT ( 'NONE',  ( 37.21932293740722031, -276.1250436357899503, -289.5026469455282268 ) ) ;
#49037 = CARTESIAN_POINT ( 'NONE',  ( -112.6788521215020893, -288.5498593662401845, -276.8059660775163593 ) ) ;
#49038 = CARTESIAN_POINT ( 'NONE',  ( -38.54495906529282223, -277.0668494516912688, -347.3517159015918310 ) ) ;
#49039 = CARTESIAN_POINT ( 'NONE',  ( -87.57875334261140665, -297.7375328000662762, -325.5705853282494786 ) ) ;
#49040 = DIRECTION ( 'NONE',  ( -0.000000000000000000, 1.000000000000000000, 0.000000000000000000 ) ) ;
#49041 = CARTESIAN_POINT ( 'NONE',  ( 104.1717476309105166, -299.5541904835127980, -195.3611179825600175 ) ) ;
#49042 = CARTESIAN_POINT ( 'NONE',  ( -110.3647210718829257, -283.1224591420339607, -279.1004827411406382 ) ) ;
#49043 = CARTESIAN_POINT ( 'NONE',  ( -35.36259463782438672, -278.0768060983852479, -195.3744352578095231 ) ) ;
#49044 = CARTESIAN_POINT ( 'NONE',  ( -57.23711263161519724, -285.8906705383787994, 52.50000000000000711 ) ) ;
#49045 = CARTESIAN_POINT ( 'NONE',  ( -24.25926044836468876, -272.6960145150854373, -195.1305954621356591 ) ) ;
#49046 = CARTESIAN_POINT ( 'NONE',  ( -107.2165108551313892, -277.6145896345292385, -292.0109915301164847 ) ) ;
#49047 = CARTESIAN_POINT ( 'NONE',  ( 34.74984846340299782, -295.2727566628387308, -285.7029626960218707 ) ) ;
#49048 = CARTESIAN_POINT ( 'NONE',  ( 8.373349113323561355, -279.5815387699674375, -208.7189098049069855 ) ) ;
#49049 = CARTESIAN_POINT ( 'NONE',  ( -28.85685618759001514, -295.8833435298444101, -343.1544157019758359 ) ) ;
#49050 = CARTESIAN_POINT ( 'NONE',  ( -104.1639674885520606, -297.3799489035009174, -307.7263616356498801 ) ) ;
#49051 = CARTESIAN_POINT ( 'NONE',  ( -55.29160844359187621, -297.6481932416154450, -199.5500571444789273 ) ) ;
#49052 = CARTESIAN_POINT ( 'NONE',  ( -68.65891597376128175, -293.6407473882142085, -202.1983976820689008 ) ) ;
#49053 = CARTESIAN_POINT ( 'NONE',  ( -52.17536325414393872, -286.0341051792089502, -194.7490513125552809 ) ) ;
#49054 = CARTESIAN_POINT ( 'NONE',  ( 22.66923194685100640, -273.0642493935716857, -224.0907385376136176 ) ) ;
#49055 = CARTESIAN_POINT ( 'NONE',  ( 19.62281679186269301, -288.0897526907239694, -322.1885150379844731 ) ) ;
#49056 = CARTESIAN_POINT ( 'NONE',  ( -66.74020650577232061, -281.6450052654294609, -201.7354018456952645 ) ) ;
#49057 = CARTESIAN_POINT ( 'NONE',  ( -4.478264524893772247, -285.5550389460045153, -204.9134056527796872 ) ) ;
#49058 = CARTESIAN_POINT ( 'NONE',  ( -95.74903386913437942, -287.9043026848621594, -317.4301200119467126 ) ) ;
#49059 = CARTESIAN_POINT ( 'NONE',  ( -84.42323508662160236, -232.9070939334762329, -346.4289530206739300 ) ) ;
#49060 = CARTESIAN_POINT ( 'NONE',  ( 22.04526140838169113, -286.4644555410820885, -227.7178849848838240 ) ) ;
#49061 = CARTESIAN_POINT ( 'NONE',  ( 202.9738562182569694, 293.9636489450776367, -44.00000000000000000 ) ) ;
#49062 = CARTESIAN_POINT ( 'NONE',  ( 25.74382143705825499, -283.0732098265501691, -314.1225217863477042 ) ) ;
#49063 = CARTESIAN_POINT ( 'NONE',  ( -113.9522589089158799, -289.6718988075677430, -265.4987630313674458 ) ) ;
#49064 = CARTESIAN_POINT ( 'NONE',  ( -92.50879621959956012, -280.8791148359696876, -217.7211551997537242 ) ) ;
#49065 = CARTESIAN_POINT ( 'NONE',  ( -72.29653378419736498, -280.9146753078727556, -202.2917439333185428 ) ) ;
#49066 = CARTESIAN_POINT ( 'NONE',  ( 19.35069529618707662, -282.0363800091801068, -316.3696488228370072 ) ) ;
#49067 = CARTESIAN_POINT ( 'NONE',  ( 35.18251157533608620, -277.7979341069139423, -289.4723546865220669 ) ) ;
#49068 = CARTESIAN_POINT ( 'NONE',  ( -5.797701210098003877, -294.6487355951004474, -340.6033854022714991 ) ) ;
#49069 = CARTESIAN_POINT ( 'NONE',  ( -101.7353558642199829, -288.0641249232600671, -308.2161762152076676 ) ) ;
#49070 = CARTESIAN_POINT ( 'NONE',  ( -94.19094351354441130, -294.8198855719933249, -316.6668060364984285 ) ) ;
#49071 = ORIENTED_EDGE ( 'NONE', *, *, #73107, .T. ) ;
#49072 = CARTESIAN_POINT ( 'NONE',  ( -69.61171599948387723, -285.4004398315260005, -337.4569337373252438 ) ) ;
#49073 = CARTESIAN_POINT ( 'NONE',  ( -73.31651649521867853, -295.2101576183756606, -333.9055911816712978 ) ) ;
#49074 = CARTESIAN_POINT ( 'NONE',  ( -7.323915927691939665, -293.5163528241192239, -199.7747278483543880 ) ) ;
#49075 = CIRCLE ( 'NONE', #33941, 25.00000000000000355 ) ;
#49076 = CARTESIAN_POINT ( 'NONE',  ( -40.23009277398153216, -283.7408306292705333, -343.4059662359040317 ) ) ;
#49077 = CARTESIAN_POINT ( 'NONE',  ( -35.51732685292294178, -273.1332410854584509, -193.6050031194094743 ) ) ;
#49078 = CARTESIAN_POINT ( 'NONE',  ( -40.63636649869368966, -292.6631778737889249, -193.5204975093755024 ) ) ;
#49079 = CARTESIAN_POINT ( 'NONE',  ( -80.21933912314375448, -283.6183068140346109, -207.8333060438608868 ) ) ;
#49080 = CARTESIAN_POINT ( 'NONE',  ( -104.5935665005996924, -291.3711356347590140, -232.9054006504900940 ) ) ;
#49081 = CARTESIAN_POINT ( 'NONE',  ( -5.779451788039407845, -288.9585810550704537, -336.2087600557789528 ) ) ;
#49082 = B_SPLINE_CURVE_WITH_KNOTS ( 'NONE', 3,
 ( #11987, #68833, #3961, #54599, #40370, #40836 ),
 .UNSPECIFIED., .F., .F.,
 ( 4, 2, 4 ),
 ( 0.000000000000000000, 0.001526582415388715898, 0.003053164830777431796 ),
 .UNSPECIFIED. ) ;
#49083 = DIRECTION ( 'NONE',  ( -0.000000000000000000, 1.000000000000000000, -0.000000000000000000 ) ) ;
#49084 = DIRECTION ( 'NONE',  ( 0.000000000000000000, 0.000000000000000000, 1.000000000000000000 ) ) ;
#49085 = CARTESIAN_POINT ( 'NONE',  ( 102.9770308486741328, 114.5320353338112795, -279.4838030456201068 ) ) ;
#49086 = CARTESIAN_POINT ( 'NONE',  ( 15.28944551476376645, -283.8448576489772677, -325.6120931757356516 ) ) ;
#49087 = CARTESIAN_POINT ( 'NONE',  ( -54.42813229853333468, -289.3380690714489560, -195.3538533559490702 ) ) ;
#49088 = ORIENTED_EDGE ( 'NONE', *, *, #50431, .T. ) ;
#49089 = CARTESIAN_POINT ( 'NONE',  ( 22.05434560458958870, -281.0713194943489270, -313.3516161058334433 ) ) ;
#49090 = CARTESIAN_POINT ( 'NONE',  ( -45.65155453694142551, -276.8213249183204994, -346.9431800961029921 ) ) ;
#49091 = CARTESIAN_POINT ( 'NONE',  ( -90.36735601340649282, -279.8044037143159812, -323.2391095640879826 ) ) ;
#49092 = CARTESIAN_POINT ( 'NONE',  ( 140.4625507534157975, 178.1663472580048335, -239.4196196848511420 ) ) ;
#49093 = CARTESIAN_POINT ( 'NONE',  ( 14.77283351634792119, -279.3435719254887317, -214.4078117668306618 ) ) ;
#49094 = CARTESIAN_POINT ( 'NONE',  ( -65.69514492888039570, -283.6997393491515709, -201.2559156838794365 ) ) ;
#49095 = CARTESIAN_POINT ( 'NONE',  ( -111.6148598902819060, -298.5163616957030968, -254.2543746898427912 ) ) ;
#49096 = CIRCLE ( 'NONE', #23409, 204.9779373800640485 ) ;
#49097 = CARTESIAN_POINT ( 'NONE',  ( 31.85729972201680482, -293.7314282135134249, -246.7625333284971418 ) ) ;
#49098 = VERTEX_POINT ( 'NONE', #50303 ) ;
#49099 = CARTESIAN_POINT ( 'NONE',  ( -109.4256946558087549, -289.0484576283844262, -284.7483117707091083 ) ) ;
#49100 = CARTESIAN_POINT ( 'NONE',  ( 39.60548046197511951, -276.2135972914053355, -271.1622903833703617 ) ) ;
#49101 = CARTESIAN_POINT ( 'NONE',  ( -97.84319116648059378, -273.1209974988395288, -229.4228094201411352 ) ) ;
#49102 = EDGE_LOOP ( 'NONE', ( #72637, #48962, #56713, #87066 ) ) ;
#49103 = CARTESIAN_POINT ( 'NONE',  ( 120.8395553409046528, -299.5541904835127980, -192.4214616598467273 ) ) ;
#49104 = CARTESIAN_POINT ( 'NONE',  ( 196.8803347170859865, 42.36571313990103249, 12.49999999999999289 ) ) ;
#49105 = EDGE_CURVE ( 'NONE', #23354, #28813, #93392, .T. ) ;
#49106 = CARTESIAN_POINT ( 'NONE',  ( 154.7156223832783724, 20.48904911123736028, 12.57712157663156560 ) ) ;
#49107 = CARTESIAN_POINT ( 'NONE',  ( 35.44840891232407643, -282.7516556034379960, -279.4831145160931669 ) ) ;
#49108 = CARTESIAN_POINT ( 'NONE',  ( -69.55347985637641273, -281.3941751992882701, -201.5255879351402655 ) ) ;
#49109 = CARTESIAN_POINT ( 'NONE',  ( -48.37592472953704004, -282.2547953711271589, -342.7603882486318412 ) ) ;
#49110 = CARTESIAN_POINT ( 'NONE',  ( 36.93908527581412216, -283.4248356664701873, -271.3062335397923448 ) ) ;
#49111 = CARTESIAN_POINT ( 'NONE',  ( 20.55527005517390293, -274.6693526733768067, -315.9736327882210389 ) ) ;
#49112 = CARTESIAN_POINT ( 'NONE',  ( 192.9182251362765328, 275.0000000000000568, 16.22085278731029945 ) ) ;
#49113 = CYLINDRICAL_SURFACE ( 'NONE', #51673, 5.000000000000000888 ) ;
#49114 = CARTESIAN_POINT ( 'NONE',  ( -100.3272692630247604, -278.7719550302677476, -314.3722177343089470 ) ) ;
#49115 = VERTEX_POINT ( 'NONE', #87206 ) ;
#49116 = ORIENTED_EDGE ( 'NONE', *, *, #2076, .F. ) ;
#49117 = CARTESIAN_POINT ( 'NONE',  ( 175.2296996224750103, 134.0000000000000284, 24.00000000000001066 ) ) ;
#49118 = CARTESIAN_POINT ( 'NONE',  ( -93.16339709568981675, -285.8291524398680963, -320.9998585473391017 ) ) ;
#49119 = CARTESIAN_POINT ( 'NONE',  ( 18.08809796983242535, -293.4280714735289166, -318.1310194508695872 ) ) ;
#49120 = EDGE_CURVE ( 'NONE', #27913, #20475, #75428, .T. ) ;
#49121 = CARTESIAN_POINT ( 'NONE',  ( 35.84818837399613045, -287.1978113967840613, -293.9524936863486460 ) ) ;
#49122 = CARTESIAN_POINT ( 'NONE',  ( -16.87038407043041843, -284.5598833568400323, -199.1815926201236095 ) ) ;
#49124 = CARTESIAN_POINT ( 'NONE',  ( 21.97231311791058062, -286.4049401136632014, -314.6522005231041135 ) ) ;
#49123 = CARTESIAN_POINT ( 'NONE',  ( -97.83000789474490944, -283.7064039238655369, -228.4277605393226054 ) ) ;
#49125 = CARTESIAN_POINT ( 'NONE',  ( 22.14270585578276140, -283.3556974694646442, -313.3795724948092243 ) ) ;
#49126 = CARTESIAN_POINT ( 'NONE',  ( 21.21329987222718216, -272.9073229016873938, -223.4759093354347215 ) ) ;
#49127 = CARTESIAN_POINT ( 'NONE',  ( -37.95534399401411463, -284.4444628814347880, -194.1635861345968976 ) ) ;
#49128 = CARTESIAN_POINT ( 'NONE',  ( -67.39993049667045000, -299.6582395602201814, -201.5925882785752776 ) ) ;
#49129 = CARTESIAN_POINT ( 'NONE',  ( -106.2353503082650406, -282.9460941968366114, -240.1695816952180564 ) ) ;
#49130 = CARTESIAN_POINT ( 'NONE',  ( -19.48876145229224477, -281.2285886096219656, -199.2827438418755150 ) ) ;
#49131 = CARTESIAN_POINT ( 'NONE',  ( 21.53947659948623539, -288.9115637224510351, -223.6176472908123571 ) ) ;
#49132 = DIRECTION ( 'NONE',  ( -0.000000000000000000, -1.000000000000000000, -0.000000000000000000 ) ) ;
#49133 = CARTESIAN_POINT ( 'NONE',  ( 170.4537599243631405, 275.0000000000000568, -23.52000000000000313 ) ) ;
#49134 = CARTESIAN_POINT ( 'NONE',  ( -8.906817434781190812, -296.6034004334743486, -340.4220638305647526 ) ) ;
#49135 = CARTESIAN_POINT ( 'NONE',  ( -111.5983994372167274, -276.6918485240350947, -259.4686532257498470 ) ) ;
#49136 = CARTESIAN_POINT ( 'NONE',  ( -96.27380454153264111, -289.0841801484867233, -319.6883841592798490 ) ) ;
#49137 = CARTESIAN_POINT ( 'NONE',  ( -31.55978762442567032, -293.3779524982520002, -343.9849407873743417 ) ) ;
#49138 = CARTESIAN_POINT ( 'NONE',  ( -4.109692083600355872, -279.1846349974526902, -204.7965626360831095 ) ) ;
#49139 = CARTESIAN_POINT ( 'NONE',  ( -90.24877788817013879, -271.3763951383644439, -217.9955250806533229 ) ) ;
#49140 = CARTESIAN_POINT ( 'NONE',  ( 34.42778658241596190, -294.6592285785947638, -254.4794508867490492 ) ) ;
#49141 = CARTESIAN_POINT ( 'NONE',  ( -85.33152481854862970, -287.9090924074130839, -210.2361428286348826 ) ) ;
#49142 = CARTESIAN_POINT ( 'NONE',  ( -110.9285790518850519, -294.7768201939189794, -290.5521804639286643 ) ) ;
#49143 = CARTESIAN_POINT ( 'NONE',  ( 16.60957983065679500, -289.8693134514361986, -320.7916479551012685 ) ) ;
#49144 = CARTESIAN_POINT ( 'NONE',  ( -6.280375931710404203, -290.6944730099417598, -200.9988491171323517 ) ) ;
#49145 = VECTOR ( 'NONE', #31231, 1000.000000000000000 ) ;
#49146 = CARTESIAN_POINT ( 'NONE',  ( -97.02596226968955762, -291.3801880719717019, -313.4095066944574910 ) ) ;
#49147 = CARTESIAN_POINT ( 'NONE',  ( 175.2296996224750103, 20.99999999999998934, 25.00000000000000355 ) ) ;
#49148 = CARTESIAN_POINT ( 'NONE',  ( -72.71396675743028482, -292.3741618894063095, -206.2619765764734154 ) ) ;
#49149 = CARTESIAN_POINT ( 'NONE',  ( 104.2209783822911646, -299.5541904835127980, -195.3611179825600175 ) ) ;
#49150 = CARTESIAN_POINT ( 'NONE',  ( -107.3621537013787162, -291.3572299554362530, -301.5583013647922712 ) ) ;
#49152 = CARTESIAN_POINT ( 'NONE',  ( -0.09095052937821483663, -292.5628401401612564, -207.5806938494377505 ) ) ;
#49151 = CARTESIAN_POINT ( 'NONE',  ( 30.89209248614742975, -279.9920850561903194, -302.4614010193409968 ) ) ;
#49153 = CARTESIAN_POINT ( 'NONE',  ( 23.74730553436537051, -280.9266612193979427, -223.4659889627629070 ) ) ;
#49154 = CARTESIAN_POINT ( 'NONE',  ( -111.4722552536914293, -283.9588377413188027, -291.1073245836867613 ) ) ;
#49155 = AXIS2_PLACEMENT_3D ( 'NONE', #29879, #58763, #87605 ) ;
#49156 = CARTESIAN_POINT ( 'NONE',  ( -75.67640438035840589, -287.5647585583109844, -334.6449780943910923 ) ) ;
#49157 = CARTESIAN_POINT ( 'NONE',  ( 23.13327050988670308, -279.1003461945784352, -227.3071587224978600 ) ) ;
#49158 = CARTESIAN_POINT ( 'NONE',  ( -70.16728794738936870, -283.6194677676351148, -202.9261015755886888 ) ) ;
#49159 = DIRECTION ( 'NONE',  ( 0.000000000000000000, 1.000000000000000000, -0.000000000000000000 ) ) ;
#49160 = CARTESIAN_POINT ( 'NONE',  ( -9.099565082630544310, -278.8947312874761337, -199.4732518768447562 ) ) ;
#49161 = TOROIDAL_SURFACE ( 'NONE', #23477, 2.103083949679977582, 2.000000000000000000 ) ;
#49162 = CARTESIAN_POINT ( 'NONE',  ( 34.56917776149460764, -286.1341763958552633, -243.7093234773917061 ) ) ;
#49163 = LINE ( 'NONE', #34025, #76384 ) ;
#49164 = CARTESIAN_POINT ( 'NONE',  ( 29.45401654481353759, -294.7315408916153388, -238.8594921247345439 ) ) ;
#49165 = CARTESIAN_POINT ( 'NONE',  ( 23.15512436067898250, -276.3494060077114796, -223.6628461444487073 ) ) ;
#49166 = CARTESIAN_POINT ( 'NONE',  ( -109.5136063674918603, -278.0724289027510849, -281.4653260391751814 ) ) ;
#49167 = CARTESIAN_POINT ( 'NONE',  ( -98.34956489679777292, -291.3459372703922554, -223.3606332760649025 ) ) ;
#49168 = CARTESIAN_POINT ( 'NONE',  ( -96.06894653456953392, -281.9820175020212218, -317.9253823626308417 ) ) ;
#49169 = CARTESIAN_POINT ( 'NONE',  ( -110.4798827387940747, -289.6720697204048633, -265.7087646233287614 ) ) ;
#49170 = CARTESIAN_POINT ( 'NONE',  ( -71.19469432189183067, -293.4989171445441229, -337.2862659958021823 ) ) ;
#49171 = EDGE_LOOP ( 'NONE', ( #34726, #73801 ) ) ;
#49172 = CARTESIAN_POINT ( 'NONE',  ( 152.6002739434462399, 20.65727164547140760, 10.65122728701363464 ) ) ;
#49173 = CARTESIAN_POINT ( 'NONE',  ( -38.89260454416110946, -291.5398259189723831, -197.3160419175862899 ) ) ;
#49174 = CARTESIAN_POINT ( 'NONE',  ( -102.0172624299487154, -276.4809262143062369, -239.1787733560258289 ) ) ;
#49175 = CARTESIAN_POINT ( 'NONE',  ( -97.15544886054213691, -296.2577419959949907, -222.2452611705070353 ) ) ;
#49176 = CARTESIAN_POINT ( 'NONE',  ( 28.67382479035883591, -280.1832238765678085, -307.6466859644883129 ) ) ;
#49177 = CARTESIAN_POINT ( 'NONE',  ( -107.7665951037462264, -285.4828190352072852, -300.3902620803494301 ) ) ;
#49178 = CARTESIAN_POINT ( 'NONE',  ( 32.27423283835092604, -287.0937559301826809, -248.3506084061936861 ) ) ;
#49179 = CARTESIAN_POINT ( 'NONE',  ( 20.57931060041919125, -277.7091043712395049, -315.9430999488069460 ) ) ;
#49180 = CARTESIAN_POINT ( 'NONE',  ( -69.24267329968802187, -293.4939513421193737, -337.8597861783933354 ) ) ;
#49181 = CARTESIAN_POINT ( 'NONE',  ( -70.15342174942310294, -297.2507374106174325, -336.7039016190236680 ) ) ;
#49182 = CARTESIAN_POINT ( 'NONE',  ( -18.93208968318285201, -275.6047359527323692, -341.4119219677253341 ) ) ;
#49183 = ORIENTED_EDGE ( 'NONE', *, *, #85799, .T. ) ;
#49184 = CARTESIAN_POINT ( 'NONE',  ( 195.5501422583016904, 40.28162780827879885, 13.79047839948404786 ) ) ;
#49185 = CARTESIAN_POINT ( 'NONE',  ( -84.17570399533069292, -295.3427602249360575, -331.5210473798308044 ) ) ;
#49186 = CARTESIAN_POINT ( 'NONE',  ( 28.31181303545864836, -289.9425791577672271, -305.5555103011849383 ) ) ;
#49187 = CARTESIAN_POINT ( 'NONE',  ( -35.71110069026453004, -296.0724073071932594, -195.3616651891954064 ) ) ;
#49188 = CARTESIAN_POINT ( 'NONE',  ( -8.170200181195644618, -289.3112761448499555, -337.4444557185789790 ) ) ;
#49189 = ORIENTED_EDGE ( 'NONE', *, *, #61048, .T. ) ;
#49190 = CARTESIAN_POINT ( 'NONE',  ( -7.616997862642444161, -279.4911197246729557, -199.5707153718254858 ) ) ;
#49191 = CARTESIAN_POINT ( 'NONE',  ( -88.53138469905071872, -296.3990029082412434, -327.8165643881372944 ) ) ;
#49192 = CARTESIAN_POINT ( 'NONE',  ( -111.0663494786645629, -288.4690682680628697, -287.8804222091131919 ) ) ;
#49193 = CARTESIAN_POINT ( 'NONE',  ( -74.59240837974009253, -295.8667219565606956, -337.7864496464563899 ) ) ;
#49194 = CARTESIAN_POINT ( 'NONE',  ( 33.13822410391224338, -294.1381844362985589, -289.5049464147945173 ) ) ;
#49195 = CARTESIAN_POINT ( 'NONE',  ( 198.0307558930329037, 68.10103061380198142, -9.048247235950418244 ) ) ;
#49196 = FACE_OUTER_BOUND ( 'NONE', #1670, .T. ) ;
#49197 = CARTESIAN_POINT ( 'NONE',  ( 184.7149167944524493, -12.49482340714361506, 13.00000000000000178 ) ) ;
#49198 = CARTESIAN_POINT ( 'NONE',  ( 31.07444624205723827, -289.5118094743826305, -304.2729300940271742 ) ) ;
#49199 = CARTESIAN_POINT ( 'NONE',  ( 40.65961533371913106, -278.2662352645559167, -288.1317622949166548 ) ) ;
#49200 = CARTESIAN_POINT ( 'NONE',  ( 31.93324942420514745, -280.4705606480367237, -236.8575417386156516 ) ) ;
#49201 = CARTESIAN_POINT ( 'NONE',  ( 2.088426583040009277, -284.5235453671684240, -334.0242595690198755 ) ) ;
#49202 = CARTESIAN_POINT ( 'NONE',  ( 21.64695662328472991, -285.4693332063245066, -221.7921498064391699 ) ) ;
#49203 = CARTESIAN_POINT ( 'NONE',  ( -98.54655273510253721, -288.0528547896117288, -312.7542694945253743 ) ) ;
#49204 = CARTESIAN_POINT ( 'NONE',  ( -7.046488210190877233, -278.5193210699403608, -339.8194104634520727 ) ) ;
#49205 = ORIENTED_EDGE ( 'NONE', *, *, #18309, .F. ) ;
#49207 = CARTESIAN_POINT ( 'NONE',  ( -22.16515713726739634, -279.6001634413627812, -198.7999905016983462 ) ) ;
#49206 = CARTESIAN_POINT ( 'NONE',  ( -107.1166226041311376, -278.2658977376094640, -291.9887221695387893 ) ) ;
#49208 = CARTESIAN_POINT ( 'NONE',  ( -35.70426938834810926, -278.1117608034664386, -347.0475956436979459 ) ) ;
#49209 = CARTESIAN_POINT ( 'NONE',  ( -111.0625828863430797, -277.0848660179694889, -291.1755400136414664 ) ) ;
#49210 = CARTESIAN_POINT ( 'NONE',  ( -40.88237375196717949, -139.0235881544214465, -362.1721031521604459 ) ) ;
#49211 = CARTESIAN_POINT ( 'NONE',  ( -90.01016813982198528, -274.2713533787037363, -214.4418274450818274 ) ) ;
#49212 = ITEM_DEFINED_TRANSFORMATION ( 'NONE', 'NONE', #65816,  #18940 ) ;
#49213 = CARTESIAN_POINT ( 'NONE',  ( -37.27248207896832355, -299.4782701078396485, -193.9495680680081193 ) ) ;
#49214 = EDGE_CURVE ( 'NONE', #19412, #93585, #43211, .T. ) ;
#49215 = CARTESIAN_POINT ( 'NONE',  ( -54.49178911615187815, -282.3376638359844719, -195.3683826091709363 ) ) ;
#49216 = VERTEX_POINT ( 'NONE', #29479 ) ;
#49217 = CARTESIAN_POINT ( 'NONE',  ( 175.2296996224750103, 150.9142415853029036, -22.83127060016886034 ) ) ;
#49218 = CARTESIAN_POINT ( 'NONE',  ( 20.57645075312527183, -288.0014731788448898, -225.4198911066196445 ) ) ;
#49219 = CARTESIAN_POINT ( 'NONE',  ( -43.60538776689624285, -287.7343192976260298, -194.5804915227278400 ) ) ;
#49220 = CARTESIAN_POINT ( 'NONE',  ( -29.16995199311165265, -288.2944427489298391, -343.0048733955921421 ) ) ;
#49221 = CARTESIAN_POINT ( 'NONE',  ( -81.53134274645626078, -283.1430784093630564, -333.4084919218286700 ) ) ;
#49222 = CARTESIAN_POINT ( 'NONE',  ( 11.85410503779443125, -279.1492084297348129, -215.3500902929334302 ) ) ;
#49223 = CARTESIAN_POINT ( 'NONE',  ( -10.32210001801530375, -288.2689450926400241, -201.2039874693329864 ) ) ;
#49224 = CARTESIAN_POINT ( 'NONE',  ( -4.016879618372591665, -278.9797202015645325, -204.6191383521114915 ) ) ;
#49225 = CARTESIAN_POINT ( 'NONE',  ( -7.290784495181046765, -277.9647077617255491, -337.4296348058483659 ) ) ;
#49226 = CARTESIAN_POINT ( 'NONE',  ( -85.14077061281625447, -278.2252856588017949, -325.6842358528556360 ) ) ;
#49227 = CARTESIAN_POINT ( 'NONE',  ( 25.51704155755779624, -286.9297003222523585, -314.2332990256165317 ) ) ;
#49228 = COLOUR_RGB ( '',0.7921568627450980005, 0.8196078431372548767, 0.9333333333333333481 ) ;
#49229 = CARTESIAN_POINT ( 'NONE',  ( -47.22544400801635334, -283.9775268795589227, -346.5613176351404832 ) ) ;
#49230 = CARTESIAN_POINT ( 'NONE',  ( -101.3644475367764954, -284.4813648353229496, -313.1253625659184650 ) ) ;
#49231 = CARTESIAN_POINT ( 'NONE',  ( 28.97179329763490330, -281.3056288400366611, -239.7191616712284485 ) ) ;
#49232 = ORIENTED_EDGE ( 'NONE', *, *, #30767, .T. ) ;
#49233 = ORIENTED_EDGE ( 'NONE', *, *, #11598, .T. ) ;
#49234 = DIRECTION ( 'NONE',  ( 0.000000000000000000, 0.9681751575201845705, -0.2502735790305593011 ) ) ;
#49235 = CARTESIAN_POINT ( 'NONE',  ( -111.1199614985169575, -292.6316394586439174, -253.1252938378680710 ) ) ;
#49236 = CARTESIAN_POINT ( 'NONE',  ( -36.36771406311004995, -290.7489564975377903, -193.8475175711297425 ) ) ;
#49237 = CARTESIAN_POINT ( 'NONE',  ( -105.6313159127634691, -271.9649432963055915, -243.7649708839908556 ) ) ;
#49238 = EDGE_CURVE ( 'NONE', #42443, #70, #35514, .T. ) ;
#49239 = CARTESIAN_POINT ( 'NONE',  ( -3.281404455394420605, -293.9628268995140843, -339.3192226677529675 ) ) ;
#49240 = CARTESIAN_POINT ( 'NONE',  ( -107.6191108771980254, -288.7388302356640111, -292.7064533077071928 ) ) ;
#49241 = CARTESIAN_POINT ( 'NONE',  ( 33.71685718705287371, -292.0626699972600591, -291.1106181194548412 ) ) ;
#49242 = CARTESIAN_POINT ( 'NONE',  ( -21.02622964997116028, -290.0431767370299099, -341.9218329502278380 ) ) ;
#49243 = CARTESIAN_POINT ( 'NONE',  ( 99.44099354567467230, -302.2645883696979467, -195.3030568020281521 ) ) ;
#49244 = CARTESIAN_POINT ( 'NONE',  ( -77.05520120966228603, -291.5840230157716633, -334.0443139884949915 ) ) ;
#49245 = CARTESIAN_POINT ( 'NONE',  ( -89.49512086895755658, -289.3196994208087744, -216.1589757877136435 ) ) ;
#49246 = CARTESIAN_POINT ( 'NONE',  ( -100.2445566975779059, -293.1040255495365727, -229.4241609441090475 ) ) ;
#49247 = CARTESIAN_POINT ( 'NONE',  ( -19.77097385643332217, -287.2249183327063520, -199.2648591100277145 ) ) ;
#49248 = CARTESIAN_POINT ( 'NONE',  ( 37.77570333207331288, -295.5871765842871355, -273.0821694437856877 ) ) ;
#49249 = CARTESIAN_POINT ( 'NONE',  ( -114.3482646169705674, -272.5982171866134536, -270.3617045005363480 ) ) ;
#49250 = CARTESIAN_POINT ( 'NONE',  ( 175.2296996224750103, 275.5000000000000568, 0.000000000000000000 ) ) ;
#49251 = CARTESIAN_POINT ( 'NONE',  ( 8.489571720350356898, -276.6562200302269048, -210.5455571263578634 ) ) ;
#49252 = CARTESIAN_POINT ( 'NONE',  ( -86.30030961089215680, -294.9091377980266770, -329.5828486015593626 ) ) ;
#49253 = CARTESIAN_POINT ( 'NONE',  ( -32.60408444673965533, -272.3525055224150719, -196.4868649115544770 ) ) ;
#49254 = CARTESIAN_POINT ( 'NONE',  ( -98.85223252442033015, -276.0600179606722691, -312.2868690514748664 ) ) ;
#49255 = CARTESIAN_POINT ( 'NONE',  ( 95.51333995075087557, -301.0646807905992546, -196.8375845645956588 ) ) ;
#49256 = CARTESIAN_POINT ( 'NONE',  ( -13.23107632313859661, -272.9340728762614958, -197.8539865288538238 ) ) ;
#49257 = EDGE_CURVE ( 'NONE', #92829, #41691, #42170, .T. ) ;
#49258 = CARTESIAN_POINT ( 'NONE',  ( -104.4666997236304127, -297.5729298646509733, -300.6453423370959399 ) ) ;
#49259 = DIRECTION ( 'NONE',  ( 0.000000000000000000, -1.000000000000000000, 0.000000000000000000 ) ) ;
#49260 = CARTESIAN_POINT ( 'NONE',  ( -108.6366949056745739, -297.5711199410398535, -253.9408424904898709 ) ) ;
#49262 = CARTESIAN_POINT ( 'NONE',  ( -41.86834226397009928, -297.9935230211907538, -197.5015989684078477 ) ) ;
#49261 = CARTESIAN_POINT ( 'NONE',  ( 11.04123961856805991, -284.7376718077125020, -212.5219273896025811 ) ) ;
#49263 = CARTESIAN_POINT ( 'NONE',  ( -3.489356550369109744, -286.4866871607825942, -201.1872173472987697 ) ) ;
#49264 = CARTESIAN_POINT ( 'NONE',  ( -65.44326090546300634, -289.0762355400047454, -342.0836633563843634 ) ) ;
#49265 = CARTESIAN_POINT ( 'NONE',  ( -98.59949036658522914, -299.1262371542309779, -226.4761554149631024 ) ) ;
#49266 = CARTESIAN_POINT ( 'NONE',  ( 4.829037383091367985, -292.4808522074100665, -332.1806725105772102 ) ) ;
#49267 = CARTESIAN_POINT ( 'NONE',  ( -6.286237524601067328, -279.6470145315262243, -200.0637538910139881 ) ) ;
#49268 = CARTESIAN_POINT ( 'NONE',  ( -85.28047601435908120, -282.9094976428775681, -210.1954327657594206 ) ) ;
#49269 = CYLINDRICAL_SURFACE ( 'NONE', #71112, 5.000000000000000888 ) ;
#49270 = CARTESIAN_POINT ( 'NONE',  ( 26.03118902092522546, -286.8537637568193190, -307.4886777664013948 ) ) ;
#49271 = DIRECTION ( 'NONE',  ( 1.000000000000000000, 0.000000000000000000, 0.000000000000000000 ) ) ;
#49272 = CARTESIAN_POINT ( 'NONE',  ( -100.5404131816323030, -288.0083156826877371, -310.7458095915461058 ) ) ;
#49273 = CARTESIAN_POINT ( 'NONE',  ( 96.20670667332062465, -301.3513922989450293, -196.5240784471901634 ) ) ;
#49274 = CARTESIAN_POINT ( 'NONE',  ( -64.54962249166925403, -281.1292334848691894, -198.9026848043201312 ) ) ;
#49276 = CARTESIAN_POINT ( 'NONE',  ( 13.92468116014686963, -282.3085731703355350, -322.4011092763580564 ) ) ;
#49275 = CARTESIAN_POINT ( 'NONE',  ( -109.2382278915457476, -294.2820011147274499, -292.9719442165803684 ) ) ;
#49277 = CARTESIAN_POINT ( 'NONE',  ( -114.1209986064743305, -296.7999800278627731, -263.8725706023754469 ) ) ;
#49278 = CARTESIAN_POINT ( 'NONE',  ( -94.24548768623192530, -274.6332888950271354, -223.6794988190263496 ) ) ;
#49279 = CARTESIAN_POINT ( 'NONE',  ( 37.29067828820828367, -283.6540100242638687, -278.2813320565020376 ) ) ;
#49280 = CARTESIAN_POINT ( 'NONE',  ( -110.0395646704508437, -295.4890986399194617, -279.6237507618450877 ) ) ;
#49281 = DIRECTION ( 'NONE',  ( 0.000000000000000000, 0.000000000000000000, 1.000000000000000000 ) ) ;
#49282 = CARTESIAN_POINT ( 'NONE',  ( -21.00420178891176093, -284.8215222325350737, -343.2492770160816917 ) ) ;
#49283 = FACE_OUTER_BOUND ( 'NONE', #2827, .T. ) ;
#49284 = CARTESIAN_POINT ( 'NONE',  ( -37.37352853689063181, -286.5523547857347353, -345.3611179825600175 ) ) ;
#49285 = CARTESIAN_POINT ( 'NONE',  ( -22.97913104049548849, -276.0702068303619399, -345.8994609378297014 ) ) ;
#49286 = CARTESIAN_POINT ( 'NONE',  ( -33.50631320998932949, -291.9350573156178825, -197.4494501609347310 ) ) ;
#49287 = CARTESIAN_POINT ( 'NONE',  ( 16.34411708659709461, -283.7928447098638571, -320.9178358879467510 ) ) ;
#49288 = AXIS2_PLACEMENT_3D ( 'NONE', #4587, #70419, #33950 ) ;
#49289 = CARTESIAN_POINT ( 'NONE',  ( 29.80556030941353640, -276.7424239733973650, -239.6159136246452590 ) ) ;
#49290 = CARTESIAN_POINT ( 'NONE',  ( -113.0132238756227423, -285.8390894433941867, -281.3373609543272096 ) ) ;
#49291 = CARTESIAN_POINT ( 'NONE',  ( -108.4818575970703876, -283.1099788768923986, -288.4223610517784664 ) ) ;
#49292 = CARTESIAN_POINT ( 'NONE',  ( -110.4296838251088957, -280.3355224867646598, -287.2449320147026128 ) ) ;
#49293 = CARTESIAN_POINT ( 'NONE',  ( -83.58178668456264404, -273.6044625959950736, -208.7244688315625183 ) ) ;
#49294 = CARTESIAN_POINT ( 'NONE',  ( 16.95372047719630970, -276.1380398866648989, -325.0341703442957169 ) ) ;
#49295 = CARTESIAN_POINT ( 'NONE',  ( 34.13966513139777703, -295.7423709774723193, -291.1850664419484360 ) ) ;
#49296 = CARTESIAN_POINT ( 'NONE',  ( 180.7287904564219332, 249.5000000000000568, -24.90000000000002345 ) ) ;
#49297 = EDGE_CURVE ( 'NONE', #2535, #39182, #17973, .T. ) ;
#49298 = DIRECTION ( 'NONE',  ( 0.000000000000000000, 0.000000000000000000, -1.000000000000000000 ) ) ;
#49299 = CARTESIAN_POINT ( 'NONE',  ( -105.3933162352427360, -295.1264214598473927, -237.0552172594741194 ) ) ;
#49300 = CARTESIAN_POINT ( 'NONE',  ( 35.16635195036931805, -275.1834271174261630, -279.7404480648376648 ) ) ;
#49301 = CARTESIAN_POINT ( 'NONE',  ( 3.869287891386177680, -296.0286083279678451, -334.6445354065239712 ) ) ;
#49302 = CARTESIAN_POINT ( 'NONE',  ( -19.36549193832724569, -296.0310787375668724, -344.8795710410058177 ) ) ;
#49303 = CARTESIAN_POINT ( 'NONE',  ( -99.84448409623446707, -293.1101111241127342, -229.1156338941977424 ) ) ;
#49304 =( REPRESENTATION_RELATIONSHIP ('NONE','NONE', #78428, #67633 ) REPRESENTATION_RELATIONSHIP_WITH_TRANSFORMATION ( #13249 )SHAPE_REPRESENTATION_RELATIONSHIP( ) );
#49305 = CARTESIAN_POINT ( 'NONE',  ( -77.35715088523424754, -275.5895855800703771, -333.6580764922073854 ) ) ;
#49306 = CARTESIAN_POINT ( 'NONE',  ( -109.2041406534285102, -280.2207571825831565, -289.7802796998409463 ) ) ;
#49307 = CARTESIAN_POINT ( 'NONE',  ( -110.5629126595498093, -294.4575359338207363, -283.8470796261016176 ) ) ;
#49308 = CARTESIAN_POINT ( 'NONE',  ( 38.29766792498102745, -283.4785496407121173, -275.5522773263807608 ) ) ;
#49309 = CARTESIAN_POINT ( 'NONE',  ( -74.86657584358310658, -284.4600258705754072, -207.3840604443440441 ) ) ;
#49310 = CARTESIAN_POINT ( 'NONE',  ( 199.0839727162727115, 283.4321579852195896, -111.4451161440015596 ) ) ;
#49311 = ORIENTED_EDGE ( 'NONE', *, *, #82549, .F. ) ;
#49312 = CARTESIAN_POINT ( 'NONE',  ( -107.4134080596330847, -283.9466203996772151, -290.9494618193027691 ) ) ;
#49313 = EDGE_LOOP ( 'NONE', ( #84002, #13725, #70050 ) ) ;
#49314 = CARTESIAN_POINT ( 'NONE',  ( 39.31128206412358850, -282.6620961325044163, -272.7720990991858230 ) ) ;
#49315 = CARTESIAN_POINT ( 'NONE',  ( -113.8130298055446303, -283.2802780066679134, -275.6748678080809896 ) ) ;
#49316 = CARTESIAN_POINT ( 'NONE',  ( -103.3971930608186085, -278.9811672193897039, -309.5740526285790679 ) ) ;
#49317 = CARTESIAN_POINT ( 'NONE',  ( -108.0070055901374673, -279.7032373881422700, -299.1556027865092915 ) ) ;
#49318 = CARTESIAN_POINT ( 'NONE',  ( -14.26626197960825415, -280.9950113884769962, -196.9511055558885744 ) ) ;
#49319 = CARTESIAN_POINT ( 'NONE',  ( -82.08285599513421005, -270.9094976428775681, -214.2051214447836571 ) ) ;
#49321 = EDGE_CURVE ( 'NONE', #14651, #70449, #21907, .T. ) ;
#49320 = CARTESIAN_POINT ( 'NONE',  ( 104.0975919659984754, 115.9579523938436125, -282.9976511085191078 ) ) ;
#49322 = VERTEX_POINT ( 'NONE', #78731 ) ;
#49323 = CARTESIAN_POINT ( 'NONE',  ( 0.3558082256967267654, -276.5556580839059961, -205.7015479880308533 ) ) ;
#49324 = CARTESIAN_POINT ( 'NONE',  ( 64.32927610681132080, 48.12963783785930616, -318.7087835613883726 ) ) ;
#49325 = CARTESIAN_POINT ( 'NONE',  ( -6.057569129089722004, -278.4854132110050386, -202.5743814259453188 ) ) ;
#49326 = CARTESIAN_POINT ( 'NONE',  ( 1.166968862343012558, -294.3186248787766885, -204.7948394867840420 ) ) ;
#49327 = CARTESIAN_POINT ( 'NONE',  ( 17.15102308680967980, -293.5970225384867263, -319.1081707556673450 ) ) ;
#49328 = CARTESIAN_POINT ( 'NONE',  ( -71.88446366406991217, -289.0041896723178070, -339.1093862574692253 ) ) ;
#49329 = DIRECTION ( 'NONE',  ( -1.000000000000000000, 0.000000000000000000, 0.000000000000000000 ) ) ;
#49331 = CARTESIAN_POINT ( 'NONE',  ( -94.73143348198347269, -283.6013342620691446, -223.9421858382964956 ) ) ;
#49330 = CARTESIAN_POINT ( 'NONE',  ( 8.537774792222245779, -293.0120981470960260, -331.4649646075354212 ) ) ;
#49332 = CARTESIAN_POINT ( 'NONE',  ( -106.8758198994898407, -292.7553319339965014, -244.2175961206301338 ) ) ;
#49333 = CARTESIAN_POINT ( 'NONE',  ( 7.362744667237497431, -285.1537609073272392, -211.7114757675392127 ) ) ;
#49334 = CARTESIAN_POINT ( 'NONE',  ( -108.8492087245877542, -286.0903214198768296, -253.3386690343470491 ) ) ;
#49335 = ORIENTED_EDGE ( 'NONE', *, *, #82962, .F. ) ;
#49336 = CARTESIAN_POINT ( 'NONE',  ( -95.49054990725012715, -292.1723607676894403, -220.2258401223970736 ) ) ;
#49337 = CARTESIAN_POINT ( 'NONE',  ( -13.50336789250761704, -283.2266078969134924, -339.4779459847818543 ) ) ;
#49338 = CARTESIAN_POINT ( 'NONE',  ( -27.81252489032839748, -293.7287728309499357, -346.4220525941694291 ) ) ;
#49339 = CARTESIAN_POINT ( 'NONE',  ( -26.15794092729106879, -289.7160529415188535, -346.3813938979574800 ) ) ;
#49340 = CARTESIAN_POINT ( 'NONE',  ( -48.85359180828439918, -289.6872350485109564, -346.4873740311346637 ) ) ;
#49341 = CARTESIAN_POINT ( 'NONE',  ( 26.36634333461551449, -287.2300712122791424, -234.6166380906255426 ) ) ;
#49342 = VERTEX_POINT ( 'NONE', #57435 ) ;
#49343 = CARTESIAN_POINT ( 'NONE',  ( 195.5941493172114747, 26.57455637838030071, 13.78431146525796791 ) ) ;
#49344 = CARTESIAN_POINT ( 'NONE',  ( -110.0236366759265962, -298.1393170590828277, -291.7993876164754283 ) ) ;
#49345 = CARTESIAN_POINT ( 'NONE',  ( -100.3350459130212045, -295.8141725894475371, -226.9199416932148665 ) ) ;
#49346 = CARTESIAN_POINT ( 'NONE',  ( -41.05115383850343136, -279.0630680189487975, -197.2198273069739116 ) ) ;
#49347 = CARTESIAN_POINT ( 'NONE',  ( -96.88445487593706673, -272.7147279018413428, -221.6149287202791243 ) ) ;
#49348 = CARTESIAN_POINT ( 'NONE',  ( -35.65396063747169109, -293.5105063549002011, -344.0477398844732306 ) ) ;
#49349 = CARTESIAN_POINT ( 'NONE',  ( 24.84784978655136811, -277.8613295289777056, -310.5858722263483855 ) ) ;
#49350 = CARTESIAN_POINT ( 'NONE',  ( -40.53962720997532898, -296.2512795178856777, -196.4041775417347822 ) ) ;
#49351 = CARTESIAN_POINT ( 'NONE',  ( -63.69732051053190958, -296.6084910984629346, -338.9168728220820412 ) ) ;
#49352 = CARTESIAN_POINT ( 'NONE',  ( -55.86820583086120706, -296.3758951696924555, -341.3432250714157021 ) ) ;
#49353 = CARTESIAN_POINT ( 'NONE',  ( 175.2296996224750103, 246.0000000000001137, -9.550761578869391144 ) ) ;
#49354 = CARTESIAN_POINT ( 'NONE',  ( -70.44174824770956889, -297.0812530218202596, -339.0109421419915066 ) ) ;
#49355 = CARTESIAN_POINT ( 'NONE',  ( -94.16796324185864364, -295.2335761247824735, -221.0817999478998672 ) ) ;
#49356 = CARTESIAN_POINT ( 'NONE',  ( -60.29883678888856480, -292.3980457138673046, -200.9043809704727437 ) ) ;
#49357 = CARTESIAN_POINT ( 'NONE',  ( 30.66798256948669987, -299.5341108523645062, -193.4557286876616047 ) ) ;
#49358 = CARTESIAN_POINT ( 'NONE',  ( -94.57390594131445027, -288.4778583820977360, -316.6196257060797166 ) ) ;
#49359 = CARTESIAN_POINT ( 'NONE',  ( -49.21654576272059245, -275.9011149203553259, -196.2545826088790193 ) ) ;
#49360 = CARTESIAN_POINT ( 'NONE',  ( -31.27117788039909030, -274.6192046584260993, -193.6492445006108483 ) ) ;
#49361 = CARTESIAN_POINT ( 'NONE',  ( -77.52715254868695638, -297.8300554375055640, -209.3313719314394064 ) ) ;
#49362 = CARTESIAN_POINT ( 'NONE',  ( -58.85716409511214664, -281.7550661210618728, -198.1427573624997081 ) ) ;
#49363 = CARTESIAN_POINT ( 'NONE',  ( -9.027948151839110480, -279.0996461557298289, -199.2863002059818314 ) ) ;
#49364 = EDGE_CURVE ( 'NONE', #44165, #16501, #82979, .T. ) ;
#49365 = CARTESIAN_POINT ( 'NONE',  ( -35.90942285938511702, -282.3832550318252856, -347.2589454746797060 ) ) ;
#49366 = CARTESIAN_POINT ( 'NONE',  ( 36.39335892120758587, -275.1754757295692571, -292.2353815850151477 ) ) ;
#49367 = CARTESIAN_POINT ( 'NONE',  ( 38.61589809767567516, -279.8752741457325897, -264.2879239529505071 ) ) ;
#49368 = CARTESIAN_POINT ( 'NONE',  ( 37.36374049901815653, -279.4396171921135874, -261.5898087648716910 ) ) ;
#49369 = ADVANCED_FACE ( 'NONE', ( #7679 ), #58523, .F. ) ;
#49370 = CARTESIAN_POINT ( 'NONE',  ( -38.07012738008141639, -272.6175739945053920, -196.7754922617695570 ) ) ;
#49371 = CARTESIAN_POINT ( 'NONE',  ( -106.8900582768564789, -280.1848723049914156, -298.5698349694508806 ) ) ;
#49372 = CARTESIAN_POINT ( 'NONE',  ( 212.7238915819278589, 32.98517505407394168, 10.50000000000000000 ) ) ;
#49373 = PLANE ( 'NONE',  #23252 ) ;
#49374 = CARTESIAN_POINT ( 'NONE',  ( -51.58835398563933694, -296.1123386876454333, -195.6683190004872301 ) ) ;
#49375 = CARTESIAN_POINT ( 'NONE',  ( -6.535770833326606244, -290.4747575874213794, -201.5764878373796307 ) ) ;
#49376 = CARTESIAN_POINT ( 'NONE',  ( -92.81208482793789472, -291.2839303038761045, -216.8808019135353504 ) ) ;
#49377 = CARTESIAN_POINT ( 'NONE',  ( -2.299288039690894792, -278.5896319226638411, -336.8596727356722340 ) ) ;
#49378 = CARTESIAN_POINT ( 'NONE',  ( -38.07709782766258400, -272.0427788392063349, -195.3647191135007972 ) ) ;
#49379 = CARTESIAN_POINT ( 'NONE',  ( 193.6552470326849686, 250.4202232226204785, 16.89672165344822830 ) ) ;
#49380 = CARTESIAN_POINT ( 'NONE',  ( 1.377635955367124465, -284.4592333065026537, -335.2466110531629511 ) ) ;
#49381 = CARTESIAN_POINT ( 'NONE',  ( 209.8602183316602066, 37.94571256237730239, 12.08763307006258536 ) ) ;
#49382 = CARTESIAN_POINT ( 'NONE',  ( -110.1424918677905396, -282.7841634197175154, -252.2796705929992811 ) ) ;
#49383 = SHAPE_REPRESENTATION ( 'High-Pressure Air Hose', ( #18940 ), #6864 ) ;
#49384 = CARTESIAN_POINT ( 'NONE',  ( 154.7659666677267865, 20.47222690886501439, -12.53936336329526391 ) ) ;
#49385 = CARTESIAN_POINT ( 'NONE',  ( -67.47217027397731215, -294.2513306055011526, -337.3023629795414422 ) ) ;
#49386 = CARTESIAN_POINT ( 'NONE',  ( 33.48507799939267926, -285.9835405036366183, -292.7678768272236880 ) ) ;
#49387 = CARTESIAN_POINT ( 'NONE',  ( 154.1407330040854333, 275.5000000000000568, -13.42592592592594158 ) ) ;
#49388 = CARTESIAN_POINT ( 'NONE',  ( 4.923005535238533348, -292.4808522086966605, -332.3183233885110894 ) ) ;
#49389 = CARTESIAN_POINT ( 'NONE',  ( -107.5964409500042649, -282.6479794078484815, -300.2785676423941368 ) ) ;
#49390 = CARTESIAN_POINT ( 'NONE',  ( -16.71745902260857264, -281.9231969900390027, -199.5015308242051333 ) ) ;
#49391 = CARTESIAN_POINT ( 'NONE',  ( -113.9302915993236667, -285.7976385458368327, -267.1464569531382836 ) ) ;
#49392 = CARTESIAN_POINT ( 'NONE',  ( 36.20529224966779225, -280.0342637357871354, -289.4612208169772316 ) ) ;
#49393 = CARTESIAN_POINT ( 'NONE',  ( 31.84059427389619756, -287.2426492264644935, -247.0628317520643407 ) ) ;
#49394 =( BOUNDED_SURFACE ( )  B_SPLINE_SURFACE ( 3, 2, ( 
 ( #33297, #76404, #12465 ),
 ( #4889, #61280, #83957 ),
 ( #25266, #90560, #41312 ),
 ( #69290, #62686, #75920 ),
 ( #91519, #55565, #11045 ),
 ( #34249, #39915, #63155 ),
 ( #68836, #18629, #3964 ),
 ( #91986, #82558, #53691 ),
 ( #93396, #14811, #65483 ),
 ( #34711, #35656, #64094 ),
 ( #20030, #86749, #64571 ),
 ( #20519, #28095, #48907 ),
 ( #14355, #42731, #56982 ),
 ( #36107, #77809, #63625 ) ),
 .UNSPECIFIED., .F., .F., .F. ) 
 B_SPLINE_SURFACE_WITH_KNOTS ( ( 4, 2, 2, 2, 2, 2, 4 ),
 ( 3, 3 ),
 ( 1.986477369973489893, 2.275256190877565921, 2.564035011781641504, 2.708424422233679074, 2.852813832685717088, 2.997203243137755102, 3.141592653589793116 ),
 ( 0.000000000000000000, 1.000000000000000000 ),
 .UNSPECIFIED. ) 
 GEOMETRIC_REPRESENTATION_ITEM ( )  RATIONAL_B_SPLINE_SURFACE ( (
 ( 1.000000000000000000, 0.9583671019092235843, 1.000000000000000000),
 ( 1.000000000000000000, 0.9398658125636398797, 1.000000000000000000),
 ( 1.000000000000000000, 0.9157002655845836170, 1.000000000000000000),
 ( 1.000000000000000000, 0.8622678315320960740, 1.000000000000000000),
 ( 1.000000000000000000, 0.8329613673158866582, 1.000000000000000000),
 ( 1.000000000000000000, 0.7919708659745643420, 1.000000000000000000),
 ( 1.000000000000000000, 0.7788285231914600093, 1.000000000000000000),
 ( 1.000000000000000000, 0.7549177526734387467, 1.000000000000000000),
 ( 1.000000000000000000, 0.7441566529437995126, 1.000000000000000000),
 ( 1.000000000000000000, 0.7262859251462967514, 1.000000000000000000),
 ( 1.000000000000000000, 0.7191857644035031250, 1.000000000000000000),
 ( 1.000000000000000000, 0.7095926089625215205, 1.000000000000000000),
 ( 1.000000000000000000, 0.7070960980132218188, 1.000000000000000000),
 ( 1.000000000000000000, 0.7071067811865473507, 1.000000000000000000) ) ) 
 REPRESENTATION_ITEM ( '' )  SURFACE ( )  );
#49395 = CARTESIAN_POINT ( 'NONE',  ( -104.8043604735452163, -279.5838067122942334, -299.8854042964910604 ) ) ;
#49396 = CARTESIAN_POINT ( 'NONE',  ( -92.84247536346586571, -278.6777971285011972, -318.0294059278054419 ) ) ;
#49397 = CARTESIAN_POINT ( 'NONE',  ( -4.235222826569365218, -288.4662586103927993, -202.6537132561683734 ) ) ;
